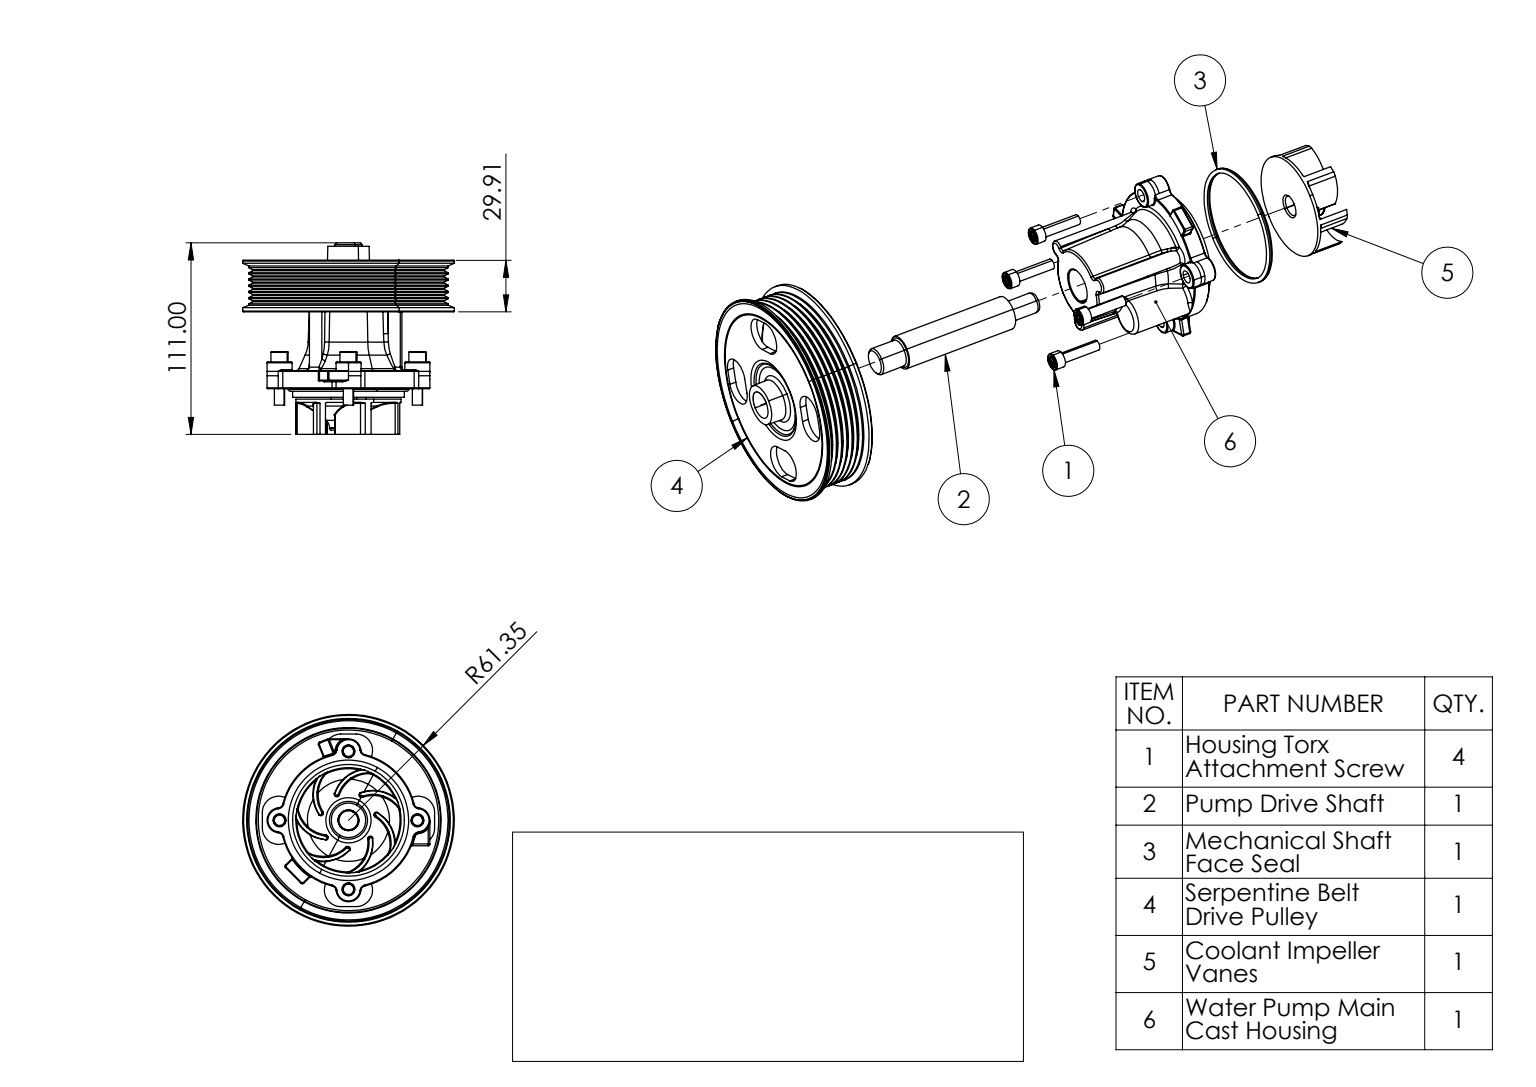
ISO-10303-21;
HEADER;
FILE_DESCRIPTION (('STEP AP214'),
    '1' );
FILE_NAME ('MAS-679',
    '2026-10-09T13:19:41',
    ( '' ),
    ( '' ),
    'SwSTEP 2.0',
    'SolidWorks 2026',
    '' );
FILE_SCHEMA (( 'AUTOMOTIVE_DESIGN' ));
ENDSEC;

DATA;
#1 = CARTESIAN_POINT ( 'NONE',  ( 13.86303783279999990, -99.69348480060000384, -10.38524229410000110 ) ) ;
#2 = DIRECTION ( 'NONE',  ( -1.000000000000000000, 0.000000000000000000, -1.110223024630000146E-15 ) ) ;
#3 = CARTESIAN_POINT ( 'NONE',  ( -4.209215656141860329, -99.16821844303207456, -18.57953415105935946 ) ) ;
#4 = CARTESIAN_POINT ( 'NONE',  ( 36.82697894980000086, -80.49999984420000487, -13.57704391360000074 ) ) ;
#5 = CARTESIAN_POINT ( 'NONE',  ( 11.49840686428493441, -72.20801872445015590, -27.07840416834825348 ) ) ;
#6 = CARTESIAN_POINT ( 'NONE',  ( -18.42950098929999925, -19.15770089200000115, 12.27996177870000061 ) ) ;
#7 = ORIENTED_EDGE ( 'NONE', *, *, #8559, .F. ) ;
#8 = CARTESIAN_POINT ( 'NONE',  ( 11.78548194719999920, -15.31994771319999948, 21.57317999869999881 ) ) ;
#9 = DIRECTION ( 'NONE',  ( 0.4377874319499604483, 0.000000000000000000, 0.8990785084889187928 ) ) ;
#10 = CARTESIAN_POINT ( 'NONE',  ( 6.195449712719999447, -93.01125874769999768, -25.86806793289999717 ) ) ;
#11 = DIRECTION ( 'NONE',  ( 0.000000000000000000, -1.000000000000000000, 0.000000000000000000 ) ) ;
#12 = CARTESIAN_POINT ( 'NONE',  ( -0.4517124965758896882, -92.59735406128710622, -30.49666433008702171 ) ) ;
#13 = APPLICATION_PROTOCOL_DEFINITION ( 'draft international standard', 'automotive_design', 1998, #17800 ) ;
#14 = CARTESIAN_POINT ( 'NONE',  ( 0.000000000000000000, -31.69999999999999929, 0.000000000000000000 ) ) ;
#15 = AXIS2_PLACEMENT_3D ( 'NONE', #13983, #16160, #22740 ) ;
#16 = CARTESIAN_POINT ( 'NONE',  ( 0.000000000000000000, -101.2530993010000060, 0.000000000000000000 ) ) ;
#17 = AXIS2_PLACEMENT_3D ( 'NONE', #8871, #7009, #22746 ) ;
#18 = CIRCLE ( 'NONE', #19870, 0.3500000000000003664 ) ;
#20 = ORIENTED_EDGE ( 'NONE', *, *, #20137, .T. ) ;
#19 = ADVANCED_FACE ( 'NONE', ( #21694 ), #5826, .T. ) ;
#21 = ADVANCED_FACE ( 'NONE', ( #16761 ), #3074, .F. ) ;
#22 = VERTEX_POINT ( 'NONE', #6246 ) ;
#23 = CARTESIAN_POINT ( 'NONE',  ( -13.70187146130000144, -57.41946977620000325, 20.98050236089999743 ) ) ;
#24 = CARTESIAN_POINT ( 'NONE',  ( -21.94602169939999925, -74.00000000000000000, -32.01791432939999993 ) ) ;
#25 = ORIENTED_EDGE ( 'NONE', *, *, #2852, .T. ) ;
#26 = CARTESIAN_POINT ( 'NONE',  ( -13.83118819819999956, -93.00000000000000000, 21.42307711379999802 ) ) ;
#27 = CARTESIAN_POINT ( 'NONE',  ( -6.649694310500000149, -97.57347470069998963, -20.16533349119999841 ) ) ;
#28 = CARTESIAN_POINT ( 'NONE',  ( 7.286238495500000134, -101.2500498790000023, 13.33737010350000141 ) ) ;
#29 = DIRECTION ( 'NONE',  ( 0.000000000000000000, -1.000000000000000000, 0.000000000000000000 ) ) ;
#30 = CARTESIAN_POINT ( 'NONE',  ( -7.249922261819999214, -74.00000000000000000, 40.03357376379999977 ) ) ;
#31 = DIRECTION ( 'NONE',  ( 0.4794255386042040601, 0.000000000000000000, 0.8775825618903720926 ) ) ;
#32 = CARTESIAN_POINT ( 'NONE',  ( 47.25000000000000000, -79.07667144713899177, -0.2614142261083034491 ) ) ;
#33 = ORIENTED_EDGE ( 'NONE', *, *, #25582, .F. ) ;
#34 = CARTESIAN_POINT ( 'NONE',  ( 6.962673371610000217, -93.00000450890000536, -28.64060071930000007 ) ) ;
#35 = CARTESIAN_POINT ( 'NONE',  ( 41.00000000000000000, -82.25000000000000000, -10.20110288159999890 ) ) ;
#36 = DIRECTION ( 'NONE',  ( 0.000000000000000000, 1.000000000000000000, 0.000000000000000000 ) ) ;
#37 = CARTESIAN_POINT ( 'NONE',  ( -13.16349300034329239, -92.74292563041959170, 27.51314017236756015 ) ) ;
#38 = ORIENTED_EDGE ( 'NONE', *, *, #11460, .T. ) ;
#39 = AXIS2_PLACEMENT_3D ( 'NONE', #26145, #6457, #10384 ) ;
#40 = CARTESIAN_POINT ( 'NONE',  ( -38.65569705749999940, -74.00000000000000000, 7.472970580910000216 ) ) ;
#41 = CARTESIAN_POINT ( 'NONE',  ( -14.41816450560000007, -92.76166464580001048, 26.16031912729999931 ) ) ;
#42 = DIRECTION ( 'NONE',  ( 0.4794255386042040601, 0.000000000000000000, 0.8775825618903719816 ) ) ;
#43 = ORIENTED_EDGE ( 'NONE', *, *, #10677, .T. ) ;
#44 = CONICAL_SURFACE ( 'NONE', #19544, 55.67692378859999280, 1.047197551199999799 ) ;
#45 = DIRECTION ( 'NONE',  ( 0.000000000000000000, -1.000000000000000000, 0.000000000000000000 ) ) ;
#46 = CONICAL_SURFACE ( 'NONE', #14894, 2.000000000000000888, 1.308996938999999804 ) ;
#47 = EDGE_CURVE ( 'NONE', #418, #1224, #23072, .T. ) ;
#48 = CARTESIAN_POINT ( 'NONE',  ( 0.8512941674849999751, -100.5027207520000019, -16.22949194299999931 ) ) ;
#49 = CARTESIAN_POINT ( 'NONE',  ( 7.691676892869999449, -59.03425911290000272, -22.18797527670000136 ) ) ;
#50 = CARTESIAN_POINT ( 'NONE',  ( -12.44168150949999863, -68.42644193349998716, -23.76792160109999585 ) ) ;
#51 = CARTESIAN_POINT ( 'NONE',  ( 23.24173891719999929, -63.62917541130000387, -7.733004683649999045 ) ) ;
#52 = CARTESIAN_POINT ( 'NONE',  ( 26.61465604159999998, -68.28989644159999273, 0.1578853838729999959 ) ) ;
#53 = CARTESIAN_POINT ( 'NONE',  ( 40.75609756099999714, -80.50000000000000000, -7.713029007999999465 ) ) ;
#54 = VERTEX_POINT ( 'NONE', #28244 ) ;
#55 = ADVANCED_FACE ( 'NONE', ( #15109 ), #24277, .F. ) ;
#56 = CARTESIAN_POINT ( 'NONE',  ( 28.37844821513105131, -92.77481473400868595, 11.17671000879152565 ) ) ;
#57 = FACE_OUTER_BOUND ( 'NONE', #7313, .T. ) ;
#58 = CARTESIAN_POINT ( 'NONE',  ( -4.347883707720000324, -95.85308664729998895, 22.07540195419999662 ) ) ;
#59 = ORIENTED_EDGE ( 'NONE', *, *, #8938, .T. ) ;
#60 = AXIS2_PLACEMENT_3D ( 'NONE', #11546, #27165, #75 ) ;
#61 = CARTESIAN_POINT ( 'NONE',  ( 23.72908286170881098, -92.68577957607949713, -19.16202722645927281 ) ) ;
#62 = CARTESIAN_POINT ( 'NONE',  ( 18.43702196799999982, -93.96464232210000489, 16.73647664110000122 ) ) ;
#63 = CIRCLE ( 'NONE', #7047, 3.000000000000002665 ) ;
#64 = CIRCLE ( 'NONE', #16341, 0.3500000000000003664 ) ;
#65 = CARTESIAN_POINT ( 'NONE',  ( 19.49531202280000031, -22.51609091130000095, -8.976487791660000326 ) ) ;
#66 = CARTESIAN_POINT ( 'NONE',  ( 22.75333808661257606, -19.47282734142590499, 1.034408943893888599 ) ) ;
#67 = CARTESIAN_POINT ( 'NONE',  ( -7.081475122079999629, -101.0678230150000019, 14.15032671260000008 ) ) ;
#68 = ORIENTED_EDGE ( 'NONE', *, *, #28286, .T. ) ;
#69 = CARTESIAN_POINT ( 'NONE',  ( 26.87524702870645044, -72.43548166874914784, -11.03468220454692883 ) ) ;
#70 = CARTESIAN_POINT ( 'NONE',  ( -13.19299550116862640, -100.0559847774924549, -11.12607270767140477 ) ) ;
#71 = CARTESIAN_POINT ( 'NONE',  ( 8.702528184260000188, -36.35983078039999583, -21.11894135150000196 ) ) ;
#72 = CARTESIAN_POINT ( 'NONE',  ( -37.59243475499999931, -65.56519245710001087, -0.6307174998519999853 ) ) ;
#73 = PLANE ( 'NONE',  #14194 ) ;
#74 = CARTESIAN_POINT ( 'NONE',  ( 22.07903221200000132, -19.15751145089999952, 0.09883320182290000755 ) ) ;
#75 = DIRECTION ( 'NONE',  ( 1.000000000000000000, 0.000000000000000000, 0.000000000000000000 ) ) ;
#76 = DIRECTION ( 'NONE',  ( 0.4794255386042042266, 0.000000000000000000, 0.8775825618903720926 ) ) ;
#77 = VERTEX_POINT ( 'NONE', #6989 ) ;
#78 = CARTESIAN_POINT ( 'NONE',  ( 11.12836528380000090, -101.0356131030000029, -10.75380786670000077 ) ) ;
#79 = CARTESIAN_POINT ( 'NONE',  ( 16.21749840157504963, -94.69376227371040500, 17.23632262694635386 ) ) ;
#80 = CARTESIAN_POINT ( 'NONE',  ( 7.120909764619999412E-15, -73.00000000000000000, 40.00000000000000000 ) ) ;
#81 = EDGE_CURVE ( 'NONE', #22088, #1149, #28672, .T. ) ;
#82 = CARTESIAN_POINT ( 'NONE',  ( 26.66586753799999698, -92.50000000000000000, 13.56661073689999952 ) ) ;
#83 = FACE_OUTER_BOUND ( 'NONE', #27486, .T. ) ;
#84 = DIRECTION ( 'NONE',  ( 1.000000000000000000, 0.000000000000000000, 0.000000000000000000 ) ) ;
#85 = CARTESIAN_POINT ( 'NONE',  ( 21.68645939410062340, -94.27895761509498129, 13.53905968357343781 ) ) ;
#86 = TOROIDAL_SURFACE ( 'NONE', #19140, 38.75000000000000000, 0.5000000000000000000 ) ;
#87 = VERTEX_POINT ( 'NONE', #24762 ) ;
#88 = CIRCLE ( 'NONE', #11209, 30.50000000000000000 ) ;
#89 = CARTESIAN_POINT ( 'NONE',  ( 36.71918983540000880, -74.79610922010000706, -14.73254090590000054 ) ) ;
#90 = VECTOR ( 'NONE', #20251, 1000.000000000000000 ) ;
#91 = EDGE_CURVE ( 'NONE', #19757, #9289, #15248, .T. ) ;
#92 = EDGE_LOOP ( 'NONE', ( #10026, #14439, #14720, #4638 ) ) ;
#93 = CARTESIAN_POINT ( 'NONE',  ( -13.96596450430000047, -64.58097845250000546, 21.73803617189999926 ) ) ;
#94 = CARTESIAN_POINT ( 'NONE',  ( 7.237400523855146872, -74.28469014324819852, 40.42867112560485054 ) ) ;
#95 = CARTESIAN_POINT ( 'NONE',  ( -26.59811871830000030, -93.01125874769999768, -0.2839302173490000358 ) ) ;
#96 = CARTESIAN_POINT ( 'NONE',  ( 27.02683049547185234, -19.50000000000000000, 2.817888817433860993 ) ) ;
#97 = CARTESIAN_POINT ( 'NONE',  ( -13.14566783280000095, -99.53431386179998697, -11.42099844400000030 ) ) ;
#98 = FACE_OUTER_BOUND ( 'NONE', #13994, .T. ) ;
#99 = EDGE_LOOP ( 'NONE', ( #14663, #18599, #4684, #25899 ) ) ;
#100 = CIRCLE ( 'NONE', #13575, 52.20000000000000284 ) ;
#101 = B_SPLINE_CURVE_WITH_KNOTS ( 'NONE', 5,
 ( #4962, #12492, #15099, #10442, #8409, #5814 ),
 .UNSPECIFIED., .F., .F.,
 ( 6, 6 ),
 ( 0.000000000000000000, 1.000000000000000000 ),
 .UNSPECIFIED. ) ;
#102 = CARTESIAN_POINT ( 'NONE',  ( 7.432628554159999013, -73.95638562449998687, -39.04162410920000070 ) ) ;
#103 = VERTEX_POINT ( 'NONE', #2623 ) ;
#104 = AXIS2_PLACEMENT_3D ( 'NONE', #11589, #3684, #25016 ) ;
#105 = DIRECTION ( 'NONE',  ( -0.7071067811865457964, 0.000000000000000000, -0.7071067811865492381 ) ) ;
#106 = ORIENTED_EDGE ( 'NONE', *, *, #502, .T. ) ;
#107 = CARTESIAN_POINT ( 'NONE',  ( -16.95867319479999935, -74.50000000000000000, 44.10460184009999551 ) ) ;
#108 = B_SPLINE_CURVE_WITH_KNOTS ( 'NONE', 3,
 ( #24628, #17928, #4072, #26234, #6261, #26822 ),
 .UNSPECIFIED., .F., .F.,
 ( 4, 2, 4 ),
 ( 0.000000000000000000, 0.5000000000000000000, 1.000000000000000000 ),
 .UNSPECIFIED. ) ;
#109 = CARTESIAN_POINT ( 'NONE',  ( -40.50000000000000000, -63.30468293320000583, -2.309401076760000393 ) ) ;
#110 = CARTESIAN_POINT ( 'NONE',  ( -10.71874886979999886, -18.50000000000000000, -18.09957584549999865 ) ) ;
#111 = PLANE ( 'NONE',  #8405 ) ;
#112 = CARTESIAN_POINT ( 'NONE',  ( 24.26002557130000170, -94.09272382170000526, -9.010767759849999337 ) ) ;
#113 = CARTESIAN_POINT ( 'NONE',  ( -13.91698628299999996, -74.00000000000000000, 36.28539016370000070 ) ) ;
#114 = FACE_OUTER_BOUND ( 'NONE', #18535, .T. ) ;
#115 = CARTESIAN_POINT ( 'NONE',  ( -16.09522089960879399, -99.28262727489575923, 7.457865879375452423 ) ) ;
#116 = B_SPLINE_SURFACE_WITH_KNOTS ( 'NONE', 5, 5, ( 
 ( #14625, #23526, #3562, #12417, #21334, #1390 ),
 ( #10232, #9826, #23801, #19147, #20920, #18734 ),
 ( #5874, #28035, #8074, #16964, #25852, #14753 ),
 ( #26709, #28718, #17525, #19703, #28300, #6299 ),
 ( #19988, #58, #13133, #10789, #8906, #15459 ),
 ( #11070, #6601, #22187, #4412, #6443, #17235 ) ),
 .UNSPECIFIED., .F., .F., .F.,
 ( 6, 6 ),
 ( 6, 6 ),
 ( 15.82769160610000014, 30.79604198849999719 ),
 ( 0.000000000000000000, 0.5000000000000000000 ),
 .UNSPECIFIED. ) ;
#117 = ORIENTED_EDGE ( 'NONE', *, *, #9091, .F. ) ;
#118 = CARTESIAN_POINT ( 'NONE',  ( -15.38823321699999980, -101.6484610359999863, 4.383952149800000697 ) ) ;
#119 = CYLINDRICAL_SURFACE ( 'NONE', #23798, 4.999999999999999112 ) ;
#120 = DIRECTION ( 'NONE',  ( 0.000000000000000000, -1.000000000000000000, 0.000000000000000000 ) ) ;
#121 = PRODUCT_DEFINITION ( 'UNKNOWN', '', #18568, #21393 ) ;
#122 = CARTESIAN_POINT ( 'NONE',  ( 20.98382983661468160, -19.47636826822539646, 9.463978915456744190 ) ) ;
#123 = CARTESIAN_POINT ( 'NONE',  ( 23.35514555854173224, -63.53090568636451962, -7.475128354575953260 ) ) ;
#124 = ORIENTED_EDGE ( 'NONE', *, *, #22234, .T. ) ;
#125 = ADVANCED_FACE ( 'NONE', ( #15853 ), #9081, .F. ) ;
#126 = CARTESIAN_POINT ( 'NONE',  ( 26.73456646982424445, -92.62800705135703083, -14.68054035958608772 ) ) ;
#127 = CARTESIAN_POINT ( 'NONE',  ( -32.18237743670000128, -74.02983596709999858, -21.99383679990000218 ) ) ;
#128 = ORIENTED_EDGE ( 'NONE', *, *, #22826, .F. ) ;
#129 = EDGE_CURVE ( 'NONE', #4293, #10101, #28625, .T. ) ;
#130 = EDGE_CURVE ( 'NONE', #14037, #19059, #13032, .T. ) ;
#131 = CARTESIAN_POINT ( 'NONE',  ( -16.95867319479999935, -79.50000000000000000, 44.10460184009999551 ) ) ;
#132 = CARTESIAN_POINT ( 'NONE',  ( 19.86285231560000142, -35.99517856170000130, -9.398749189900000189 ) ) ;
#133 = CARTESIAN_POINT ( 'NONE',  ( -35.88566914520000495, -79.50000000000000000, -26.69328098980000163 ) ) ;
#134 = VERTEX_POINT ( 'NONE', #18050 ) ;
#135 = ORIENTED_EDGE ( 'NONE', *, *, #7062, .T. ) ;
#136 = CARTESIAN_POINT ( 'NONE',  ( -40.00000000000000000, -69.00000000000000000, 0.000000000000000000 ) ) ;
#137 = CARTESIAN_POINT ( 'NONE',  ( 25.95077523760000204, -92.66001738319999959, 10.56845450099999972 ) ) ;
#138 = CARTESIAN_POINT ( 'NONE',  ( 30.45033996220000105, -72.00000000000000000, 1.805359716810000181 ) ) ;
#139 = VERTEX_POINT ( 'NONE', #26948 ) ;
#140 = CARTESIAN_POINT ( 'NONE',  ( -39.22207447329392238, -63.24690319806988725, -2.469861454400793299 ) ) ;
#141 = CARTESIAN_POINT ( 'NONE',  ( -22.28727701460000077, -80.19684096389998729, -32.37890396869999421 ) ) ;
#142 = TOROIDAL_SURFACE ( 'NONE', #23843, 43.34897771020000334, 20.00000000000000000 ) ;
#143 = AXIS2_PLACEMENT_3D ( 'NONE', #11532, #26560, #20442 ) ;
#144 = LINE ( 'NONE', #2612, #25776 ) ;
#145 = CARTESIAN_POINT ( 'NONE',  ( -12.45428620100000039, -94.22485739629999557, -21.30780079690000406 ) ) ;
#146 = AXIS2_PLACEMENT_3D ( 'NONE', #12009, #28037, #9963 ) ;
#147 = ORIENTED_EDGE ( 'NONE', *, *, #2522, .F. ) ;
#148 = DIRECTION ( 'NONE',  ( 0.000000000000000000, 1.000000000000000000, 0.000000000000000000 ) ) ;
#149 = CARTESIAN_POINT ( 'NONE',  ( -17.00715350810000004, -99.92967567080000890, 3.484608414699999823 ) ) ;
#150 = DIRECTION ( 'NONE',  ( 0.000000000000000000, -1.000000000000000000, 0.000000000000000000 ) ) ;
#151 = CARTESIAN_POINT ( 'NONE',  ( -21.99783282880000002, -74.36373701399999447, -32.65606203760000170 ) ) ;
#152 = DIRECTION ( 'NONE',  ( 0.4794255386042040601, 0.000000000000000000, 0.8775825618903720926 ) ) ;
#153 = CARTESIAN_POINT ( 'NONE',  ( -27.04683438039999999, -80.00000000000000000, -36.23922253580000330 ) ) ;
#154 = CARTESIAN_POINT ( 'NONE',  ( 0.9512194931930000319, -99.70407914540000149, -17.16990763940000164 ) ) ;
#155 = CARTESIAN_POINT ( 'NONE',  ( -18.45398243510000214, -18.61794786970000359, 11.31880357350000033 ) ) ;
#156 = ORIENTED_EDGE ( 'NONE', *, *, #2664, .T. ) ;
#157 = EDGE_CURVE ( 'NONE', #20862, #20652, #26784, .T. ) ;
#158 = CARTESIAN_POINT ( 'NONE',  ( -7.593124578350000320, -94.98812656910000385, -22.45811535680000048 ) ) ;
#159 = CIRCLE ( 'NONE', #18770, 16.00000000000000000 ) ;
#160 = CARTESIAN_POINT ( 'NONE',  ( 9.189959902346380716, -37.98173178281364670, -22.48186365736571801 ) ) ;
#161 = CARTESIAN_POINT ( 'NONE',  ( -23.83924287751435500, -92.80442066021429071, -19.02474555443098936 ) ) ;
#162 = DIRECTION ( 'NONE',  ( 0.000000000000000000, 1.000000000000000000, 0.000000000000000000 ) ) ;
#163 = CARTESIAN_POINT ( 'NONE',  ( -38.62700573890000300, -65.19264941160000149, 2.813424548380000001 ) ) ;
#164 = CARTESIAN_POINT ( 'NONE',  ( -14.62576901236522886, -101.1449112445098564, 4.605366063130757581 ) ) ;
#165 = ADVANCED_FACE ( 'NONE', ( #26356 ), #6385, .F. ) ;
#166 = DIRECTION ( 'NONE',  ( 0.000000000000000000, 0.000000000000000000, 1.000000000000000000 ) ) ;
#167 = CIRCLE ( 'NONE', #27093, 2.000000000000001776 ) ;
#168 = B_SPLINE_CURVE_WITH_KNOTS ( 'NONE', 3,
 ( #1213, #18961, #8023, #3928, #12792, #23335 ),
 .UNSPECIFIED., .F., .F.,
 ( 4, 2, 4 ),
 ( 0.000000000000000000, 0.5000000000000000000, 1.000000000000000000 ),
 .UNSPECIFIED. ) ;
#169 = DIRECTION ( 'NONE',  ( 0.000000000000000000, 1.000000000000000000, 0.000000000000000000 ) ) ;
#170 = CIRCLE ( 'NONE', #22027, 0.8000000000000003775 ) ;
#171 = CARTESIAN_POINT ( 'NONE',  ( 0.000000000000000000, -37.50000000000000000, 0.000000000000000000 ) ) ;
#172 = ORIENTED_EDGE ( 'NONE', *, *, #20476, .T. ) ;
#173 = CARTESIAN_POINT ( 'NONE',  ( 5.151434834259999649E-15, -84.50000000000000000, 40.00000000000000000 ) ) ;
#174 = DIRECTION ( 'NONE',  ( 0.4794255386042042266, 0.000000000000000000, 0.8775825618903720926 ) ) ;
#175 = EDGE_LOOP ( 'NONE', ( #20884, #12154, #22401, #5530, #9489 ) ) ;
#176 = CARTESIAN_POINT ( 'NONE',  ( -12.68423258129999986, -57.45864775709999606, 20.28109956510000345 ) ) ;
#177 = DIRECTION ( 'NONE',  ( 0.000000000000000000, 1.000000000000000000, 0.000000000000000000 ) ) ;
#178 = VERTEX_POINT ( 'NONE', #329 ) ;
#179 = CARTESIAN_POINT ( 'NONE',  ( 16.44117324919999845, -94.63960161729998788, 17.12038106740000032 ) ) ;
#180 = CIRCLE ( 'NONE', #4826, 30.50000000000000000 ) ;
#181 = CARTESIAN_POINT ( 'NONE',  ( 7.155402402981435372, -93.74885977083570765, -25.65720728536609840 ) ) ;
#182 = CARTESIAN_POINT ( 'NONE',  ( -24.61280144410000048, -93.91547326130000783, -2.656926711870000180 ) ) ;
#183 = CARTESIAN_POINT ( 'NONE',  ( 0.000000000000000000, 4.440892098500000496E-16, 0.000000000000000000 ) ) ;
#184 = CARTESIAN_POINT ( 'NONE',  ( -11.05730518689999897, -18.50000000000000000, -18.25363368680000065 ) ) ;
#185 = CARTESIAN_POINT ( 'NONE',  ( 11.60289000694941208, -98.08323605844854853, -16.85433682801441435 ) ) ;
#186 = ORIENTED_EDGE ( 'NONE', *, *, #11011, .T. ) ;
#187 = FACE_OUTER_BOUND ( 'NONE', #28080, .T. ) ;
#188 = DIRECTION ( 'NONE',  ( 0.4794255386042000078, 0.000000000000000000, 0.8775825618903743131 ) ) ;
#189 = CARTESIAN_POINT ( 'NONE',  ( -12.62382144519470906, -92.54938211474033949, 27.76503023812927395 ) ) ;
#190 = ORIENTED_EDGE ( 'NONE', *, *, #2721, .F. ) ;
#191 = EDGE_CURVE ( 'NONE', #3233, #22412, #10451, .T. ) ;
#192 = DIRECTION ( 'NONE',  ( 1.000000000000000000, 0.000000000000000000, 0.000000000000000000 ) ) ;
#193 = CARTESIAN_POINT ( 'NONE',  ( 0.000000000000000000, -23.00000000000000000, 0.000000000000000000 ) ) ;
#194 = CARTESIAN_POINT ( 'NONE',  ( 4.794255386040000566, -108.5000000000000000, 8.775825618900000791 ) ) ;
#195 = ORIENTED_EDGE ( 'NONE', *, *, #12887, .F. ) ;
#196 = EDGE_CURVE ( 'NONE', #27670, #21621, #4916, .T. ) ;
#197 = CARTESIAN_POINT ( 'NONE',  ( 27.03525773600000193, -69.21553441180000732, 0.3672064477150000505 ) ) ;
#198 = CARTESIAN_POINT ( 'NONE',  ( 1.100347978140000071, -100.4792519539999915, -16.15648718290000119 ) ) ;
#199 = CARTESIAN_POINT ( 'NONE',  ( 26.01146028782885011, -74.32246178234187539, -29.34981677889942375 ) ) ;
#200 = CARTESIAN_POINT ( 'NONE',  ( 21.14593590499999820, -36.00000000000000000, -10.72085360310000013 ) ) ;
#201 = EDGE_CURVE ( 'NONE', #9396, #9232, #7255, .T. ) ;
#202 = CARTESIAN_POINT ( 'NONE',  ( -11.49099129190000035, -57.47122623430000488, -20.56185124510000151 ) ) ;
#203 = EDGE_CURVE ( 'NONE', #6901, #22316, #21214, .T. ) ;
#204 = AXIS2_PLACEMENT_3D ( 'NONE', #18687, #25805, #7624 ) ;
#205 = B_SPLINE_CURVE_WITH_KNOTS ( 'NONE', 3,
 ( #6928, #20469, #27325, #4883 ),
 .UNSPECIFIED., .F., .F.,
 ( 4, 4 ),
 ( 0.000000000000000000, 1.000000000000000000 ),
 .UNSPECIFIED. ) ;
#206 = FACE_OUTER_BOUND ( 'NONE', #10971, .T. ) ;
#207 = AXIS2_PLACEMENT_3D ( 'NONE', #10252, #6026, #27775 ) ;
#208 = CYLINDRICAL_SURFACE ( 'NONE', #19119, 0.5000000000000004441 ) ;
#209 = ORIENTED_EDGE ( 'NONE', *, *, #22626, .F. ) ;
#210 = DIRECTION ( 'NONE',  ( 0.000000000000000000, 1.000000000000000000, 0.000000000000000000 ) ) ;
#211 = CARTESIAN_POINT ( 'NONE',  ( 14.90405967080000060, -97.14975741390000508, 15.22359678429999974 ) ) ;
#212 = VERTEX_POINT ( 'NONE', #28690 ) ;
#213 = AXIS2_PLACEMENT_3D ( 'NONE', #15083, #23991, #4026 ) ;
#214 = CARTESIAN_POINT ( 'NONE',  ( 36.70830968599999977, -79.00000000000000000, -14.75000000000000000 ) ) ;
#215 = CARTESIAN_POINT ( 'NONE',  ( 18.38937822269999955, -93.75379239730000336, 16.85123465680000265 ) ) ;
#216 = CARTESIAN_POINT ( 'NONE',  ( 0.000000000000000000, -108.5000000000000000, 0.000000000000000000 ) ) ;
#217 = EDGE_CURVE ( 'NONE', #3543, #26971, #14750, .T. ) ;
#218 = FACE_OUTER_BOUND ( 'NONE', #16317, .T. ) ;
#219 = ORIENTED_EDGE ( 'NONE', *, *, #4229, .F. ) ;
#220 = CARTESIAN_POINT ( 'NONE',  ( -3.592524684419479364, -80.18584070972035249, 46.36824188645663014 ) ) ;
#221 = CARTESIAN_POINT ( 'NONE',  ( -12.45669907782013119, -101.5026031439933831, -10.21990696985948333 ) ) ;
#222 = CARTESIAN_POINT ( 'NONE',  ( 9.433208476599999059, -36.00000000000000000, -19.93952380609999864 ) ) ;
#223 = DIRECTION ( 'NONE',  ( 0.000000000000000000, 1.000000000000000000, 0.000000000000000000 ) ) ;
#224 = CARTESIAN_POINT ( 'NONE',  ( 7.375300558930000250, -99.32951138629999832, 16.07022401509999909 ) ) ;
#225 = AXIS2_PLACEMENT_3D ( 'NONE', #24981, #531, #7212 ) ;
#226 = DIRECTION ( 'NONE',  ( 0.000000000000000000, -1.000000000000000000, 0.000000000000000000 ) ) ;
#227 = CARTESIAN_POINT ( 'NONE',  ( 7.460698725479999927E-15, -73.50000000000000000, 40.00000000000000000 ) ) ;
#228 = AXIS2_PLACEMENT_3D ( 'NONE', #18983, #14038, #961 ) ;
#229 = CARTESIAN_POINT ( 'NONE',  ( 13.12744653600000078, -94.59276292389999696, -19.84842857619999990 ) ) ;
#230 = ORIENTED_EDGE ( 'NONE', *, *, #12077, .T. ) ;
#231 = CYLINDRICAL_SURFACE ( 'NONE', #19067, 8.099999999999997868 ) ;
#232 = CARTESIAN_POINT ( 'NONE',  ( -47.25000000000000000, -77.00000000000000000, 3.352534721190000231E-15 ) ) ;
#233 = CARTESIAN_POINT ( 'NONE',  ( 10.26951296328627450, -97.66504487118385214, 16.98417627201420643 ) ) ;
#234 = EDGE_CURVE ( 'NONE', #8501, #14143, #28325, .T. ) ;
#235 = CARTESIAN_POINT ( 'NONE',  ( 16.83483077069999823, -101.1889999979999999, 4.239603657359999112 ) ) ;
#236 = B_SPLINE_CURVE_WITH_KNOTS ( 'NONE', 5,
 ( #24946, #20125, #22766, #18392, #22315, #639, #13265, #8890, #20574 ),
 .UNSPECIFIED., .F., .F.,
 ( 6, 3, 6 ),
 ( 54.79316277730000451, 55.82679151939999684, 65.31895145690000959 ),
 .UNSPECIFIED. ) ;
#237 = CARTESIAN_POINT ( 'NONE',  ( 21.68248887209999864, -36.72282065030000098, -8.793944725010000241 ) ) ;
#238 = CARTESIAN_POINT ( 'NONE',  ( -13.11191196370000078, -67.01088404460000447, -22.48946444609999773 ) ) ;
#239 = AXIS2_PLACEMENT_3D ( 'NONE', #11995, #25424, #7660 ) ;
#240 = CARTESIAN_POINT ( 'NONE',  ( 14.95019707169999990, -101.2530993000000024, 2.710463435110000319 ) ) ;
#241 = CARTESIAN_POINT ( 'NONE',  ( 47.25000000000000000, -82.25000000000000000, 7.327133149349999745E-15 ) ) ;
#242 = ORIENTED_EDGE ( 'NONE', *, *, #1523, .T. ) ;
#243 = EDGE_CURVE ( 'NONE', #2786, #26473, #23537, .T. ) ;
#244 = DIRECTION ( 'NONE',  ( 1.000000000000000000, 0.000000000000000000, 0.000000000000000000 ) ) ;
#245 = CIRCLE ( 'NONE', #4394, 58.54999999999999716 ) ;
#246 = ORIENTED_EDGE ( 'NONE', *, *, #20790, .F. ) ;
#247 = CARTESIAN_POINT ( 'NONE',  ( -14.67079199249999988, -67.87586507669998070, 22.52608771310000080 ) ) ;
#248 = CARTESIAN_POINT ( 'NONE',  ( -14.08829788499999935, -63.05022673990000470, 21.64331597370000182 ) ) ;
#249 = CARTESIAN_POINT ( 'NONE',  ( 7.244026535080238638, -74.18384006186305157, 40.29424782664090543 ) ) ;
#250 = CIRCLE ( 'NONE', #27231, 57.75000000000000000 ) ;
#251 = B_SPLINE_CURVE_WITH_KNOTS ( 'NONE', 3,
 ( #2695, #18425, #27024, #971, #16075, #16523, #22510, #7208, #16373, #25420, #27617 ),
 .UNSPECIFIED., .F., .F.,
 ( 4, 2, 1, 2, 2, 4 ),
 ( 0.000000000000000000, 0.2499999999999618638, 0.3749999999999487632, 0.4374999999999482636, 0.4999999999999477085, 1.000000000000000000 ),
 .UNSPECIFIED. ) ;
#252 = CARTESIAN_POINT ( 'NONE',  ( 20.27618985420000186, -36.00000000000000000, -9.807089787700000727 ) ) ;
#253 = CARTESIAN_POINT ( 'NONE',  ( 19.26180799268026078, -18.95847994163547767, 10.44830257471190471 ) ) ;
#254 = CARTESIAN_POINT ( 'NONE',  ( -7.325370793560000315, -19.50000000000000000, -24.94672208400000102 ) ) ;
#255 = ADVANCED_FACE ( 'NONE', ( #17790 ), #18406, .F. ) ;
#256 = CARTESIAN_POINT ( 'NONE',  ( 20.51180957029163565, -19.46799463732224922, -8.054242869036199792 ) ) ;
#257 = CARTESIAN_POINT ( 'NONE',  ( 15.94061401059999916, -100.1275643909999928, 4.799433088389999824 ) ) ;
#258 = VERTEX_POINT ( 'NONE', #22459 ) ;
#259 = DIRECTION ( 'NONE',  ( 1.000000000000000000, 0.000000000000000000, 0.000000000000000000 ) ) ;
#260 = FILL_AREA_STYLE_COLOUR ( '', #13962 ) ;
#261 = CARTESIAN_POINT ( 'NONE',  ( -19.90122868539999956, -97.01677120260001175, -7.153572992790000029 ) ) ;
#262 = ORIENTED_EDGE ( 'NONE', *, *, #10555, .F. ) ;
#263 = CARTESIAN_POINT ( 'NONE',  ( -30.47294111744043832, -92.56492639277982448, 1.288063236097679587 ) ) ;
#264 = LINE ( 'NONE', #16101, #15060 ) ;
#265 = CARTESIAN_POINT ( 'NONE',  ( 0.000000000000000000, -26.90310889129999694, 0.000000000000000000 ) ) ;
#266 = CIRCLE ( 'NONE', #3945, 6.749999999999999112 ) ;
#267 = CARTESIAN_POINT ( 'NONE',  ( 20.31209251039999941, -39.36414254479999641, 10.36558011049999983 ) ) ;
#268 = LINE ( 'NONE', #1996, #17176 ) ;
#269 = CARTESIAN_POINT ( 'NONE',  ( -7.237400523910141104, -74.28469014252485181, -40.42867112467618540 ) ) ;
#270 = CARTESIAN_POINT ( 'NONE',  ( 19.55635611740000002, -19.15716910929999628, 10.13489318640000114 ) ) ;
#271 = CARTESIAN_POINT ( 'NONE',  ( -32.83566817454328657, -79.62152845406559720, -22.22906645665674219 ) ) ;
#272 = CARTESIAN_POINT ( 'NONE',  ( -17.52930755215682268, -96.09960287657678180, 13.04485788190981488 ) ) ;
#273 = ORIENTED_EDGE ( 'NONE', *, *, #13276, .F. ) ;
#274 = DIRECTION ( 'NONE',  ( 0.000000000000000000, -1.000000000000000000, 0.000000000000000000 ) ) ;
#275 = CARTESIAN_POINT ( 'NONE',  ( -3.794472973536972216, -98.68740021267650775, 19.30576947772378560 ) ) ;
#276 = CARTESIAN_POINT ( 'NONE',  ( -12.75146816829999885, -100.4650220110000021, -10.99189795709999906 ) ) ;
#277 = CARTESIAN_POINT ( 'NONE',  ( 21.85414229151949073, -19.48999941750866327, 9.596093625701307417 ) ) ;
#278 = CARTESIAN_POINT ( 'NONE',  ( 22.95684285356151122, -62.19234181365079195, -7.315910207710417446 ) ) ;
#279 = ORIENTED_EDGE ( 'NONE', *, *, #17232, .T. ) ;
#280 = CARTESIAN_POINT ( 'NONE',  ( -37.29988270759999835, -74.00000000000000000, -26.69328098980000163 ) ) ;
#281 = ORIENTED_EDGE ( 'NONE', *, *, #28769, .F. ) ;
#282 = CARTESIAN_POINT ( 'NONE',  ( -1.332267629549999902E-15, -101.6484611540000031, 3.552713678799999608E-15 ) ) ;
#283 = CARTESIAN_POINT ( 'NONE',  ( 0.3059185938709999553, -101.1889999979999999, 14.72672055670000013 ) ) ;
#284 = CARTESIAN_POINT ( 'NONE',  ( 10.50737348100000013, -92.95010077049998642, 27.57035790109999596 ) ) ;
#285 = ORIENTED_EDGE ( 'NONE', *, *, #19460, .T. ) ;
#286 = B_SPLINE_CURVE_WITH_KNOTS ( 'NONE', 3,
 ( #13483, #9260, #22391, #17872, #13330, #22237 ),
 .UNSPECIFIED., .F., .F.,
 ( 4, 2, 4 ),
 ( 0.000000000000000000, 0.5000000000000000000, 1.000000000000000000 ),
 .UNSPECIFIED. ) ;
#287 = EDGE_CURVE ( 'NONE', #8306, #13803, #18426, .T. ) ;
#288 = EDGE_LOOP ( 'NONE', ( #10036, #21342, #22222, #19692, #5253 ) ) ;
#289 = CARTESIAN_POINT ( 'NONE',  ( -27.35150891653901084, -93.48480241393187384, -0.1005241429990150898 ) ) ;
#290 = CARTESIAN_POINT ( 'NONE',  ( 19.72730657420000000, -94.57749572790000059, 14.01459989379999982 ) ) ;
#291 = DIRECTION ( 'NONE',  ( 0.000000000000000000, -1.000000000000000000, 0.000000000000000000 ) ) ;
#292 = ORIENTED_EDGE ( 'NONE', *, *, #16592, .T. ) ;
#293 = DIRECTION ( 'NONE',  ( 0.9704142011833033488, 0.000000000000000000, -0.2414462220490755373 ) ) ;
#294 = CARTESIAN_POINT ( 'NONE',  ( -25.34933364415341472, -93.66270333196791853, -5.750320990542998167 ) ) ;
#295 = EDGE_CURVE ( 'NONE', #9549, #16619, #7522, .T. ) ;
#296 = DIRECTION ( 'NONE',  ( -0.2162432783070587228, 0.000000000000000000, -0.9763395129702658881 ) ) ;
#297 = EDGE_CURVE ( 'NONE', #22756, #7089, #25863, .T. ) ;
#298 = CARTESIAN_POINT ( 'NONE',  ( -12.52668430659999999, -94.45168166330000759, -21.51447599709999992 ) ) ;
#299 = CARTESIAN_POINT ( 'NONE',  ( -24.12300379919877713, -94.89420224095245260, -4.133214399626305102 ) ) ;
#300 = VERTEX_POINT ( 'NONE', #17646 ) ;
#301 = EDGE_CURVE ( 'NONE', #178, #23662, #773, .T. ) ;
#302 = CARTESIAN_POINT ( 'NONE',  ( -15.53338745080000116, -84.25000000000000000, -28.43367500519999780 ) ) ;
#303 = CARTESIAN_POINT ( 'NONE',  ( -16.99615325119999909, -99.69348474340000621, 3.341833029000000010 ) ) ;
#304 = CARTESIAN_POINT ( 'NONE',  ( 0.000000000000000000, -18.50000000000000000, 0.000000000000000000 ) ) ;
#305 = CARTESIAN_POINT ( 'NONE',  ( -21.75993564049999662, -74.26505820949999759, -32.61013845149999923 ) ) ;
#306 = CARTESIAN_POINT ( 'NONE',  ( -9.444188748147608337, -96.12507615671063377, -21.04386775914182905 ) ) ;
#307 = DIRECTION ( 'NONE',  ( 0.000000000000000000, 1.000000000000000000, 0.000000000000000000 ) ) ;
#308 = CARTESIAN_POINT ( 'NONE',  ( 0.5505338958400000093, -101.0875971110000080, -15.39929819530000010 ) ) ;
#309 = EDGE_LOOP ( 'NONE', ( #11613, #26788, #16517, #882 ) ) ;
#310 = CARTESIAN_POINT ( 'NONE',  ( -11.92805169729999903, -93.25168459629999518, -23.54816055649999740 ) ) ;
#311 = CARTESIAN_POINT ( 'NONE',  ( 23.49021206360000136, -61.37513324760000444, 10.53893526849999951 ) ) ;
#312 = DIRECTION ( 'NONE',  ( 0.9952295494196654602, 0.000000000000000000, -0.09756097560976667582 ) ) ;
#313 = CARTESIAN_POINT ( 'NONE',  ( -23.96181287727355880, -92.68577957613881324, -18.87019301755865186 ) ) ;
#314 = DIRECTION ( 'NONE',  ( 0.000000000000000000, -1.000000000000000000, 0.000000000000000000 ) ) ;
#315 = CARTESIAN_POINT ( 'NONE',  ( 47.13373881900000129, -79.60558632359999365, -1.850014393339999952 ) ) ;
#316 = AXIS2_PLACEMENT_3D ( 'NONE', #22770, #793, #16190 ) ;
#317 =( NAMED_UNIT ( * ) SI_UNIT ( $, .STERADIAN. ) SOLID_ANGLE_UNIT ( ) );
#318 = CARTESIAN_POINT ( 'NONE',  ( 0.000000000000000000, -11.00000000000000000, 0.000000000000000000 ) ) ;
#319 = ORIENTED_EDGE ( 'NONE', *, *, #5451, .T. ) ;
#320 = CARTESIAN_POINT ( 'NONE',  ( 17.35878545119999927, -99.60591458940000109, 0.7490350149880000696 ) ) ;
#321 = VERTEX_POINT ( 'NONE', #13849 ) ;
#322 = CARTESIAN_POINT ( 'NONE',  ( 22.48431106502128785, -26.11410610478370131, 9.982359961558207928 ) ) ;
#323 = CARTESIAN_POINT ( 'NONE',  ( 32.39999999999999858, -89.50000000000000000, 3.967724586379999025E-15 ) ) ;
#324 = ORIENTED_EDGE ( 'NONE', *, *, #4162, .T. ) ;
#325 = CARTESIAN_POINT ( 'NONE',  ( 0.000000000000000000, -102.8486084350000027, 0.000000000000000000 ) ) ;
#326 = DIRECTION ( 'NONE',  ( 1.000000000000000000, 0.000000000000000000, 0.000000000000000000 ) ) ;
#327 = EDGE_CURVE ( 'NONE', #28629, #9768, #11659, .T. ) ;
#328 = CARTESIAN_POINT ( 'NONE',  ( 4.957296131405555251, -93.25521310932876418, -27.72106811766053980 ) ) ;
#329 = CARTESIAN_POINT ( 'NONE',  ( 32.25000000000000000, -74.00000000000000000, 1.484822157706350179E-15 ) ) ;
#330 = DIRECTION ( 'NONE',  ( -0.9993816408608721114, 0.000000000000000000, 0.03516156865429608674 ) ) ;
#331 = EDGE_CURVE ( 'NONE', #2214, #4550, #8167, .T. ) ;
#332 = CARTESIAN_POINT ( 'NONE',  ( -10.44633092189999957, -19.46971296670000129, -20.02005348129999973 ) ) ;
#333 = ORIENTED_EDGE ( 'NONE', *, *, #19304, .T. ) ;
#334 = ADVANCED_FACE ( 'NONE', ( #7744 ), #22137, .T. ) ;
#335 = CARTESIAN_POINT ( 'NONE',  ( 7.189062418559999834, -92.50000460620000808, -28.89817089330000144 ) ) ;
#336 = CARTESIAN_POINT ( 'NONE',  ( -20.38472824830307317, -61.37133910092857292, 12.44426916512128223 ) ) ;
#337 = CARTESIAN_POINT ( 'NONE',  ( -13.21000303337382675, -92.77521214512354675, 27.49085673672507468 ) ) ;
#338 = ORIENTED_EDGE ( 'NONE', *, *, #4914, .F. ) ;
#339 = CARTESIAN_POINT ( 'NONE',  ( -38.15937129994918564, -63.35495516230771074, -1.162516276375642921 ) ) ;
#340 = CARTESIAN_POINT ( 'NONE',  ( -15.46453744689999965, -92.60980597189998775, 23.68301408729999835 ) ) ;
#341 = CARTESIAN_POINT ( 'NONE',  ( -22.62548402540000225, -71.48510949040000639, 17.99032368389999803 ) ) ;
#342 = ORIENTED_EDGE ( 'NONE', *, *, #9374, .T. ) ;
#343 = CARTESIAN_POINT ( 'NONE',  ( -17.63662366879999865, -94.54719310779999830, 16.06392309460000334 ) ) ;
#344 = CARTESIAN_POINT ( 'NONE',  ( 0.9125455711469999676, -100.1785804069999983, -16.62377051789999882 ) ) ;
#345 = CARTESIAN_POINT ( 'NONE',  ( 25.28766026403006961, -74.25610482756999886, -29.93611247388432162 ) ) ;
#346 = CARTESIAN_POINT ( 'NONE',  ( -19.90266458460165566, -57.44036973094087273, 14.20824301555132152 ) ) ;
#347 = CARTESIAN_POINT ( 'NONE',  ( 22.71963930829999967, -57.44066855169999997, -9.099147364980002095 ) ) ;
#348 = CARTESIAN_POINT ( 'NONE',  ( 6.888451995309999631, -99.53431386179998697, 15.99365561480000153 ) ) ;
#349 = ORIENTED_EDGE ( 'NONE', *, *, #6891, .T. ) ;
#350 = CARTESIAN_POINT ( 'NONE',  ( -17.51528407220000361, -94.37182379849998881, 16.53944417690000179 ) ) ;
#351 = CARTESIAN_POINT ( 'NONE',  ( 15.38595020189201179, -101.1586404113103015, 2.789465265516761772 ) ) ;
#352 = EDGE_CURVE ( 'NONE', #18033, #14401, #4448, .T. ) ;
#353 = CARTESIAN_POINT ( 'NONE',  ( 19.89028060919999774, -94.80026829410000744, 14.17835456439999930 ) ) ;
#354 = ORIENTED_EDGE ( 'NONE', *, *, #12243, .F. ) ;
#355 = CARTESIAN_POINT ( 'NONE',  ( 23.48150327141549099, -92.56772982771099123, -19.46465348493570957 ) ) ;
#356 = DIRECTION ( 'NONE',  ( 0.000000000000000000, 1.000000000000000000, 0.000000000000000000 ) ) ;
#357 = EDGE_CURVE ( 'NONE', #20895, #2845, #5405, .T. ) ;
#358 = B_SPLINE_SURFACE_WITH_KNOTS ( 'NONE', 5, 5, ( 
 ( #10209, #18565, #20758, #23504, #23087, #27741, #25691, #27609, #3542 ),
 ( #25277, #12127, #816, #21309, #7649, #19123, #16212, #964, #25125 ),
 ( #5159, #25412, #3402, #14040, #9658, #22946, #14328, #16367, #23222 ),
 ( #11846, #27457, #5305, #3131, #20898, #16516, #5443, #3270, #21043 ),
 ( #1100, #7777, #16650, #25544, #14467, #23361, #23634, #1928, #28278 ),
 ( #19396, #15144, #19819, #4092, #28424, #23917, #3954, #12678, #10767 ) ),
 .UNSPECIFIED., .F., .F., .F.,
 ( 6, 6 ),
 ( 6, 3, 6 ),
 ( 10.27983419480000116, 28.98451109560000205 ),
 ( 0.000000000000000000, 0.2500000000000000000, 0.5000000000000000000 ),
 .UNSPECIFIED. ) ;
#359 = LINE ( 'NONE', #9205, #7030 ) ;
#360 = ORIENTED_EDGE ( 'NONE', *, *, #15898, .T. ) ;
#361 = DIRECTION ( 'NONE',  ( 0.000000000000000000, -1.000000000000000000, 0.000000000000000000 ) ) ;
#362 = CARTESIAN_POINT ( 'NONE',  ( -12.45203970512436165, -101.4728631013286559, -10.26186846076686443 ) ) ;
#363 = CARTESIAN_POINT ( 'NONE',  ( 8.154561305720001485, -36.99980119890000196, -21.51307946880000088 ) ) ;
#364 = EDGE_CURVE ( 'NONE', #27046, #11872, #7856, .T. ) ;
#365 = CARTESIAN_POINT ( 'NONE',  ( 8.054097215812880961, -19.46843057288947421, -20.48836643782571443 ) ) ;
#366 = ORIENTED_EDGE ( 'NONE', *, *, #9045, .T. ) ;
#367 = AXIS2_PLACEMENT_3D ( 'NONE', #6686, #4637, #15550 ) ;
#368 = ADVANCED_FACE ( 'NONE', ( #27069 ), #19745, .T. ) ;
#369 = CIRCLE ( 'NONE', #15692, 60.85000000000000142 ) ;
#370 = DIRECTION ( 'NONE',  ( 0.000000000000000000, 1.000000000000000000, 0.000000000000000000 ) ) ;
#371 = CARTESIAN_POINT ( 'NONE',  ( -36.70028666173043774, -63.05366661935808992, 0.03681143521525633011 ) ) ;
#372 = DIRECTION ( 'NONE',  ( 0.000000000000000000, 1.000000000000000000, 0.000000000000000000 ) ) ;
#373 = CYLINDRICAL_SURFACE ( 'NONE', #27643, 15.99999999999999822 ) ;
#374 = CARTESIAN_POINT ( 'NONE',  ( -14.95854026159999961, -100.9763033870000015, 4.709388778109999230 ) ) ;
#375 = CARTESIAN_POINT ( 'NONE',  ( -17.31644382271060323, -99.07183861590023355, -8.238310338614811101 ) ) ;
#376 = CARTESIAN_POINT ( 'NONE',  ( -38.31826369283189848, -63.05366661936042050, -2.839229858537526852 ) ) ;
#377 = CONICAL_SURFACE ( 'NONE', #5926, 2.000000000000000888, 1.308996938999999804 ) ;
#378 = CARTESIAN_POINT ( 'NONE',  ( 26.29305724443631220, -63.71690337527751069, 1.488180441977877466 ) ) ;
#379 = CARTESIAN_POINT ( 'NONE',  ( 0.000000000000000000, -101.6484611540000031, 0.000000000000000000 ) ) ;
#380 = CARTESIAN_POINT ( 'NONE',  ( 24.72812962333588160, -93.39299082536693675, -12.36525841036616313 ) ) ;
#381 = CARTESIAN_POINT ( 'NONE',  ( -10.61287167059999881, -19.46510050329999686, 19.30934957549999709 ) ) ;
#382 = ORIENTED_EDGE ( 'NONE', *, *, #3847, .F. ) ;
#383 = CARTESIAN_POINT ( 'NONE',  ( 36.31166979920000415, -74.62997809459999132, -14.90098611910000059 ) ) ;
#384 = CARTESIAN_POINT ( 'NONE',  ( 3.883346862689999845, -2.000000000000000000, 7.108418751309999450 ) ) ;
#385 = AXIS2_PLACEMENT_3D ( 'NONE', #10663, #12718, #21630 ) ;
#386 = CARTESIAN_POINT ( 'NONE',  ( 23.63616061750000341, -94.63960162979999780, -2.179844042860000108 ) ) ;
#387 = CARTESIAN_POINT ( 'NONE',  ( -12.68423313600000135, -57.45864720369999645, 20.28110700490000085 ) ) ;
#388 = CARTESIAN_POINT ( 'NONE',  ( -1.314504061159999897E-13, -19.50000000000000000, -1.119104808819999722E-13 ) ) ;
#389 = CARTESIAN_POINT ( 'NONE',  ( 29.11677867130000052, -92.50000000000000000, 6.880015861159999524 ) ) ;
#390 = CARTESIAN_POINT ( 'NONE',  ( 18.71434861636577907, -18.49999996077436037, 10.15134080778569370 ) ) ;
#391 = ADVANCED_FACE ( 'NONE', ( #7256 ), #13212, .F. ) ;
#392 = B_SPLINE_CURVE_WITH_KNOTS ( 'NONE', 5,
 ( #381, #18132, #9225, #11262, #10956, #27029 ),
 .UNSPECIFIED., .F., .F.,
 ( 6, 6 ),
 ( 0.000000000000000000, 1.000000000000000000 ),
 .UNSPECIFIED. ) ;
#393 = CARTESIAN_POINT ( 'NONE',  ( 16.66712582699999956, -100.0994409990000094, 4.341523580040000496 ) ) ;
#394 = ORIENTED_EDGE ( 'NONE', *, *, #12962, .T. ) ;
#395 = CARTESIAN_POINT ( 'NONE',  ( -7.253647055860000137, -74.31845592130000000, -40.32201634399999790 ) ) ;
#396 = CARTESIAN_POINT ( 'NONE',  ( 30.63887047069549752, -74.17816095543288668, -24.34389095944435155 ) ) ;
#397 = EDGE_CURVE ( 'NONE', #15581, #14037, #15975, .T. ) ;
#398 = AXIS2_PLACEMENT_3D ( 'NONE', #25664, #5557, #14574 ) ;
#399 = CARTESIAN_POINT ( 'NONE',  ( -20.09682587570000223, -97.23151480800000002, -7.274462301079999804 ) ) ;
#400 = VERTEX_POINT ( 'NONE', #13649 ) ;
#401 = CARTESIAN_POINT ( 'NONE',  ( -30.44002477821454633, -92.69183043801065480, 1.913949942781201674 ) ) ;
#402 = DIRECTION ( 'NONE',  ( 0.6184463001828860440, 0.000000000000000000, 0.7858270635388550085 ) ) ;
#403 = DIRECTION ( 'NONE',  ( 0.4794255386042042266, 0.000000000000000000, 0.8775825618903720926 ) ) ;
#404 = DIRECTION ( 'NONE',  ( 0.000000000000000000, 0.000000000000000000, -1.000000000000000000 ) ) ;
#405 = CARTESIAN_POINT ( 'NONE',  ( 7.670973119660000172, -34.59820496239999699, -21.21808926809999818 ) ) ;
#406 = CARTESIAN_POINT ( 'NONE',  ( 22.78264864029999970, -94.59276292120000562, -6.873201003520000185 ) ) ;
#407 = TOROIDAL_SURFACE ( 'NONE', #6924, 18.14285714289999873, 0.5000000000000000000 ) ;
#408 = DIRECTION ( 'NONE',  ( 0.000000000000000000, 1.000000000000000000, 0.000000000000000000 ) ) ;
#409 = CARTESIAN_POINT ( 'NONE',  ( -1.598721155459999804E-14, -84.50000000000000000, 7.105427357599999217E-15 ) ) ;
#410 = CARTESIAN_POINT ( 'NONE',  ( 13.82833792859999811, -99.73367660430000115, -10.41122475269999903 ) ) ;
#411 = ORIENTED_EDGE ( 'NONE', *, *, #8688, .T. ) ;
#412 = CIRCLE ( 'NONE', #28280, 57.75000000000000000 ) ;
#413 = CARTESIAN_POINT ( 'NONE',  ( -12.08584015490000141, -69.49854784190000601, -25.11440668759999895 ) ) ;
#414 = CARTESIAN_POINT ( 'NONE',  ( -9.356041104380000917, -74.50000000000000000, -37.60355029590000697 ) ) ;
#415 = CARTESIAN_POINT ( 'NONE',  ( -13.27698888679999989, -99.83167681540000160, -11.13684395419999973 ) ) ;
#416 = CARTESIAN_POINT ( 'NONE',  ( -12.76745321220000129, -101.1364147039999892, -8.514038431850000421 ) ) ;
#417 = CARTESIAN_POINT ( 'NONE',  ( 16.58537890990000108, -94.98812477769999418, 16.93952572510000110 ) ) ;
#418 = VERTEX_POINT ( 'NONE', #2300 ) ;
#419 = EDGE_CURVE ( 'NONE', #9997, #22379, #25806, .T. ) ;
#420 = CARTESIAN_POINT ( 'NONE',  ( 0.000000000000000000, -90.50000000000000000, 0.000000000000000000 ) ) ;
#421 =( GEOMETRIC_REPRESENTATION_CONTEXT ( 3 ) GLOBAL_UNCERTAINTY_ASSIGNED_CONTEXT ( ( #7445 ) ) GLOBAL_UNIT_ASSIGNED_CONTEXT ( ( #6851, #22443, #317 ) ) REPRESENTATION_CONTEXT ( 'NONE', 'WORKASPACE' ) );
#422 = ORIENTED_EDGE ( 'NONE', *, *, #27436, .F. ) ;
#423 = B_SPLINE_CURVE_WITH_KNOTS ( 'NONE', 5,
 ( #28794, #10856, #8982, #22117, #26629, #17888, #2016, #26198, #19767 ),
 .UNSPECIFIED., .F., .F.,
 ( 6, 3, 6 ),
 ( 0.000000000000000000, 0.2815520576815128129, 1.000000000000000000 ),
 .UNSPECIFIED. ) ;
#424 = CARTESIAN_POINT ( 'NONE',  ( -4.500000000000000000, -11.00000000000000000, 31.00000000000000000 ) ) ;
#425 = B_SPLINE_CURVE_WITH_KNOTS ( 'NONE', 3,
 ( #6749, #17383, #15612, #10933, #24370, #2227, #8482, #26130 ),
 .UNSPECIFIED., .F., .F.,
 ( 4, 2, 2, 4 ),
 ( 0.000000000000000000, 0.5000000000000000000, 0.7500000000000000000, 1.000000000000000000 ),
 .UNSPECIFIED. ) ;
#426 = CARTESIAN_POINT ( 'NONE',  ( -10.50000000000000000, -89.00000000000000000, 6.411537967209999764E-15 ) ) ;
#427 = CARTESIAN_POINT ( 'NONE',  ( 10.51978096080000213, -92.52763213160000078, 27.11043680749999751 ) ) ;
#428 = ORIENTED_EDGE ( 'NONE', *, *, #14886, .F. ) ;
#429 = EDGE_CURVE ( 'NONE', #15620, #8975, #245, .T. ) ;
#430 = CIRCLE ( 'NONE', #7407, 0.4999999999999993339 ) ;
#431 = ORIENTED_EDGE ( 'NONE', *, *, #22851, .T. ) ;
#432 = DIRECTION ( 'NONE',  ( -1.000000000000000000, 0.000000000000000000, -4.565061778886334044E-16 ) ) ;
#433 = DIRECTION ( 'NONE',  ( 0.4151946956541399669, 0.5000000000001689759, 0.7600087925152558821 ) ) ;
#434 = CARTESIAN_POINT ( 'NONE',  ( 47.03393487260000683, -74.30497055530000239, -1.819362492409999810 ) ) ;
#435 = ORIENTED_EDGE ( 'NONE', *, *, #15676, .F. ) ;
#436 = DIRECTION ( 'NONE',  ( -1.224606353819999829E-16, 0.000000000000000000, 1.000000000000000000 ) ) ;
#437 = CARTESIAN_POINT ( 'NONE',  ( -11.33957729739370635, -60.31986010322346203, 20.76858926670032446 ) ) ;
#438 = DIRECTION ( 'NONE',  ( 1.000000000000000000, 0.000000000000000000, 0.000000000000000000 ) ) ;
#439 = CARTESIAN_POINT ( 'NONE',  ( -14.10155798110000092, -93.81709628049999594, -21.57370430179999943 ) ) ;
#440 = CARTESIAN_POINT ( 'NONE',  ( -24.00582547640926379, -94.71481465629901209, -4.132763972591003032 ) ) ;
#441 = ORIENTED_EDGE ( 'NONE', *, *, #13396, .T. ) ;
#442 = CARTESIAN_POINT ( 'NONE',  ( 36.44627168800000305, -74.06782051840001202, -14.22901210950000106 ) ) ;
#443 = CARTESIAN_POINT ( 'NONE',  ( -17.09009608839999927, -99.55609322370000314, 3.193624944930000265 ) ) ;
#444 = CARTESIAN_POINT ( 'NONE',  ( -39.96417052329999819, -74.08839659379999887, 7.268571389559999929 ) ) ;
#445 = CARTESIAN_POINT ( 'NONE',  ( -21.96029098729999873, -74.01681409379999366, -32.14278154310000701 ) ) ;
#446 = ORIENTED_EDGE ( 'NONE', *, *, #18563, .T. ) ;
#448 = TOROIDAL_SURFACE ( 'NONE', #14380, 3.500000000000000000, 0.5000000000000000000 ) ;
#447 = B_SPLINE_CURVE_WITH_KNOTS ( 'NONE', 3,
 ( #7135, #24608, #16144, #11221, #2517, #21773, #21492, #4538, #15745, #9188 ),
 .UNSPECIFIED., .F., .F.,
 ( 4, 2, 2, 2, 4 ),
 ( 0.000000000000000000, 0.2500000000000000000, 0.5000000000000000000, 0.7500000000000000000, 1.000000000000000000 ),
 .UNSPECIFIED. ) ;
#449 = DIRECTION ( 'NONE',  ( 0.000000000000000000, 1.000000000000000000, 0.000000000000000000 ) ) ;
#450 = DIRECTION ( 'NONE',  ( 0.000000000000000000, -1.000000000000000000, 0.000000000000000000 ) ) ;
#451 = CARTESIAN_POINT ( 'NONE',  ( -18.42673315119999700, -19.46723765599999822, 12.71460005940000038 ) ) ;
#452 = VERTEX_POINT ( 'NONE', #2600 ) ;
#453 = CIRCLE ( 'NONE', #16705, 25.14975229270000057 ) ;
#454 = CONICAL_SURFACE ( 'NONE', #1820, 55.67692378859999280, 1.047197551199999799 ) ;
#455 = DIRECTION ( 'NONE',  ( 0.9952295494196655712, 0.000000000000000000, -0.09756097560976655092 ) ) ;
#456 = EDGE_CURVE ( 'NONE', #25924, #731, #15538, .T. ) ;
#457 = AXIS2_PLACEMENT_3D ( 'NONE', #1882, #15240, #28107 ) ;
#458 = CARTESIAN_POINT ( 'NONE',  ( 23.02872706139999792, -64.78279487710000240, 10.89319034239999873 ) ) ;
#459 = CARTESIAN_POINT ( 'NONE',  ( 27.68682485439999752, -17.30000000000000071, 50.68039294919999804 ) ) ;
#460 = CARTESIAN_POINT ( 'NONE',  ( 15.94843830448696487, -101.0147714271772088, 4.203990814596493486 ) ) ;
#461 = CYLINDRICAL_SURFACE ( 'NONE', #14611, 7.250000000000004441 ) ;
#462 = EDGE_LOOP ( 'NONE', ( #7534, #13266, #11753, #16100 ) ) ;
#463 = DIRECTION ( 'NONE',  ( 0.000000000000000000, 1.000000000000000000, 0.000000000000000000 ) ) ;
#464 = CARTESIAN_POINT ( 'NONE',  ( -14.29547445250000060, -74.00000000000000000, 45.69901703040000029 ) ) ;
#465 = B_SPLINE_CURVE_WITH_KNOTS ( 'NONE', 5,
 ( #5943, #23459, #23728, #10162, #18944, #17165, #14693, #26054, #14961, #21544, #25785, #21403 ),
 .UNSPECIFIED., .F., .F.,
 ( 6, 3, 3, 6 ),
 ( 0.000000000000000000, 0.4964111757582199136, 0.7833083924326244007, 1.000000000000000000 ),
 .UNSPECIFIED. ) ;
#466 = CARTESIAN_POINT ( 'NONE',  ( -11.32870268019999926, -60.33034294469999992, -22.21640803110000206 ) ) ;
#467 = ADVANCED_FACE ( 'NONE', ( #20064 ), #15828, .T. ) ;
#468 = CARTESIAN_POINT ( 'NONE',  ( 25.82404717150000195, -69.73911356650000926, -8.782782835009999900 ) ) ;
#469 = DIRECTION ( 'NONE',  ( 1.000000000000000000, 0.000000000000000000, 0.000000000000000000 ) ) ;
#470 = ORIENTED_EDGE ( 'NONE', *, *, #14294, .F. ) ;
#471 = CARTESIAN_POINT ( 'NONE',  ( 7.815970093360001426E-15, -84.50000000000000000, -40.00000000000000000 ) ) ;
#473 = ORIENTED_EDGE ( 'NONE', *, *, #11539, .F. ) ;
#472 = TOROIDAL_SURFACE ( 'NONE', #16728, 1.500000000000000000, 0.5000000000000000000 ) ;
#474 = DIRECTION ( 'NONE',  ( 0.000000000000000000, 1.000000000000000000, 0.000000000000000000 ) ) ;
#475 = CARTESIAN_POINT ( 'NONE',  ( 9.119802927630001221, -98.28914429610000525, 16.69368728350000097 ) ) ;
#476 = EDGE_LOOP ( 'NONE', ( #14422, #15237, #5808, #25954 ) ) ;
#477 = CYLINDRICAL_SURFACE ( 'NONE', #16417, 5.999999999999999112 ) ;
#478 = CIRCLE ( 'NONE', #7895, 3.000000000000000000 ) ;
#479 = CIRCLE ( 'NONE', #4152, 28.68388914670000034 ) ;
#480 = PLANE ( 'NONE',  #18583 ) ;
#481 = DIRECTION ( 'NONE',  ( 0.000000000000000000, 1.000000000000000000, 0.000000000000000000 ) ) ;
#482 = CARTESIAN_POINT ( 'NONE',  ( -10.10487300439999991, -18.62107971969999909, -21.27518202489999766 ) ) ;
#483 = CARTESIAN_POINT ( 'NONE',  ( 21.51792335492191199, -37.40300027226001589, -7.702379948524843201 ) ) ;
#484 = ORIENTED_EDGE ( 'NONE', *, *, #2417, .F. ) ;
#485 = CARTESIAN_POINT ( 'NONE',  ( 11.45574570990000041, -93.13207089280000162, -23.61394595179999811 ) ) ;
#486 = CARTESIAN_POINT ( 'NONE',  ( -20.39638010391581702, -61.43221488831640897, 12.45288284519579314 ) ) ;
#487 = CARTESIAN_POINT ( 'NONE',  ( -13.33479272893357859, -92.93978723899297734, 27.43052168310984840 ) ) ;
#488 = ORIENTED_EDGE ( 'NONE', *, *, #1371, .F. ) ;
#489 = LINE ( 'NONE', #22764, #1160 ) ;
#490 = DIRECTION ( 'NONE',  ( 0.4794255386042036715, 0.000000000000000000, 0.8775825618903724257 ) ) ;
#491 = CARTESIAN_POINT ( 'NONE',  ( 14.34373124439999891, -102.5000000000000000, 26.25602392650000283 ) ) ;
#492 = ORIENTED_EDGE ( 'NONE', *, *, #28617, .F. ) ;
#493 = CARTESIAN_POINT ( 'NONE',  ( -18.48642635659999911, -96.07607726710000406, 13.72266607319999920 ) ) ;
#494 = CARTESIAN_POINT ( 'NONE',  ( 0.6457915530089999301, -99.58396362730000817, -17.35065848859999704 ) ) ;
#495 = CARTESIAN_POINT ( 'NONE',  ( -20.45998242170000125, -52.56313962710000709, 14.78974999389999923 ) ) ;
#496 = CARTESIAN_POINT ( 'NONE',  ( -19.95527577780000072, -57.47855601759999900, 12.14622656770000120 ) ) ;
#497 = PRODUCT_RELATED_PRODUCT_CATEGORY ( 'part', '', ( #13159 ) ) ;
#498 = CARTESIAN_POINT ( 'NONE',  ( 22.40625751809999855, -60.56287431679999855, -8.064917839230000496 ) ) ;
#499 = EDGE_CURVE ( 'NONE', #18811, #12707, #22077, .T. ) ;
#500 = CARTESIAN_POINT ( 'NONE',  ( 27.49606017789999868, -67.46051290640001241, 1.934794646639999893 ) ) ;
#501 = CARTESIAN_POINT ( 'NONE',  ( -10.27945668490000131, -18.50000000000000000, 18.70272521329999904 ) ) ;
#502 = EDGE_CURVE ( 'NONE', #19526, #5924, #14185, .T. ) ;
#503 = EDGE_CURVE ( 'NONE', #1478, #12804, #17430, .T. ) ;
#504 = EDGE_LOOP ( 'NONE', ( #699, #16423, #5514, #12046 ) ) ;
#505 = CARTESIAN_POINT ( 'NONE',  ( 10.20110288159999890, -74.50000000000000000, -41.00000000000000000 ) ) ;
#506 = CARTESIAN_POINT ( 'NONE',  ( -43.20000000000000284, -65.14977478849999670, 0.1732050807559999961 ) ) ;
#507 = B_SPLINE_CURVE_WITH_KNOTS ( 'NONE', 3,
 ( #4002, #15340, #26308, #12728 ),
 .UNSPECIFIED., .F., .F.,
 ( 4, 4 ),
 ( 0.000000000000000000, 1.000000000000000000 ),
 .UNSPECIFIED. ) ;
#508 = CARTESIAN_POINT ( 'NONE',  ( 10.14179094049999819, -99.62155479429999616, 14.52072615979999881 ) ) ;
#509 = EDGE_LOOP ( 'NONE', ( #14292, #25818, #23874, #1797 ) ) ;
#510 = CARTESIAN_POINT ( 'NONE',  ( 7.323170304809999642, -73.87254094300001839, 39.07240670449999698 ) ) ;
#511 = CARTESIAN_POINT ( 'NONE',  ( 26.37318048140000215, -93.00000450890000536, 13.16123783449999962 ) ) ;
#512 = DIRECTION ( 'NONE',  ( 0.000000000000000000, 1.000000000000000000, 0.000000000000000000 ) ) ;
#513 = FACE_OUTER_BOUND ( 'NONE', #18198, .T. ) ;
#514 = CARTESIAN_POINT ( 'NONE',  ( -6.885095864830000245, -101.1417990620000040, 14.17428525849999943 ) ) ;
#515 = CARTESIAN_POINT ( 'NONE',  ( 26.80884837331130655, -72.62863614316471228, -10.52387429041271538 ) ) ;
#516 = CARTESIAN_POINT ( 'NONE',  ( -12.61948338259999858, -101.6484611540000031, -9.836088610590000059 ) ) ;
#517 = CARTESIAN_POINT ( 'NONE',  ( 8.994939661169999212, -36.15004583290000539, -20.77616074780000233 ) ) ;
#518 = CARTESIAN_POINT ( 'NONE',  ( 8.620126422187169624, -19.47938362974832316, -19.97534244429069616 ) ) ;
#519 = VERTEX_POINT ( 'NONE', #424 ) ;
#520 = CIRCLE ( 'NONE', #16773, 5.000000000000000888 ) ;
#521 = CARTESIAN_POINT ( 'NONE',  ( 7.321257786130000333, -99.28585527969998736, 16.15667156069999777 ) ) ;
#522 = CARTESIAN_POINT ( 'NONE',  ( 36.28164458690000060, -74.50000000000000000, -14.97346873880000118 ) ) ;
#523 = CARTESIAN_POINT ( 'NONE',  ( -3.773308002759999891, -96.65227117080000596, -20.92579437230000039 ) ) ;
#524 = CARTESIAN_POINT ( 'NONE',  ( -2.568686407175419184, -19.48618186047746548, -23.50321383691693100 ) ) ;
#525 = CYLINDRICAL_SURFACE ( 'NONE', #18143, 7.249999999999999112 ) ;
#526 = CARTESIAN_POINT ( 'NONE',  ( 5.873292863139999653, -11.55246854740000018, 10.75099047199999980 ) ) ;
#527 = DIRECTION ( 'NONE',  ( 1.000000000000000000, 0.000000000000000000, 0.000000000000000000 ) ) ;
#528 = CARTESIAN_POINT ( 'NONE',  ( -39.10791602276640333, -73.54003775238672347, 7.198125313980217932 ) ) ;
#529 = DIRECTION ( 'NONE',  ( -0.2414462220490760924, 0.000000000000000000, -0.9704142011833030157 ) ) ;
#530 = FACE_OUTER_BOUND ( 'NONE', #1949, .T. ) ;
#531 = DIRECTION ( 'NONE',  ( 0.000000000000000000, 1.000000000000000000, 0.000000000000000000 ) ) ;
#532 = ORIENTED_EDGE ( 'NONE', *, *, #4377, .T. ) ;
#533 = ADVANCED_FACE ( 'NONE', ( #11147 ), #17891, .T. ) ;
#534 = CARTESIAN_POINT ( 'NONE',  ( 36.25731322790000632, -74.69416361989999587, -15.03231676859999943 ) ) ;
#535 = CARTESIAN_POINT ( 'NONE',  ( -22.29222582179728107, -79.74578553650356127, -32.80938733156981613 ) ) ;
#536 = CONICAL_SURFACE ( 'NONE', #26096, 7.000000000000005329, 0.7853981633970000820 ) ;
#537 = AXIS2_PLACEMENT_3D ( 'NONE', #16966, #27223, #1016 ) ;
#538 = EDGE_CURVE ( 'NONE', #11457, #18344, #12745, .T. ) ;
#539 = CIRCLE ( 'NONE', #15843, 30.50000000000000000 ) ;
#540 = CARTESIAN_POINT ( 'NONE',  ( -11.41594931139999858, -19.46510050329999686, -18.84569254350000023 ) ) ;
#541 = CARTESIAN_POINT ( 'NONE',  ( 19.99082350619999815, -35.29518274429999991, -8.963945870050000764 ) ) ;
#542 = CARTESIAN_POINT ( 'NONE',  ( -19.01557598121447157, -92.50000000001456613, 22.91712378798360916 ) ) ;
#543 = CARTESIAN_POINT ( 'NONE',  ( 28.83687378200000140, -92.50000647099999185, 7.262115126140000321 ) ) ;
#544 = DIRECTION ( 'NONE',  ( 0.000000000000000000, -1.000000000000000000, 0.000000000000000000 ) ) ;
#545 = CARTESIAN_POINT ( 'NONE',  ( -19.98788946392987853, -95.81531090358907932, 9.701109111489476078 ) ) ;
#546 = CARTESIAN_POINT ( 'NONE',  ( 27.68682485439999752, -14.30000000000000071, 50.68039294919999804 ) ) ;
#547 = ORIENTED_EDGE ( 'NONE', *, *, #12350, .T. ) ;
#548 = CARTESIAN_POINT ( 'NONE',  ( 21.56931449510000220, -36.56979901409999911, -6.850353628320000610 ) ) ;
#549 = CARTESIAN_POINT ( 'NONE',  ( -24.15517241699999929, -94.98812769030000425, -4.102690932189999806 ) ) ;
#550 = ORIENTED_EDGE ( 'NONE', *, *, #21053, .T. ) ;
#551 = CARTESIAN_POINT ( 'NONE',  ( 8.639505966715979923, -92.69183043846588532, 29.25093587448420962 ) ) ;
#552 = CARTESIAN_POINT ( 'NONE',  ( 0.3872056760440000245, -99.92967571559999840, -17.35614698070000017 ) ) ;
#553 = LINE ( 'NONE', #19920, #16709 ) ;
#554 = DIRECTION ( 'NONE',  ( 1.000000000000000000, 0.000000000000000000, 0.000000000000000000 ) ) ;
#555 = CARTESIAN_POINT ( 'NONE',  ( -40.00000000000000000, -65.00000000000000000, 3.175426480540000096 ) ) ;
#556 = AXIS2_PLACEMENT_3D ( 'NONE', #15444, #1512, #21732 ) ;
#557 = DIRECTION ( 'NONE',  ( 0.9982579106777251798, 0.000000000000000000, -0.05900121837168281064 ) ) ;
#558 = CIRCLE ( 'NONE', #25661, 18.64285714289999873 ) ;
#559 = VECTOR ( 'NONE', #7059, 1000.000000000000000 ) ;
#560 = CARTESIAN_POINT ( 'NONE',  ( -13.82310862920000005, -74.00000000000000000, 36.20061004779999791 ) ) ;
#561 = CARTESIAN_POINT ( 'NONE',  ( -21.72229115340000050, -67.06690763590000870, 14.40139912269999911 ) ) ;
#562 = CARTESIAN_POINT ( 'NONE',  ( 14.21256893470000193, -98.58303758080000989, -12.13706782569999909 ) ) ;
#563 = EDGE_LOOP ( 'NONE', ( #25536, #17511, #4054, #11653 ) ) ;
#565 = EDGE_CURVE ( 'NONE', #21465, #19989, #2562, .T. ) ;
#564 = CARTESIAN_POINT ( 'NONE',  ( -12.47289874710000035, -69.87861895790000233, -24.46965691790000363 ) ) ;
#566 = DIRECTION ( 'NONE',  ( 0.000000000000000000, 1.000000000000000000, 0.000000000000000000 ) ) ;
#567 = CARTESIAN_POINT ( 'NONE',  ( 7.891778559019607009, -101.5538022607323683, 14.00007649551812072 ) ) ;
#568 = DIRECTION ( 'NONE',  ( 0.000000000000000000, -1.000000000000000000, 0.000000000000000000 ) ) ;
#569 = CARTESIAN_POINT ( 'NONE',  ( 7.135467692469593892, -73.63089972761061119, -38.71641001238787538 ) ) ;
#570 = ORIENTED_EDGE ( 'NONE', *, *, #2545, .F. ) ;
#571 = ADVANCED_FACE ( 'NONE', ( #26925 ), #15677, .T. ) ;
#572 = CARTESIAN_POINT ( 'NONE',  ( 26.38387423984804769, -92.80045754842753070, -15.30171679607595259 ) ) ;
#573 = ORIENTED_EDGE ( 'NONE', *, *, #1821, .F. ) ;
#574 = EDGE_CURVE ( 'NONE', #4330, #15463, #9981, .T. ) ;
#575 = DIRECTION ( 'NONE',  ( 0.4794255386042000078, 0.000000000000000000, 0.8775825618903743131 ) ) ;
#576 = CARTESIAN_POINT ( 'NONE',  ( -4.045235864600000397, -98.43722212099999069, 19.19069134749999961 ) ) ;
#577 = VECTOR ( 'NONE', #18094, 1000.000000000000000 ) ;
#578 = CARTESIAN_POINT ( 'NONE',  ( 8.074115162410000934, -92.66424957140000629, 26.74225754210000261 ) ) ;
#579 = VECTOR ( 'NONE', #5626, 999.9999999999998863 ) ;
#580 = ORIENTED_EDGE ( 'NONE', *, *, #6138, .F. ) ;
#581 = CARTESIAN_POINT ( 'NONE',  ( 0.000000000000000000, -37.08699221940000257, 0.000000000000000000 ) ) ;
#582 = CARTESIAN_POINT ( 'NONE',  ( -16.86265888959999870, -79.50000000000000000, 45.21850545039999503 ) ) ;
#583 = CARTESIAN_POINT ( 'NONE',  ( 10.08829703670000022, -36.00000000000000000, -20.49602678049999938 ) ) ;
#584 = VERTEX_POINT ( 'NONE', #13793 ) ;
#585 = CARTESIAN_POINT ( 'NONE',  ( 7.246063797170706700, -73.82871504787716788, -39.75929607700521018 ) ) ;
#586 = CARTESIAN_POINT ( 'NONE',  ( -11.50280172684225732, -61.70151683873936577, 21.01880821135103972 ) ) ;
#587 = ORIENTED_EDGE ( 'NONE', *, *, #16283, .F. ) ;
#588 = CARTESIAN_POINT ( 'NONE',  ( 22.44118743278407280, -65.00127796776330058, 11.39886732859506502 ) ) ;
#589 = EDGE_CURVE ( 'NONE', #21458, #13839, #9040, .T. ) ;
#590 = CARTESIAN_POINT ( 'NONE',  ( 7.367077158260816994, -101.1416252679887577, 13.68480675837215799 ) ) ;
#591 = CARTESIAN_POINT ( 'NONE',  ( -2.675358685650000012, -67.79480919600000277, -26.71434926430000090 ) ) ;
#592 = PLANE ( 'NONE',  #25559 ) ;
#593 = CARTESIAN_POINT ( 'NONE',  ( -15.48552837409999938, -71.82739780379999672, 23.60563397449999812 ) ) ;
#594 = ORIENTED_EDGE ( 'NONE', *, *, #7560, .T. ) ;
#595 = DIRECTION ( 'NONE',  ( 1.000000000000000000, 0.000000000000000000, 0.000000000000000000 ) ) ;
#596 = CARTESIAN_POINT ( 'NONE',  ( -16.91403943069999727, -99.72583475830001021, 3.025870399720000048 ) ) ;
#597 = CARTESIAN_POINT ( 'NONE',  ( 25.46032906830000186, -64.78279197330000727, 0.8694561931790000253 ) ) ;
#598 = CARTESIAN_POINT ( 'NONE',  ( -21.94602169939999925, -74.00000000000000000, -32.01791432939999993 ) ) ;
#599 = ORIENTED_EDGE ( 'NONE', *, *, #25882, .T. ) ;
#600 = CARTESIAN_POINT ( 'NONE',  ( -19.61617179850000170, -45.99935878759999497, 11.93235644279999974 ) ) ;
#601 = VECTOR ( 'NONE', #24406, 1000.000000000000000 ) ;
#602 = CARTESIAN_POINT ( 'NONE',  ( 0.7331063123750001242, -99.53431386179998697, -17.39857302659999760 ) ) ;
#603 = CARTESIAN_POINT ( 'NONE',  ( -18.66344010299999923, -18.85523519099999845, 11.44727505870000073 ) ) ;
#604 = ORIENTED_EDGE ( 'NONE', *, *, #24072, .T. ) ;
#605 = ADVANCED_FACE ( 'NONE', ( #18903 ), #27359, .T. ) ;
#607 = EDGE_CURVE ( 'NONE', #27919, #28507, #7827, .T. ) ;
#606 = CARTESIAN_POINT ( 'NONE',  ( -9.465083148179999739, -93.62676565499999981, -23.38439984080000045 ) ) ;
#608 = DIRECTION ( 'NONE',  ( 0.3388759126238506392, 0.000000000000000000, -0.9408310772095872521 ) ) ;
#609 = CARTESIAN_POINT ( 'NONE',  ( 8.964388214039999525, -35.14340553630000130, -19.96644199109999818 ) ) ;
#610 = CARTESIAN_POINT ( 'NONE',  ( 16.28778070538160350, -100.5550990449209223, 4.345266980774773913 ) ) ;
#611 = DIRECTION ( 'NONE',  ( 0.000000000000000000, 1.000000000000000000, 0.000000000000000000 ) ) ;
#612 = ORIENTED_EDGE ( 'NONE', *, *, #9543, .F. ) ;
#613 = CARTESIAN_POINT ( 'NONE',  ( 47.25000000000000000, -79.00000000000000000, -7.713829575100000215E-13 ) ) ;
#614 = CONTEXT_DEPENDENT_SHAPE_REPRESENTATION ( #13885, #24097 ) ;
#615 = CARTESIAN_POINT ( 'NONE',  ( -11.81677247600000058, -62.06858034060000762, -21.05646513629999816 ) ) ;
#616 = CARTESIAN_POINT ( 'NONE',  ( 25.13747520559999771, -67.81660459209999203, -9.975487151870000346 ) ) ;
#617 = CARTESIAN_POINT ( 'NONE',  ( 9.475766568499999210, -35.50000000000000000, -19.97576656850000276 ) ) ;
#618 = VERTEX_POINT ( 'NONE', #23274 ) ;
#619 = DIRECTION ( 'NONE',  ( 0.000000000000000000, 1.000000000000000000, 0.000000000000000000 ) ) ;
#620 = ORIENTED_EDGE ( 'NONE', *, *, #6006, .F. ) ;
#621 = CARTESIAN_POINT ( 'NONE',  ( 0.000000000000000000, -102.5000000000000000, 0.000000000000000000 ) ) ;
#622 = CARTESIAN_POINT ( 'NONE',  ( 9.335817441747641610, -98.58684426249028832, 16.46450815360437048 ) ) ;
#623 = VERTEX_POINT ( 'NONE', #3318 ) ;
#624 = AXIS2_PLACEMENT_3D ( 'NONE', #1463, #10304, #17029 ) ;
#625 = CARTESIAN_POINT ( 'NONE',  ( -2.579145438419999881, -53.53226321310000202, -25.13754169039999908 ) ) ;
#626 = EDGE_CURVE ( 'NONE', #27517, #13659, #27786, .T. ) ;
#627 = CARTESIAN_POINT ( 'NONE',  ( -22.27191869549999836, -94.59276292389999696, -8.381623179300000004 ) ) ;
#628 = CARTESIAN_POINT ( 'NONE',  ( -10.49491320851042708, -19.48298603870330581, -20.96686108838342832 ) ) ;
#629 = CARTESIAN_POINT ( 'NONE',  ( -18.14789115860000024, -98.53904439360000822, 4.701750000830000609 ) ) ;
#630 = CARTESIAN_POINT ( 'NONE',  ( -0.5455113252076949637, -98.53908159007990264, -18.73906669024530913 ) ) ;
#631 = CARTESIAN_POINT ( 'NONE',  ( 47.24130919904909121, -79.14360025649037311, -0.4895094584727857079 ) ) ;
#632 = EDGE_LOOP ( 'NONE', ( #19632, #17486, #11324, #22339 ) ) ;
#633 = CARTESIAN_POINT ( 'NONE',  ( 13.03263341399999931, -94.63960343439998724, -19.83860458410000049 ) ) ;
#634 = CARTESIAN_POINT ( 'NONE',  ( -20.38860325545200070, -61.39165777032547311, 12.44713039966608292 ) ) ;
#635 = DIRECTION ( 'NONE',  ( 0.000000000000000000, 1.000000000000000000, 0.000000000000000000 ) ) ;
#636 = ORIENTED_EDGE ( 'NONE', *, *, #17902, .T. ) ;
#637 = DIRECTION ( 'NONE',  ( -1.000000000000000000, 0.000000000000000000, 0.000000000000000000 ) ) ;
#638 = CYLINDRICAL_SURFACE ( 'NONE', #9269, 4.999999999999999112 ) ;
#639 = CARTESIAN_POINT ( 'NONE',  ( 7.235472567440000446, -61.68715554919999988, -22.75972229710000150 ) ) ;
#640 = VERTEX_POINT ( 'NONE', #18620 ) ;
#641 = CARTESIAN_POINT ( 'NONE',  ( -18.40263696530000104, -95.90090461900000207, 13.63749173159999906 ) ) ;
#642 = CARTESIAN_POINT ( 'NONE',  ( 0.7331063045040000503, -99.53431386179998697, -17.39857310140000024 ) ) ;
#643 = DIRECTION ( 'NONE',  ( 0.000000000000000000, 1.000000000000000000, 0.000000000000000000 ) ) ;
#644 = CARTESIAN_POINT ( 'NONE',  ( 22.30843460160000191, -36.00000000000000000, -11.28235740200000059 ) ) ;
#645 = CARTESIAN_POINT ( 'NONE',  ( 23.70193923009999892, -61.68490361759999985, -9.613352042829999888 ) ) ;
#646 = VECTOR ( 'NONE', #958, 1000.000000000000000 ) ;
#647 = CARTESIAN_POINT ( 'NONE',  ( 25.12978992150000224, -65.01950800350000748, 0.1513709550449999774 ) ) ;
#648 = DIRECTION ( 'NONE',  ( 1.000000000000000000, 0.000000000000000000, 0.000000000000000000 ) ) ;
#649 = ORIENTED_EDGE ( 'NONE', *, *, #27398, .T. ) ;
#650 = CARTESIAN_POINT ( 'NONE',  ( -19.68803156824991163, -18.87168151093004198, 14.53288012867929702 ) ) ;
#651 = VECTOR ( 'NONE', #20044, 1000.000000000000114 ) ;
#652 = CARTESIAN_POINT ( 'NONE',  ( 8.185345124539999517, -101.3150701389999995, 14.03998254610000096 ) ) ;
#653 = ORIENTED_EDGE ( 'NONE', *, *, #17240, .T. ) ;
#654 = CARTESIAN_POINT ( 'NONE',  ( 7.135467526410000261, -73.50000000000000000, 38.71641004229999794 ) ) ;
#655 = CARTESIAN_POINT ( 'NONE',  ( 7.383549334360000493, -18.50000000000000000, -19.69582310909999734 ) ) ;
#656 = CARTESIAN_POINT ( 'NONE',  ( 23.35112319427650007, -19.48210987405916583, 1.375628917947436136 ) ) ;
#657 = CARTESIAN_POINT ( 'NONE',  ( -7.569816714379999922, -100.7776802639999971, 13.87827956499999971 ) ) ;
#658 = CARTESIAN_POINT ( 'NONE',  ( -12.66558680574216922, -93.40492137171338527, -23.55307789253798845 ) ) ;
#659 = CARTESIAN_POINT ( 'NONE',  ( 9.018047497980001381, -36.17942459150000190, -20.85226661109999924 ) ) ;
#660 = AXIS2_PLACEMENT_3D ( 'NONE', #6377, #25920, #4047 ) ;
#661 = CARTESIAN_POINT ( 'NONE',  ( 7.318052426040000391, -101.1822553929999913, 13.41977313900000013 ) ) ;
#662 = ORIENTED_EDGE ( 'NONE', *, *, #22175, .F. ) ;
#663 = EDGE_CURVE ( 'NONE', #10505, #5317, #25363, .T. ) ;
#664 = CARTESIAN_POINT ( 'NONE',  ( -43.22799762839635918, -65.13413837705087417, 0.1570406424686417168 ) ) ;
#665 = CARTESIAN_POINT ( 'NONE',  ( -36.74605004467864688, -63.06523941402065958, -0.1332336900803410829 ) ) ;
#666 = CARTESIAN_POINT ( 'NONE',  ( 21.48302338326642413, -36.56890885472610364, -7.253824468342653375 ) ) ;
#667 = ORIENTED_EDGE ( 'NONE', *, *, #3117, .T. ) ;
#668 = DIRECTION ( 'NONE',  ( -0.7071067811865470176, 0.000000000000000000, 0.7071067811865480168 ) ) ;
#669 = EDGE_CURVE ( 'NONE', #15395, #12657, #1152, .T. ) ;
#670 = CARTESIAN_POINT ( 'NONE',  ( 11.85549584000000145, -101.3350617309999961, -10.77753387699999976 ) ) ;
#671 = CARTESIAN_POINT ( 'NONE',  ( -0.8441209747499999194, -45.99930305819999887, -22.94698520209999870 ) ) ;
#672 = CARTESIAN_POINT ( 'NONE',  ( 15.48878798707903925, -95.04305759974297985, 17.29288121155813585 ) ) ;
#673 = EDGE_CURVE ( 'NONE', #12096, #23467, #9990, .T. ) ;
#674 = DIRECTION ( 'NONE',  ( 0.000000000000000000, 1.000000000000000000, 0.000000000000000000 ) ) ;
#675 = AXIS2_PLACEMENT_3D ( 'NONE', #1404, #7809, #1680 ) ;
#676 = CARTESIAN_POINT ( 'NONE',  ( 41.00000000000000000, -74.50000000000000000, 10.20110288159999890 ) ) ;
#677 = CARTESIAN_POINT ( 'NONE',  ( 22.20693316850000087, -40.71455396009999816, -8.968806686309999776 ) ) ;
#678 = CARTESIAN_POINT ( 'NONE',  ( 19.97576656849999921, -72.00000000000000000, -19.97576656849999921 ) ) ;
#679 = CARTESIAN_POINT ( 'NONE',  ( -14.88706571849999882, -101.2269841009999993, 3.209819282999999857 ) ) ;
#680 = ORIENTED_EDGE ( 'NONE', *, *, #13024, .F. ) ;
#681 = CARTESIAN_POINT ( 'NONE',  ( 36.59408416780000550, -74.85684975549999365, -14.74361069959999959 ) ) ;
#682 = CARTESIAN_POINT ( 'NONE',  ( -32.66809844459999823, -74.41869006989999491, -22.00101410510000122 ) ) ;
#683 = CARTESIAN_POINT ( 'NONE',  ( -18.13877362739999910, -92.50000000000000000, -23.79298866759999598 ) ) ;
#684 = AXIS2_PLACEMENT_3D ( 'NONE', #27269, #20999, #20718 ) ;
#685 = CARTESIAN_POINT ( 'NONE',  ( 21.27776255609999723, -96.58372173029999885, 1.059637706860000028 ) ) ;
#686 = CARTESIAN_POINT ( 'NONE',  ( 9.004237477329999351, -35.65077419509999146, -19.54737253879999770 ) ) ;
#687 = CARTESIAN_POINT ( 'NONE',  ( 23.18812391385057126, -58.58546841852697895, 10.40058855015711892 ) ) ;
#688 = CARTESIAN_POINT ( 'NONE',  ( 20.11250903250000022, -36.00000000000000000, -9.561259576869998611 ) ) ;
#689 = CARTESIAN_POINT ( 'NONE',  ( 21.16767063019999995, -36.23936169889999803, -8.913590358700000493 ) ) ;
#690 = CARTESIAN_POINT ( 'NONE',  ( 0.4125572470530000091, -92.84292833370000153, -30.36594662649999776 ) ) ;
#691 = CIRCLE ( 'NONE', #4371, 24.76278252470000041 ) ;
#692 = CARTESIAN_POINT ( 'NONE',  ( 16.40194905730000130, -100.1981337080000003, 4.404945126920000398 ) ) ;
#693 = ORIENTED_EDGE ( 'NONE', *, *, #2892, .T. ) ;
#694 = CIRCLE ( 'NONE', #26077, 1.249999999999999112 ) ;
#695 = CARTESIAN_POINT ( 'NONE',  ( 8.185346967789998374, -101.3150701389999995, 14.03998109830000018 ) ) ;
#696 = CARTESIAN_POINT ( 'NONE',  ( -22.25469472199999998, -96.07623048470000526, -5.897558151980000218 ) ) ;
#697 = ORIENTED_EDGE ( 'NONE', *, *, #27258, .F. ) ;
#698 = CARTESIAN_POINT ( 'NONE',  ( -30.48402335599918800, -92.52498922770503498, 0.9899291096564720727 ) ) ;
#699 = ORIENTED_EDGE ( 'NONE', *, *, #16855, .F. ) ;
#700 = EDGE_CURVE ( 'NONE', #27146, #28156, #13733, .T. ) ;
#701 = DIRECTION ( 'NONE',  ( 0.000000000000000000, -1.000000000000000000, 0.000000000000000000 ) ) ;
#702 = DIRECTION ( 'NONE',  ( 0.000000000000000000, 0.000000000000000000, -1.000000000000000000 ) ) ;
#703 = DIRECTION ( 'NONE',  ( 0.000000000000000000, 1.000000000000000000, 0.000000000000000000 ) ) ;
#704 = TOROIDAL_SURFACE ( 'NONE', #18826, 25.11294200180000047, 0.5000000000000000000 ) ;
#705 = CARTESIAN_POINT ( 'NONE',  ( -7.250038883930940870, -73.95086734744796786, -39.95935625309049755 ) ) ;
#706 = ADVANCED_FACE ( 'NONE', ( #3044 ), #14624, .F. ) ;
#707 = CARTESIAN_POINT ( 'NONE',  ( -14.57729759870000130, -74.12911414260001663, 36.26887511289999821 ) ) ;
#708 = CARTESIAN_POINT ( 'NONE',  ( -21.87632299289999693, -67.55173099820000004, 16.08189821899999927 ) ) ;
#709 = CARTESIAN_POINT ( 'NONE',  ( 14.00782577689999897, -96.65227117100000953, -15.99711037630000021 ) ) ;
#710 = ORIENTED_EDGE ( 'NONE', *, *, #14232, .F. ) ;
#711 = CARTESIAN_POINT ( 'NONE',  ( -12.46915732870000149, -70.42119542689999889, -24.73933575500000259 ) ) ;
#712 = CARTESIAN_POINT ( 'NONE',  ( 8.142471319829999388, -22.47117226119999955, -20.59194991089999860 ) ) ;
#713 = DIRECTION ( 'NONE',  ( 0.9295286103719528903, 0.000000000000000000, 0.3687499999999813705 ) ) ;
#714 = CARTESIAN_POINT ( 'NONE',  ( 19.96073932771978221, -19.46608320370787482, 9.833604944531050052 ) ) ;
#715 = CARTESIAN_POINT ( 'NONE',  ( 11.77298154309999845, -101.2530993010000060, -9.604785791470000333 ) ) ;
#716 = ORIENTED_EDGE ( 'NONE', *, *, #14608, .F. ) ;
#717 = CIRCLE ( 'NONE', #12731, 2.000000035459998493 ) ;
#718 = ORIENTED_EDGE ( 'NONE', *, *, #26083, .T. ) ;
#719 = CARTESIAN_POINT ( 'NONE',  ( -2.487950882160000265, -57.83919435140000331, -24.63540447140000111 ) ) ;
#720 = LINE ( 'NONE', #20953, #7524 ) ;
#721 = LINE ( 'NONE', #9422, #6410 ) ;
#722 = CARTESIAN_POINT ( 'NONE',  ( 2.631283596650000334, -94.29487537309999823, 25.29847487550000196 ) ) ;
#723 = VERTEX_POINT ( 'NONE', #5055 ) ;
#724 = CARTESIAN_POINT ( 'NONE',  ( -11.18835776723661724, -94.77533639018899692, -20.78536094536529077 ) ) ;
#725 = CIRCLE ( 'NONE', #16980, 18.64285714289999518 ) ;
#726 = VERTEX_POINT ( 'NONE', #19037 ) ;
#727 = CARTESIAN_POINT ( 'NONE',  ( -26.32546053305905076, -93.86130746203110675, -1.655768764585977548 ) ) ;
#728 = CARTESIAN_POINT ( 'NONE',  ( 21.09474350280000010, -36.06031159909999673, -9.858094216790000530 ) ) ;
#729 = ADVANCED_FACE ( 'NONE', ( #27924 ), #23339, .F. ) ;
#730 = CARTESIAN_POINT ( 'NONE',  ( 47.14031554959999681, -74.51859318479999672, -1.361887490440000015 ) ) ;
#731 = VERTEX_POINT ( 'NONE', #1559 ) ;
#732 = CARTESIAN_POINT ( 'NONE',  ( 7.250349464191871540, -73.96150430845511892, -39.97648509748324130 ) ) ;
#733 = CARTESIAN_POINT ( 'NONE',  ( -11.45517213598250095, -61.33682282352064874, 20.94728758455344675 ) ) ;
#734 = EDGE_CURVE ( 'NONE', #9200, #23505, #24513, .T. ) ;
#735 = CARTESIAN_POINT ( 'NONE',  ( 24.22382764319999993, -64.24504439390000243, 10.76339940740000145 ) ) ;
#736 = CIRCLE ( 'NONE', #10888, 0.3500000000000003664 ) ;
#737 = CARTESIAN_POINT ( 'NONE',  ( -2.901733356760000326, -65.28594186040000125, -26.69036142120000221 ) ) ;
#738 = ADVANCED_FACE ( 'NONE', ( #6191 ), #18923, .F. ) ;
#739 = AXIS2_PLACEMENT_3D ( 'NONE', #22838, #3037, #27350 ) ;
#740 = CYLINDRICAL_SURFACE ( 'NONE', #28427, 5.000000000000000000 ) ;
#741 = ORIENTED_EDGE ( 'NONE', *, *, #6844, .T. ) ;
#742 = EDGE_CURVE ( 'NONE', #12644, #2204, #16508, .T. ) ;
#743 = CARTESIAN_POINT ( 'NONE',  ( 36.61501056740000593, -74.18926003920000767, -14.42630212289999925 ) ) ;
#744 = CARTESIAN_POINT ( 'NONE',  ( -15.62495981729999883, -101.3646851630000043, 3.472370199919999845 ) ) ;
#745 = CARTESIAN_POINT ( 'NONE',  ( 25.05740514639999716, -58.84796781909999908, 1.374148744239999997 ) ) ;
#746 = CARTESIAN_POINT ( 'NONE',  ( -20.94815322850000072, -63.05060005210000185, 15.10280677179999920 ) ) ;
#747 = EDGE_LOOP ( 'NONE', ( #26424, #26914 ) ) ;
#748 = CARTESIAN_POINT ( 'NONE',  ( -40.00000000000000000, -63.00000000000000000, 0.000000000000000000 ) ) ;
#749 = CARTESIAN_POINT ( 'NONE',  ( -13.83118819819999956, -93.00000000000000000, 21.42307711379999802 ) ) ;
#750 = CARTESIAN_POINT ( 'NONE',  ( 36.73784911806745868, -74.38638021456385729, -14.53963971729679017 ) ) ;
#751 = ORIENTED_EDGE ( 'NONE', *, *, #16283, .T. ) ;
#752 = DIRECTION ( 'NONE',  ( 1.000000000000000000, 0.000000000000000000, 0.000000000000000000 ) ) ;
#753 = CARTESIAN_POINT ( 'NONE',  ( 20.73451516309999931, -60.34941021230000047, 11.32693620240000065 ) ) ;
#754 = CARTESIAN_POINT ( 'NONE',  ( -2.664535259099999805E-15, -84.00000000000000000, -40.00000000000000000 ) ) ;
#755 = CARTESIAN_POINT ( 'NONE',  ( 15.63673621517384227, -101.5526869446983511, 3.723052656565844831 ) ) ;
#756 = CARTESIAN_POINT ( 'NONE',  ( -4.459621975350000156, -72.00000000000000000, -28.73485931899999812 ) ) ;
#757 = ORIENTED_EDGE ( 'NONE', *, *, #538, .T. ) ;
#758 = CARTESIAN_POINT ( 'NONE',  ( 46.85840109400000131, -80.01819416290000220, -2.680681327329999863 ) ) ;
#759 = CARTESIAN_POINT ( 'NONE',  ( -11.12510688389999913, -19.15751128430000350, 19.07158749389999741 ) ) ;
#760 = CARTESIAN_POINT ( 'NONE',  ( -12.19871700799999914, -59.03921360480000402, -19.98710743599999873 ) ) ;
#761 = CARTESIAN_POINT ( 'NONE',  ( 37.10328156088058194, -79.93994609586795264, -14.09141366765611636 ) ) ;
#762 = CARTESIAN_POINT ( 'NONE',  ( 24.78973582949999965, -64.24504403269999386, -10.08507979989999903 ) ) ;
#763 = CARTESIAN_POINT ( 'NONE',  ( 2.113568700161239988, -94.60931859130616317, 24.93618714997996122 ) ) ;
#764 = ORIENTED_EDGE ( 'NONE', *, *, #15472, .F. ) ;
#765 = CARTESIAN_POINT ( 'NONE',  ( 25.57735248450000043, -16.00000000000000000, 46.81902967690000139 ) ) ;
#766 = DIRECTION ( 'NONE',  ( -1.000000000000000000, 0.000000000000000000, -1.224606353820000075E-16 ) ) ;
#767 = VERTEX_POINT ( 'NONE', #4884 ) ;
#768 = CARTESIAN_POINT ( 'NONE',  ( 22.78965548680000097, -53.78538132969999452, 10.19408277159999976 ) ) ;
#769 = CARTESIAN_POINT ( 'NONE',  ( -5.360408304419999936, -101.0356131030000029, 14.51726283890000069 ) ) ;
#770 = ORIENTED_EDGE ( 'NONE', *, *, #5118, .F. ) ;
#771 = CARTESIAN_POINT ( 'NONE',  ( 45.89652019488737977, -80.18584073604786511, -4.323399995959095854 ) ) ;
#772 = ADVANCED_FACE ( 'NONE', ( #13764 ), #9092, .T. ) ;
#773 = CIRCLE ( 'NONE', #24460, 7.750000000000000000 ) ;
#774 = ORIENTED_EDGE ( 'NONE', *, *, #17934, .T. ) ;
#775 = FACE_OUTER_BOUND ( 'NONE', #22718, .T. ) ;
#776 = CARTESIAN_POINT ( 'NONE',  ( 40.00000000000000000, -80.50000000000000000, 0.000000000000000000 ) ) ;
#777 = CARTESIAN_POINT ( 'NONE',  ( 13.75178900340000077, -72.82938648530000592, 25.17248092229999656 ) ) ;
#778 = CARTESIAN_POINT ( 'NONE',  ( -10.38787484979999931, -19.16887642500000055, -20.73616781340000159 ) ) ;
#779 = CARTESIAN_POINT ( 'NONE',  ( 46.40218322401350548, -80.00000000000000000, -4.271240362889383135 ) ) ;
#780 = ORIENTED_EDGE ( 'NONE', *, *, #25866, .T. ) ;
#781 = CARTESIAN_POINT ( 'NONE',  ( -32.25831118210000170, -80.18584106479998752, -22.46797580029999963 ) ) ;
#782 = CARTESIAN_POINT ( 'NONE',  ( -20.68567502208468767, -62.76183479546326538, 12.67672343809073254 ) ) ;
#783 = CARTESIAN_POINT ( 'NONE',  ( 46.25000000000000000, -74.00000000000000000, -4.582575694960000057 ) ) ;
#784 = CARTESIAN_POINT ( 'NONE',  ( 15.50655985760000100, -100.4792519539999915, 4.667916574389999518 ) ) ;
#785 = ORIENTED_EDGE ( 'NONE', *, *, #21487, .T. ) ;
#786 = CIRCLE ( 'NONE', #28633, 0.3500000000000003664 ) ;
#787 = DIRECTION ( 'NONE',  ( 1.000000000000000000, 0.000000000000000000, 0.000000000000000000 ) ) ;
#788 = CARTESIAN_POINT ( 'NONE',  ( -12.40956463280000044, -101.1716782170000073, -9.672470230850001016 ) ) ;
#789 = CARTESIAN_POINT ( 'NONE',  ( -16.04004518150000180, -79.50000000000000000, 40.43303297039999933 ) ) ;
#790 = VERTEX_POINT ( 'NONE', #2415 ) ;
#791 = CARTESIAN_POINT ( 'NONE',  ( -16.41347552970000123, -99.62149529559999905, 6.656434160910000841 ) ) ;
#792 = CARTESIAN_POINT ( 'NONE',  ( -19.54048411309999977, -52.63055504180000099, 12.61913916920000034 ) ) ;
#793 = DIRECTION ( 'NONE',  ( 0.000000000000000000, 1.000000000000000000, 0.000000000000000000 ) ) ;
#794 = CARTESIAN_POINT ( 'NONE',  ( -19.68647263592396257, -57.47571017175199160, 12.70082573817182592 ) ) ;
#795 = DIRECTION ( 'NONE',  ( 1.000000000000000000, 0.000000000000000000, 0.000000000000000000 ) ) ;
#796 = ADVANCED_FACE ( 'NONE', ( #21061 ), #26133, .F. ) ;
#797 = CARTESIAN_POINT ( 'NONE',  ( 26.57205606840000200, -68.20221627489999605, 0.6012252253150000003 ) ) ;
#798 = ORIENTED_EDGE ( 'NONE', *, *, #9993, .T. ) ;
#799 = CARTESIAN_POINT ( 'NONE',  ( 20.49657866619999780, -57.47855601759999900, 11.20866246179999948 ) ) ;
#800 = DIRECTION ( 'NONE',  ( 1.000000000000000000, 0.000000000000000000, -1.165696672470000011E-15 ) ) ;
#801 = CARTESIAN_POINT ( 'NONE',  ( 12.48171397640000180, -98.43722862079999913, 15.12788944299999905 ) ) ;
#802 = ORIENTED_EDGE ( 'NONE', *, *, #21545, .T. ) ;
#803 = VECTOR ( 'NONE', #16768, 999.9999999999998863 ) ;
#804 = CYLINDRICAL_SURFACE ( 'NONE', #2762, 4.750000000000001776 ) ;
#805 = CARTESIAN_POINT ( 'NONE',  ( -11.67423268237357448, -95.07100787631300420, -21.41835470664000596 ) ) ;
#806 = EDGE_CURVE ( 'NONE', #21652, #15706, #7691, .T. ) ;
#807 = CARTESIAN_POINT ( 'NONE',  ( -17.09958374329999842, -92.50686295190000408, -23.80106955060000118 ) ) ;
#808 = CARTESIAN_POINT ( 'NONE',  ( -7.939103275319999042, -100.2511768809999921, 14.67510867289999865 ) ) ;
#809 = FACE_OUTER_BOUND ( 'NONE', #5937, .T. ) ;
#810 = DIRECTION ( 'NONE',  ( 1.000000000000000000, 0.000000000000000000, 0.000000000000000000 ) ) ;
#811 = CYLINDRICAL_SURFACE ( 'NONE', #10352, 0.7499999999999991118 ) ;
#812 = CYLINDRICAL_SURFACE ( 'NONE', #25089, 3.749999999999996447 ) ;
#813 = VERTEX_POINT ( 'NONE', #16669 ) ;
#814 = CARTESIAN_POINT ( 'NONE',  ( -40.29424782663165416, -74.18384006185542034, 7.244026535080610785 ) ) ;
#815 = FACE_OUTER_BOUND ( 'NONE', #4729, .T. ) ;
#816 = CARTESIAN_POINT ( 'NONE',  ( 12.08846704350000145, -99.82967635420000363, -13.24263972569999837 ) ) ;
#817 = ORIENTED_EDGE ( 'NONE', *, *, #25510, .T. ) ;
#818 = CARTESIAN_POINT ( 'NONE',  ( -2.235159051901111749, -19.47504441211092896, -22.82101578340120795 ) ) ;
#819 = CYLINDRICAL_SURFACE ( 'NONE', #10657, 0.4999999999999967804 ) ;
#820 = CARTESIAN_POINT ( 'NONE',  ( -2.495716009669999735, -52.58489974409999945, -24.49317771890000017 ) ) ;
#821 = CARTESIAN_POINT ( 'NONE',  ( -18.09364012780129372, -92.54687141712491893, 24.55341606856252312 ) ) ;
#822 = FACE_OUTER_BOUND ( 'NONE', #17874, .T. ) ;
#823 = CARTESIAN_POINT ( 'NONE',  ( 21.79230230059999940, -37.95144147500000287, -8.472395268590000583 ) ) ;
#824 = DIRECTION ( 'NONE',  ( 0.000000000000000000, -1.000000000000000000, 0.000000000000000000 ) ) ;
#825 = CARTESIAN_POINT ( 'NONE',  ( -17.12548553040000243, -99.53431416519998720, 3.156821174210000081 ) ) ;
#826 = EDGE_LOOP ( 'NONE', ( #24817, #21134, #2537, #3950, #25575 ) ) ;
#827 = CARTESIAN_POINT ( 'NONE',  ( -32.69645381549999286, -74.45114023669999881, -21.71458329279999688 ) ) ;
#828 = CYLINDRICAL_SURFACE ( 'NONE', #23410, 16.00000000000000000 ) ;
#829 = CARTESIAN_POINT ( 'NONE',  ( 7.493565752170000316, -101.1298585160000130, 13.45843171979999831 ) ) ;
#830 = ADVANCED_FACE ( 'NONE', ( #5326 ), #25668, .F. ) ;
#831 = CARTESIAN_POINT ( 'NONE',  ( -13.39422214930000088, -65.52751332760001901, 21.76797051860000209 ) ) ;
#832 = CARTESIAN_POINT ( 'NONE',  ( 20.42417383799999797, -34.94312134569999984, -8.791129100729998314 ) ) ;
#833 = CARTESIAN_POINT ( 'NONE',  ( -43.20000000000000284, -64.11445222650000630, 0.1732050807559999961 ) ) ;
#834 = EDGE_CURVE ( 'NONE', #24358, #3863, #28590, .T. ) ;
#835 = CARTESIAN_POINT ( 'NONE',  ( -1.158253037810001107, -52.63055504179944677, -23.23212522879996556 ) ) ;
#836 = CARTESIAN_POINT ( 'NONE',  ( 18.48933855830000184, -18.50000000000000000, 10.02928721039999971 ) ) ;
#837 = CARTESIAN_POINT ( 'NONE',  ( 13.81100091409999919, -101.1889999979999999, -10.51865105429999936 ) ) ;
#838 = DIRECTION ( 'NONE',  ( 1.000000000000000000, 0.000000000000000000, 0.000000000000000000 ) ) ;
#839 = ORIENTED_EDGE ( 'NONE', *, *, #4007, .T. ) ;
#840 = CARTESIAN_POINT ( 'NONE',  ( -5.459548099580000091, -101.1364147039999892, 14.34189828759999941 ) ) ;
#841 = CARTESIAN_POINT ( 'NONE',  ( -20.16249632440000283, -93.14733754460000625, 18.54048584069999706 ) ) ;
#842 = VERTEX_POINT ( 'NONE', #27887 ) ;
#843 = CARTESIAN_POINT ( 'NONE',  ( -30.43382723913022403, -92.71525149887465034, 2.010643618899957019 ) ) ;
#844 = CARTESIAN_POINT ( 'NONE',  ( 0.5993989555620130583, -100.8061861239892067, -16.64687443652875132 ) ) ;
#845 = CARTESIAN_POINT ( 'NONE',  ( -7.243718123969999922, -73.71457659610000235, 39.57993253109999898 ) ) ;
#846 = CYLINDRICAL_SURFACE ( 'NONE', #3859, 0.9999999999999991118 ) ;
#847 = CIRCLE ( 'NONE', #11969, 3.500000000000003109 ) ;
#848 = CARTESIAN_POINT ( 'NONE',  ( 23.34631240599999913, -94.16701134370001114, -7.441733273619999700 ) ) ;
#849 = CARTESIAN_POINT ( 'NONE',  ( -21.66710847110000060, -65.28157844300000079, 15.85023555240000093 ) ) ;
#850 = CARTESIAN_POINT ( 'NONE',  ( 23.87011249777025412, -92.83160374581406415, -18.98598802258993246 ) ) ;
#851 = B_SPLINE_SURFACE_WITH_KNOTS ( 'NONE', 5, 5, ( 
 ( #9154, #9307, #24622, #7287, #11483, #27396 ),
 ( #27108, #18362, #11342, #26963, #9456, #7147 ),
 ( #20248, #7000, #20389, #758, #9603, #18502 ),
 ( #7444, #315, #4654, #13978, #13830, #13530 ),
 ( #24773, #18061, #4810, #18210, #24919, #11631 ),
 ( #16304, #4949, #22735, #2776, #20541, #613 ) ),
 .UNSPECIFIED., .F., .F., .F.,
 ( 6, 6 ),
 ( 6, 6 ),
 ( 5.157533855050000504, 12.02487295920000143 ),
 ( 0.000000000000000000, 0.5000000000000000000 ),
 .UNSPECIFIED. ) ;
#852 = ORIENTED_EDGE ( 'NONE', *, *, #4107, .F. ) ;
#853 = CARTESIAN_POINT ( 'NONE',  ( -12.27142156090000036, -72.55115057349999574, -25.88050564190000102 ) ) ;
#854 = CARTESIAN_POINT ( 'NONE',  ( 7.670974394469999957, -34.59820524359999894, -21.21808786259999735 ) ) ;
#855 = DIRECTION ( 'NONE',  ( 0.5000000000001882938, 0.000000000000000000, 0.8660254037843300168 ) ) ;
#856 = CARTESIAN_POINT ( 'NONE',  ( 8.125631349740000786, -111.0000000000000000, 24.17072847820000092 ) ) ;
#857 = CARTESIAN_POINT ( 'NONE',  ( 15.34608781240000042, -101.0356131030000029, 1.995616791270000023 ) ) ;
#858 = ORIENTED_EDGE ( 'NONE', *, *, #20790, .T. ) ;
#859 = CIRCLE ( 'NONE', #18511, 57.75000000000000000 ) ;
#860 = EDGE_LOOP ( 'NONE', ( #15145, #21340, #10745, #11214 ) ) ;
#861 = EDGE_CURVE ( 'NONE', #22467, #9596, #19286, .T. ) ;
#862 = EDGE_CURVE ( 'NONE', #12242, #19473, #26277, .T. ) ;
#863 = CARTESIAN_POINT ( 'NONE',  ( 4.500000000000000000, -13.00000000000000000, -50.00000000000000000 ) ) ;
#864 = AXIS2_PLACEMENT_3D ( 'NONE', #14681, #1447, #3755 ) ;
#865 = EDGE_CURVE ( 'NONE', #22913, #452, #1848, .T. ) ;
#866 = CARTESIAN_POINT ( 'NONE',  ( -4.870171913750000137, -99.56347590840000805, 16.86609011349999676 ) ) ;
#867 = CARTESIAN_POINT ( 'NONE',  ( 1.495931207609999980, -94.52292840100000149, 23.88472403519999787 ) ) ;
#868 = ADVANCED_FACE ( 'NONE', ( #21197 ), #23938, .T. ) ;
#869 = ORIENTED_EDGE ( 'NONE', *, *, #25177, .F. ) ;
#870 = CARTESIAN_POINT ( 'NONE',  ( -20.32218854209832060, -45.95049969750532171, 14.70359657038399170 ) ) ;
#871 = ORIENTED_EDGE ( 'NONE', *, *, #18136, .T. ) ;
#872 = DIRECTION ( 'NONE',  ( 0.000000000000000000, 0.000000000000000000, -1.000000000000000000 ) ) ;
#873 = CARTESIAN_POINT ( 'NONE',  ( 21.87060598609999928, -37.33944922150000423, -8.721288104830000165 ) ) ;
#874 = CARTESIAN_POINT ( 'NONE',  ( -2.903039748510000351, -94.98812477769999418, 23.52859306979999943 ) ) ;
#875 = ORIENTED_EDGE ( 'NONE', *, *, #26119, .T. ) ;
#876 = CARTESIAN_POINT ( 'NONE',  ( 7.245634850458852583, -74.15297958040834203, -40.25190969039465472 ) ) ;
#877 = DIRECTION ( 'NONE',  ( 0.000000000000000000, -1.000000000000000000, 0.000000000000000000 ) ) ;
#878 = ORIENTED_EDGE ( 'NONE', *, *, #8574, .T. ) ;
#879 = CARTESIAN_POINT ( 'NONE',  ( -14.59919365920000089, -79.49999999010000806, 36.80099835649999562 ) ) ;
#880 = CARTESIAN_POINT ( 'NONE',  ( -1.061008937839999833, -66.63438074019998680, -25.83911337500000016 ) ) ;
#881 = FACE_OUTER_BOUND ( 'NONE', #22917, .T. ) ;
#882 = ORIENTED_EDGE ( 'NONE', *, *, #11910, .F. ) ;
#883 = CARTESIAN_POINT ( 'NONE',  ( 36.54773082250000016, -74.06528849890000288, -14.18451747229999960 ) ) ;
#884 = CARTESIAN_POINT ( 'NONE',  ( -15.68327981119999670, -101.1552388829999956, 3.291924952050000019 ) ) ;
#885 = CARTESIAN_POINT ( 'NONE',  ( 23.41606623399999876, -59.03785532109999679, -0.2656050083209999801 ) ) ;
#886 = CARTESIAN_POINT ( 'NONE',  ( -20.94814304569999663, -64.78279493969998271, 14.49686735409999905 ) ) ;
#887 = ORIENTED_EDGE ( 'NONE', *, *, #2613, .F. ) ;
#888 = LINE ( 'NONE', #4938, #18082 ) ;
#889 = CARTESIAN_POINT ( 'NONE',  ( -2.199195337949999995, -18.50000000000000000, -21.72398268019999890 ) ) ;
#890 = CARTESIAN_POINT ( 'NONE',  ( 36.58027808493192623, -74.13071341588579344, -14.24617784392711428 ) ) ;
#891 = ORIENTED_EDGE ( 'NONE', *, *, #7329, .T. ) ;
#892 = CARTESIAN_POINT ( 'NONE',  ( -12.57512920220000119, -18.50000000000000000, 18.22246578589999899 ) ) ;
#893 = CARTESIAN_POINT ( 'NONE',  ( -4.314829847440000421, -16.50000000000000000, -7.898243057010000179 ) ) ;
#894 = CARTESIAN_POINT ( 'NONE',  ( 8.963580768319998171, -35.44265701029999605, -20.01429411819999871 ) ) ;
#895 = CARTESIAN_POINT ( 'NONE',  ( 16.39931659300885514, -100.4166221066841587, 4.355705164862286871 ) ) ;
#896 = EDGE_CURVE ( 'NONE', #22615, #26338, #2075, .T. ) ;
#897 = CARTESIAN_POINT ( 'NONE',  ( -13.44405788329999929, -68.28990366489999531, 22.97003105929999833 ) ) ;
#898 = VERTEX_POINT ( 'NONE', #25850 ) ;
#899 = EDGE_CURVE ( 'NONE', #18945, #25813, #27579, .T. ) ;
#900 = CIRCLE ( 'NONE', #15733, 53.35000000000000142 ) ;
#901 = AXIS2_PLACEMENT_3D ( 'NONE', #9797, #12393, #21304 ) ;
#902 = CONTEXT_DEPENDENT_SHAPE_REPRESENTATION ( #21333, #1547 ) ;
#903 = CARTESIAN_POINT ( 'NONE',  ( -11.09626372079999967, -18.85488200820000060, 18.94417954700000450 ) ) ;
#904 = CARTESIAN_POINT ( 'NONE',  ( -11.93805380160000063, -59.03785532109999679, -20.14610571120000060 ) ) ;
#905 = FACE_OUTER_BOUND ( 'NONE', #21357, .T. ) ;
#906 = CARTESIAN_POINT ( 'NONE',  ( 3.767790178086171782, -94.00299386466799945, 25.81181420351906297 ) ) ;
#907 = EDGE_CURVE ( 'NONE', #16270, #7945, #3697, .T. ) ;
#908 = ORIENTED_EDGE ( 'NONE', *, *, #7129, .F. ) ;
#909 = CARTESIAN_POINT ( 'NONE',  ( 22.85993602570000149, -94.54719592029999831, -6.820848577220000486 ) ) ;
#910 = ORIENTED_EDGE ( 'NONE', *, *, #10616, .T. ) ;
#911 =( GEOMETRIC_REPRESENTATION_CONTEXT ( 3 ) GLOBAL_UNCERTAINTY_ASSIGNED_CONTEXT ( ( #21125 ) ) GLOBAL_UNIT_ASSIGNED_CONTEXT ( ( #27847, #5964, #28255 ) ) REPRESENTATION_CONTEXT ( 'NONE', 'WORKASPACE' ) );
#912 = CARTESIAN_POINT ( 'NONE',  ( -11.61449144829999902, -19.46147648009999997, 19.01640067170000137 ) ) ;
#913 = CARTESIAN_POINT ( 'NONE',  ( -5.598527377420000839, -101.2141467319999890, 14.18131542549999935 ) ) ;
#914 = VERTEX_POINT ( 'NONE', #15022 ) ;
#915 = FACE_OUTER_BOUND ( 'NONE', #3176, .T. ) ;
#916 = CARTESIAN_POINT ( 'NONE',  ( 39.12175830329999826, -73.75838856969998858, 7.250123850439999629 ) ) ;
#917 = CARTESIAN_POINT ( 'NONE',  ( -10.51912179628067179, -19.48459656375596083, -21.06649659360595805 ) ) ;
#918 = CARTESIAN_POINT ( 'NONE',  ( 23.52740994132569341, -94.89420224091314537, -6.742681588792337699 ) ) ;
#919 = CARTESIAN_POINT ( 'NONE',  ( 26.64667610715658341, -68.06111924181846007, 1.045321110801250342 ) ) ;
#920 = CARTESIAN_POINT ( 'NONE',  ( 9.822722921346285219, -62.32592447406135960, -24.20923697715459255 ) ) ;
#921 = ORIENTED_EDGE ( 'NONE', *, *, #8543, .F. ) ;
#922 = TOROIDAL_SURFACE ( 'NONE', #1351, 3.500000000000000000, 0.5000000000000000000 ) ;
#923 = CARTESIAN_POINT ( 'NONE',  ( -32.73892504640000567, -79.66744423050000989, -22.13232332860000184 ) ) ;
#924 = CARTESIAN_POINT ( 'NONE',  ( 19.88643906569999942, -97.93128678309999202, 2.148978528179999792 ) ) ;
#925 = CARTESIAN_POINT ( 'NONE',  ( -20.57672323510000112, -92.65509245750000389, 18.55002133529999853 ) ) ;
#926 = CARTESIAN_POINT ( 'NONE',  ( 14.80905440220000102, -101.2358105800000061, 3.500992360309999718 ) ) ;
#927 = VERTEX_POINT ( 'NONE', #21470 ) ;
#928 = CARTESIAN_POINT ( 'NONE',  ( -2.207587960610000177, -80.12576929450000307, 46.98911235669999797 ) ) ;
#929 = CARTESIAN_POINT ( 'NONE',  ( 7.687068830730000357, -29.55373640999999907, -21.02495470140000222 ) ) ;
#930 = LINE ( 'NONE', #25388, #17766 ) ;
#931 = EDGE_LOOP ( 'NONE', ( #13783, #10024, #26286, #1881 ) ) ;
#932 = CARTESIAN_POINT ( 'NONE',  ( -17.06681816329999890, -98.24294206849999966, 8.836829391780000265 ) ) ;
#933 = B_SPLINE_CURVE_WITH_KNOTS ( 'NONE', 5,
 ( #6402, #24190, #13248, #15129, #17199, #26088, #4076, #19520, #22155 ),
 .UNSPECIFIED., .F., .F.,
 ( 6, 3, 6 ),
 ( 0.000000000000000000, 1.237573681340000009, 1.566718891480000098 ),
 .UNSPECIFIED. ) ;
#934 = CARTESIAN_POINT ( 'NONE',  ( -18.92959878400000306, -32.71502530480000104, 13.33075250369999942 ) ) ;
#935 = SPHERICAL_SURFACE ( 'NONE', #9109, 2.000000494509999616 ) ;
#936 = CARTESIAN_POINT ( 'NONE',  ( -38.20072243471708617, -65.72601415636297872, 1.277196024491957571 ) ) ;
#937 = CARTESIAN_POINT ( 'NONE',  ( 22.38224740400000101, -58.97930424469999622, -8.613459702469999257 ) ) ;
#938 = EDGE_CURVE ( 'NONE', #813, #6598, #26153, .T. ) ;
#939 = CARTESIAN_POINT ( 'NONE',  ( 26.59217027070000228, -67.24447298400001216, 1.343207599729999924 ) ) ;
#940 = AXIS2_PLACEMENT_3D ( 'NONE', #13156, #4429, #22204 ) ;
#941 = EDGE_CURVE ( 'NONE', #25484, #19516, #6323, .T. ) ;
#942 = VECTOR ( 'NONE', #24106, 999.9999999999998863 ) ;
#943 = ADVANCED_FACE ( 'NONE', ( #22484 ), #23059, .T. ) ;
#944 = AXIS2_PLACEMENT_3D ( 'NONE', #27835, #25652, #10173 ) ;
#945 = ORIENTED_EDGE ( 'NONE', *, *, #24505, .F. ) ;
#946 = DIRECTION ( 'NONE',  ( 0.000000000000000000, -1.000000000000000000, 0.000000000000000000 ) ) ;
#947 = DIRECTION ( 'NONE',  ( -0.000000000000000000, 1.000000000000000000, 0.000000000000000000 ) ) ;
#948 = CARTESIAN_POINT ( 'NONE',  ( -7.325370793560000315, -19.50000000000000000, -24.94672208400000102 ) ) ;
#949 = CARTESIAN_POINT ( 'NONE',  ( 21.79230281499999933, -37.95144146749999692, -8.472394310150001218 ) ) ;
#950 = CARTESIAN_POINT ( 'NONE',  ( 7.584268328590000330, -101.6484612600000048, 14.08825304710000026 ) ) ;
#951 = ORIENTED_EDGE ( 'NONE', *, *, #1960, .T. ) ;
#952 = DIRECTION ( 'NONE',  ( 0.000000000000000000, 0.000000000000000000, -1.000000000000000000 ) ) ;
#953 = CARTESIAN_POINT ( 'NONE',  ( 47.16788169050000334, -74.59616887820000386, -1.399136062990000040 ) ) ;
#954 = CARTESIAN_POINT ( 'NONE',  ( 0.000000000000000000, -10.00000000000000000, 60.66666666670000296 ) ) ;
#955 = CARTESIAN_POINT ( 'NONE',  ( -7.808702190560000034, -100.5027207520000019, 14.25290428609999971 ) ) ;
#956 = CARTESIAN_POINT ( 'NONE',  ( 40.65853658540000026, -84.50000000000000000, -6.717799458580000049 ) ) ;
#957 = CARTESIAN_POINT ( 'NONE',  ( -36.23922253580000330, -74.50000000000000000, -27.04683438039999999 ) ) ;
#958 = DIRECTION ( 'NONE',  ( -0.7600087925152557711, 0.5000000000001688649, -0.4151946956541399114 ) ) ;
#959 = LINE ( 'NONE', #23355, #1352 ) ;
#960 = EDGE_LOOP ( 'NONE', ( #25413, #1869, #2126, #4112 ) ) ;
#961 = DIRECTION ( 'NONE',  ( 0.3687499999999825917, 0.000000000000000000, -0.9295286103719523352 ) ) ;
#962 = EDGE_CURVE ( 'NONE', #25324, #23580, #23376, .T. ) ;
#963 = DIRECTION ( 'NONE',  ( 0.3422283636740854340, 0.7003189540771749266, 0.6264448177271558782 ) ) ;
#964 = CARTESIAN_POINT ( 'NONE',  ( 11.50033716490000124, -99.57131247680000286, -13.08529392099999988 ) ) ;
#965 = ORIENTED_EDGE ( 'NONE', *, *, #6007, .F. ) ;
#966 = CARTESIAN_POINT ( 'NONE',  ( -14.24982662769999919, -74.06193868690000670, 36.58417219249999874 ) ) ;
#967 = CYLINDRICAL_SURFACE ( 'NONE', #8348, 16.00000000000000711 ) ;
#968 = CARTESIAN_POINT ( 'NONE',  ( -2.594576081490000075, -26.05152176759999705, -23.77804158390000211 ) ) ;
#969 = CARTESIAN_POINT ( 'NONE',  ( 41.00000000000000000, -84.50000000000000000, -10.20110288159999890 ) ) ;
#970 = CIRCLE ( 'NONE', #26038, 7.750000000000000000 ) ;
#971 = CARTESIAN_POINT ( 'NONE',  ( -38.00203752171322691, -65.72812580224879753, 0.9281902028072916977 ) ) ;
#972 = CARTESIAN_POINT ( 'NONE',  ( 40.70731707320000226, -82.25000000000000000, 7.215414233289999757 ) ) ;
#973 = CARTESIAN_POINT ( 'NONE',  ( 22.03392159830000097, -53.29669431010000125, -7.317502146920000783 ) ) ;
#974 = CARTESIAN_POINT ( 'NONE',  ( -16.13894939720000110, -100.3684138120000000, 2.534589637169999854 ) ) ;
#975 = ORIENTED_EDGE ( 'NONE', *, *, #2781, .F. ) ;
#976 = EDGE_CURVE ( 'NONE', #2923, #24336, #19701, .T. ) ;
#977 = B_SPLINE_CURVE_WITH_KNOTS ( 'NONE', 5,
 ( #1268, #16978, #25726, #6621, #28740, #10949, #22067, #6463, #6321, #3993, #21918, #12853 ),
 .UNSPECIFIED., .F., .F.,
 ( 6, 3, 3, 6 ),
 ( 0.000000000000000000, 0.4964111757593155927, 0.7833083924321462277, 1.000000000000000000 ),
 .UNSPECIFIED. ) ;
#978 = CARTESIAN_POINT ( 'NONE',  ( 6.983903848129999758, -101.1716782170000073, 14.09890285740000060 ) ) ;
#979 = CYLINDRICAL_SURFACE ( 'NONE', #11270, 32.39999999999999147 ) ;
#980 = CARTESIAN_POINT ( 'NONE',  ( -11.71812394180000005, -95.05064612279998926, -21.42448367849999968 ) ) ;
#981 = DIRECTION ( 'NONE',  ( 1.000000000000000000, 0.000000000000000000, 0.000000000000000000 ) ) ;
#982 = CARTESIAN_POINT ( 'NONE',  ( 36.82697894980000086, -80.49999984420000487, -13.57704391360000074 ) ) ;
#983 = CARTESIAN_POINT ( 'NONE',  ( 26.73328265790000202, -93.00000450890000536, -12.41349335419999989 ) ) ;
#984 = AXIS2_PLACEMENT_3D ( 'NONE', #22104, #28780, #24280 ) ;
#985 = CARTESIAN_POINT ( 'NONE',  ( -16.49390888960000368, -77.00000000000000000, 44.28897684009999836 ) ) ;
#986 = AXIS2_PLACEMENT_3D ( 'NONE', #22602, #25076, #15579 ) ;
#987 = ORIENTED_EDGE ( 'NONE', *, *, #21643, .T. ) ;
#988 = CARTESIAN_POINT ( 'NONE',  ( -17.05934341600000081, -99.58396357329999660, 3.231284207160000310 ) ) ;
#989 = ORIENTED_EDGE ( 'NONE', *, *, #21743, .T. ) ;
#990 = CARTESIAN_POINT ( 'NONE',  ( -41.75000000000000000, -65.14977478849999670, -2.684678751739999925 ) ) ;
#991 = ORIENTED_EDGE ( 'NONE', *, *, #7736, .F. ) ;
#992 = CARTESIAN_POINT ( 'NONE',  ( 0.5973072979270338534, -100.4166221066882656, -16.95738706857987310 ) ) ;
#993 = EDGE_CURVE ( 'NONE', #10427, #13587, #7237, .T. ) ;
#994 = CARTESIAN_POINT ( 'NONE',  ( -7.228306055930000085, -73.78142915380000488, 38.95667586449999931 ) ) ;
#995 = CARTESIAN_POINT ( 'NONE',  ( -12.53380938399999955, -99.91102932029998840, -11.37771751150000021 ) ) ;
#996 = CARTESIAN_POINT ( 'NONE',  ( 20.30102379280000235, -72.00000000000000000, -30.97095677779999789 ) ) ;
#997 = CARTESIAN_POINT ( 'NONE',  ( -6.754619094799999779, -97.17811284689999241, -19.41490638410000003 ) ) ;
#998 = CARTESIAN_POINT ( 'NONE',  ( 13.90581089109999979, -96.83679385050000121, -16.07632342850000029 ) ) ;
#999 = FACE_OUTER_BOUND ( 'NONE', #16209, .T. ) ;
#1000 = CARTESIAN_POINT ( 'NONE',  ( 8.118248377169999586, -31.57154383349999804, -20.94291994239999966 ) ) ;
#1001 = CARTESIAN_POINT ( 'NONE',  ( 0.000000000000000000, -18.50000000000000000, 0.000000000000000000 ) ) ;
#1002 = EDGE_CURVE ( 'NONE', #1715, #20804, #12259, .T. ) ;
#1003 = FILL_AREA_STYLE_COLOUR ( '', #22561 ) ;
#1004 = AXIS2_PLACEMENT_3D ( 'NONE', #7236, #15807, #16248 ) ;
#1005 = ORIENTED_EDGE ( 'NONE', *, *, #21842, .F. ) ;
#1006 = AXIS2_PLACEMENT_3D ( 'NONE', #8762, #26564, #6605 ) ;
#1007 = LINE ( 'NONE', #25323, #579 ) ;
#1008 = AXIS2_PLACEMENT_3D ( 'NONE', #14537, #28360, #12892 ) ;
#1009 = ORIENTED_EDGE ( 'NONE', *, *, #8094, .T. ) ;
#1010 = CARTESIAN_POINT ( 'NONE',  ( -2.487211299430000189, -58.24783479010000065, -24.65535445909999979 ) ) ;
#1011 = CARTESIAN_POINT ( 'NONE',  ( -2.163692630959999974, -97.01506441819999793, 20.66419130159999895 ) ) ;
#1012 = CYLINDRICAL_SURFACE ( 'NONE', #26910, 9.999999999999996447 ) ;
#1013 = VERTEX_POINT ( 'NONE', #20588 ) ;
#1014 = ORIENTED_EDGE ( 'NONE', *, *, #20847, .T. ) ;
#1015 = CARTESIAN_POINT ( 'NONE',  ( -28.90627101076691119, -93.08694455166653370, 3.225356627808906751 ) ) ;
#1016 = DIRECTION ( 'NONE',  ( -0.2414462220490755373, 0.000000000000000000, -0.9704142011833033488 ) ) ;
#1017 = CARTESIAN_POINT ( 'NONE',  ( 1.535001344007000501, -93.33134965528456917, 26.92859106544546677 ) ) ;
#1018 = VERTEX_POINT ( 'NONE', #11526 ) ;
#1019 = CIRCLE ( 'NONE', #13531, 23.79684788999999867 ) ;
#1020 = DIRECTION ( 'NONE',  ( 0.4794255386042041156, 0.000000000000000000, 0.8775825618903722036 ) ) ;
#1021 = DIRECTION ( 'NONE',  ( 0.000000000000000000, -1.000000000000000000, 0.000000000000000000 ) ) ;
#1022 = AXIS2_PLACEMENT_3D ( 'NONE', #25105, #14175, #648 ) ;
#1023 = AXIS2_PLACEMENT_3D ( 'NONE', #5325, #23241, #26231 ) ;
#1024 = CARTESIAN_POINT ( 'NONE',  ( -14.40567825890000009, -79.99130678609999734, 36.71221731090000873 ) ) ;
#1025 = B_SPLINE_CURVE_WITH_KNOTS ( 'NONE', 3,
 ( #4760, #6803, #13636, #19749, #20338, #2286 ),
 .UNSPECIFIED., .F., .F.,
 ( 4, 2, 4 ),
 ( 0.000000000000000000, 0.5000000000000000000, 1.000000000000000000 ),
 .UNSPECIFIED. ) ;
#1026 = CARTESIAN_POINT ( 'NONE',  ( 7.525098751867413505, -101.3051320485135989, 13.97834179997459891 ) ) ;
#1027 = CARTESIAN_POINT ( 'NONE',  ( -0.9701699858879999638, -66.11532834579999474, -25.60589938009999855 ) ) ;
#1028 = AXIS2_PLACEMENT_3D ( 'NONE', #28773, #22096, #8961 ) ;
#1029 = PRODUCT_DEFINITION ( 'UNKNOWN', '', #24580, #27815 ) ;
#1030 = CARTESIAN_POINT ( 'NONE',  ( -16.27748161719999942, -72.55114741090000052, 23.56761092880000064 ) ) ;
#1031 = ORIENTED_EDGE ( 'NONE', *, *, #24472, .F. ) ;
#1032 = EDGE_CURVE ( 'NONE', #16440, #21679, #3049, .T. ) ;
#1033 = CARTESIAN_POINT ( 'NONE',  ( 0.000000000000000000, -2.000000000000000000, 0.000000000000000000 ) ) ;
#1034 = CARTESIAN_POINT ( 'NONE',  ( -14.98642683749999982, -101.1746813909999929, 3.063272132379999846 ) ) ;
#1035 = CARTESIAN_POINT ( 'NONE',  ( 25.24156424050000069, -64.93834664010000779, 0.4035716298300000560 ) ) ;
#1036 = CARTESIAN_POINT ( 'NONE',  ( 36.26491344080000090, -73.99869055300000298, -14.02738897890000125 ) ) ;
#1037 = ORIENTED_EDGE ( 'NONE', *, *, #28166, .F. ) ;
#1038 = CARTESIAN_POINT ( 'NONE',  ( 7.347638122930000545E-15, -79.00000000000000000, -40.00000000000000000 ) ) ;
#1039 = ADVANCED_FACE ( 'NONE', ( #9787 ), #6268, .T. ) ;
#1040 = CARTESIAN_POINT ( 'NONE',  ( -7.288905194729153436, -73.99994620308055460, 39.62752846077490432 ) ) ;
#1041 = CARTESIAN_POINT ( 'NONE',  ( -7.919443313535407647, -100.1406256087997946, 15.25681078078310193 ) ) ;
#1042 = EDGE_LOOP ( 'NONE', ( #18545, #11786 ) ) ;
#1043 = EDGE_CURVE ( 'NONE', #4106, #10296, #15561, .T. ) ;
#1044 = FACE_OUTER_BOUND ( 'NONE', #23374, .T. ) ;
#1045 = CARTESIAN_POINT ( 'NONE',  ( 15.73209904307306495, -101.3586211804324364, 3.965908164571182670 ) ) ;
#1046 = CARTESIAN_POINT ( 'NONE',  ( 36.71918983540000880, -74.79610922010000706, -14.73254090590000054 ) ) ;
#1047 = ORIENTED_EDGE ( 'NONE', *, *, #26762, .F. ) ;
#1048 = TOROIDAL_SURFACE ( 'NONE', #18699, 57.54999999999999716, 1.000000000000000000 ) ;
#1049 = VECTOR ( 'NONE', #16313, 1000.000000000000000 ) ;
#1050 = AXIS2_PLACEMENT_3D ( 'NONE', #23123, #18318, #2882 ) ;
#1051 = CARTESIAN_POINT ( 'NONE',  ( 6.505013304209224856, -93.40023634520538565, 26.84593531204708938 ) ) ;
#1052 = EDGE_LOOP ( 'NONE', ( #19310, #18086, #18495, #5928 ) ) ;
#1053 = CARTESIAN_POINT ( 'NONE',  ( 47.25000000000000000, -75.00000000000000000, -1.242228542250000064E-12 ) ) ;
#1054 = VERTEX_POINT ( 'NONE', #22778 ) ;
#1055 = CARTESIAN_POINT ( 'NONE',  ( -10.70549402610000023, -27.06641747000000109, 19.56133743230000022 ) ) ;
#1056 = CARTESIAN_POINT ( 'NONE',  ( -6.285925807539999965, -101.5369810359999860, 14.71350185169999847 ) ) ;
#1057 = ORIENTED_EDGE ( 'NONE', *, *, #2655, .F. ) ;
#1058 = DIRECTION ( 'NONE',  ( 0.000000000000000000, 1.000000000000000000, 0.000000000000000000 ) ) ;
#1059 = AXIS2_PLACEMENT_3D ( 'NONE', #10540, #19604, #15069 ) ;
#1060 = CIRCLE ( 'NONE', #4744, 14.25000000000000000 ) ;
#1061 = CARTESIAN_POINT ( 'NONE',  ( 40.03809227200000009, -73.97913911259999509, 7.260235792989999659 ) ) ;
#1062 = CARTESIAN_POINT ( 'NONE',  ( -10.64840607053500854, -19.46749811384168893, -19.68096147938357277 ) ) ;
#1063 = CARTESIAN_POINT ( 'NONE',  ( 24.98800475346121175, -67.64340390318518814, -8.269946471920237130 ) ) ;
#1064 = CARTESIAN_POINT ( 'NONE',  ( 16.79767991550562201, -99.84800943041638277, 4.262183576306437516 ) ) ;
#1065 = VECTOR ( 'NONE', #27100, 1000.000000000000000 ) ;
#1066 = CARTESIAN_POINT ( 'NONE',  ( 46.77002716385706549, -79.85430130744032340, -3.262371211140790539 ) ) ;
#1067 = ORIENTED_EDGE ( 'NONE', *, *, #7433, .T. ) ;
#1068 = ADVANCED_FACE ( 'NONE', ( #9500, #27594, #25400, #14021, #7488, #27729 ), #16055, .F. ) ;
#1069 = CARTESIAN_POINT ( 'NONE',  ( -32.70203577369999692, -80.13412001289999864, -21.70611439569999845 ) ) ;
#1070 = CARTESIAN_POINT ( 'NONE',  ( -41.00000000000000000, -74.50000000000000000, 10.20110288159999890 ) ) ;
#1071 = CARTESIAN_POINT ( 'NONE',  ( 24.01308097620000126, -92.92146929989999649, -18.61461950569999857 ) ) ;
#1072 = ORIENTED_EDGE ( 'NONE', *, *, #1722, .F. ) ;
#1073 = CARTESIAN_POINT ( 'NONE',  ( -3.653527383279999707, -80.06168500389999565, 46.47637748780000067 ) ) ;
#1074 = CARTESIAN_POINT ( 'NONE',  ( -13.17060483900000101, -68.28989248250000799, -23.12790341000000183 ) ) ;
#1075 = ORIENTED_EDGE ( 'NONE', *, *, #3374, .F. ) ;
#1076 = ADVANCED_FACE ( 'NONE', ( #16501 ), #12110, .F. ) ;
#1077 = CARTESIAN_POINT ( 'NONE',  ( -6.717799458580000049, -84.00000000000000000, -40.65853658540000026 ) ) ;
#1078 = CARTESIAN_POINT ( 'NONE',  ( -19.73214627109999952, -19.39383846099999786, 14.41763749569999931 ) ) ;
#1079 = CARTESIAN_POINT ( 'NONE',  ( -8.209463884390000743, -99.53431386179998697, 15.35748973489999969 ) ) ;
#1080 = CARTESIAN_POINT ( 'NONE',  ( 29.01006767000000153, -74.25055803479999383, -26.50048742260000267 ) ) ;
#1081 = CARTESIAN_POINT ( 'NONE',  ( -14.92146038114265316, -71.38375628612867274, 23.72383756696897450 ) ) ;
#1082 = CARTESIAN_POINT ( 'NONE',  ( 26.61464584169999981, -68.28989939179999169, 0.1578490469770000015 ) ) ;
#1083 = AXIS2_PLACEMENT_3D ( 'NONE', #14215, #2856, #27761 ) ;
#1084 = B_SPLINE_CURVE_WITH_KNOTS ( 'NONE', 3,
 ( #28210, #4315, #23701, #17577, #6210, #21518 ),
 .UNSPECIFIED., .F., .F.,
 ( 4, 2, 4 ),
 ( 0.000000000000000000, 0.5000000000000000000, 1.000000000000000000 ),
 .UNSPECIFIED. ) ;
#1085 = ORIENTED_EDGE ( 'NONE', *, *, #16389, .T. ) ;
#1086 = LINE ( 'NONE', #18838, #1922 ) ;
#1087 = CARTESIAN_POINT ( 'NONE',  ( -38.81101221975856674, -73.50000015768027595, -7.152485405736775270 ) ) ;
#1088 = CARTESIAN_POINT ( 'NONE',  ( 20.73023592270000037, -36.12634066420000067, -8.988673776420000650 ) ) ;
#1089 = DIRECTION ( 'NONE',  ( -0.3447001089730665213, 0.000000000000000000, 0.9387128607161809857 ) ) ;
#1090 = ORIENTED_EDGE ( 'NONE', *, *, #9403, .T. ) ;
#1091 = CARTESIAN_POINT ( 'NONE',  ( 46.25000000000000000, -74.00000000000000000, -4.582575694960000057 ) ) ;
#1092 = CARTESIAN_POINT ( 'NONE',  ( -15.70782602609999756, -68.38632221809999123, 23.02257119289999920 ) ) ;
#1093 = FACE_OUTER_BOUND ( 'NONE', #11606, .T. ) ;
#1094 = CARTESIAN_POINT ( 'NONE',  ( 6.890073352990000011, -40.75155002679999683, -21.70991749099999879 ) ) ;
#1095 = CARTESIAN_POINT ( 'NONE',  ( 7.294752286439998734, -101.1411471520000021, 13.55045874839999875 ) ) ;
#1096 = EDGE_LOOP ( 'NONE', ( #26180, #28223, #1259, #7233 ) ) ;
#1097 = ADVANCED_FACE ( 'NONE', ( #2970 ), #25823, .T. ) ;
#1098 = CARTESIAN_POINT ( 'NONE',  ( -39.84605369636123129, -73.88016183364008782, 7.248366623731184788 ) ) ;
#1099 = CARTESIAN_POINT ( 'NONE',  ( 24.39453504989999999, -19.39368411259999903, 1.460252184429999822 ) ) ;
#1100 = CARTESIAN_POINT ( 'NONE',  ( 10.68340813570000059, -96.16784750930000314, -20.42747610590000207 ) ) ;
#1101 = EDGE_LOOP ( 'NONE', ( #18516, #25126, #4373, #25716 ) ) ;
#1102 = CARTESIAN_POINT ( 'NONE',  ( 19.92601281039999961, -18.61945110180000285, -8.242644266630000160 ) ) ;
#1103 = B_SPLINE_CURVE_WITH_KNOTS ( 'NONE', 3,
 ( #9770, #5554, #23742, #18682, #27581, #25387, #8018, #5415, #3375, #10178, #3240, #19095, #16908, #25801, #5827, #6247, #3923, #15110, #4358, #6542, #4056, #26358, #12787, #14974, #12922, #28246, #1743, #1892, #15250, #21839, #24171, #21695, #10730 ),
 .UNSPECIFIED., .F., .F.,
 ( 4, 2, 1, 1, 2, 2, 1, 1, 1, 2, 2, 2, 1, 1, 2, 2, 1, 1, 2, 2, 4 ),
 ( 0.000000000000000000, 0.06250000000012244372, 0.09375000000017180701, 0.1093750000001865452, 0.1171875000001930262, 0.1250000000001995071, 0.1875000000001214029, 0.2187500000000817679, 0.2343750000000625888, 0.2421875000000536238, 0.2500000000000446310, 0.3750000000000313083, 0.4375000000000246470, 0.4687500000000220379, 0.4843750000000230371, 0.5000000000000239808, 0.6250000000000188738, 0.6875000000000155431, 0.7187500000000137668, 0.7500000000000119904, 1.000000000000000000 ),
 .UNSPECIFIED. ) ;
#1104 = AXIS2_PLACEMENT_3D ( 'NONE', #1320, #19082, #16896 ) ;
#1105 = CARTESIAN_POINT ( 'NONE',  ( 11.96217641910000040, -101.6484611580000035, -10.62652795770000047 ) ) ;
#1106 = AXIS2_PLACEMENT_3D ( 'NONE', #6041, #26597, #12868 ) ;
#1107 = CARTESIAN_POINT ( 'NONE',  ( -2.573836319060000211, -39.29539198449999304, -24.78771587189999792 ) ) ;
#1108 = CARTESIAN_POINT ( 'NONE',  ( -16.54318588419999969, -93.00000000000000000, 25.62368046950000178 ) ) ;
#1109 = EDGE_CURVE ( 'NONE', #25360, #10596, #7633, .T. ) ;
#1110 = DIRECTION ( 'NONE',  ( 0.000000000000000000, -1.000000000000000000, 0.000000000000000000 ) ) ;
#1111 = CARTESIAN_POINT ( 'NONE',  ( 11.91621941349511360, -101.5902664364218992, -10.74252197561657773 ) ) ;
#1112 = CARTESIAN_POINT ( 'NONE',  ( 21.84994998139999822, -44.93330283399999558, -6.931585813899999948 ) ) ;
#1113 = CARTESIAN_POINT ( 'NONE',  ( 9.154723059868985047, -100.7167546688124986, 14.37589150456371279 ) ) ;
#1114 = CARTESIAN_POINT ( 'NONE',  ( 0.000000000000000000, -15.14308496720000008, 0.000000000000000000 ) ) ;
#1115 = VERTEX_POINT ( 'NONE', #11677 ) ;
#1116 = CARTESIAN_POINT ( 'NONE',  ( -32.73892506530000190, -74.45114023669999881, -22.13232332709999994 ) ) ;
#1117 = CARTESIAN_POINT ( 'NONE',  ( 13.79150630012393286, -97.05288880406236274, -15.91483940542160269 ) ) ;
#1118 = VECTOR ( 'NONE', #7360, 1000.000000000000000 ) ;
#1119 = CARTESIAN_POINT ( 'NONE',  ( -11.31832638660000079, -94.71194659750000255, -20.80844780490000190 ) ) ;
#1120 = CARTESIAN_POINT ( 'NONE',  ( 20.76917594449999882, -34.61672939740000032, -8.508194273930000051 ) ) ;
#1121 = CARTESIAN_POINT ( 'NONE',  ( 7.135467526410000261, -73.50000000000000000, 38.71641004229999794 ) ) ;
#1122 = CONICAL_SURFACE ( 'NONE', #9854, 11.99999999999999822, 0.02623728384790100648 ) ;
#1123 = DIRECTION ( 'NONE',  ( 0.000000000000000000, 1.000000000000000000, 0.000000000000000000 ) ) ;
#1124 = AXIS2_PLACEMENT_3D ( 'NONE', #20115, #24488, #15589 ) ;
#1125 = CARTESIAN_POINT ( 'NONE',  ( -18.09563929800284754, -93.31462968090272625, -21.26308191278070936 ) ) ;
#1126 = CARTESIAN_POINT ( 'NONE',  ( 20.15266352549999951, -28.56548694950000211, -8.805377537309999170 ) ) ;
#1127 = ORIENTED_EDGE ( 'NONE', *, *, #23270, .T. ) ;
#1128 = CARTESIAN_POINT ( 'NONE',  ( 8.069590842209999337, -101.0685850230000113, 13.92289867959999938 ) ) ;
#1129 = CARTESIAN_POINT ( 'NONE',  ( -17.03413894869999723, -99.61736770250000461, 3.268853260370000235 ) ) ;
#1130 = ORIENTED_EDGE ( 'NONE', *, *, #22043, .T. ) ;
#1131 = CYLINDRICAL_SURFACE ( 'NONE', #24779, 61.34999999999998721 ) ;
#1132 = ORIENTED_EDGE ( 'NONE', *, *, #23898, .T. ) ;
#1133 = EDGE_CURVE ( 'NONE', #17770, #10479, #13657, .T. ) ;
#1134 = ADVANCED_FACE ( 'NONE', ( #21028 ), #16056, .T. ) ;
#1135 = CARTESIAN_POINT ( 'NONE',  ( 0.5079992097761589775, -100.1240332945069724, -17.19565627508607264 ) ) ;
#1136 = DIRECTION ( 'NONE',  ( 0.000000000000000000, -1.000000000000000000, 0.000000000000000000 ) ) ;
#1137 = AXIS2_PLACEMENT_3D ( 'NONE', #6987, #7132, #23919 ) ;
#1138 = CARTESIAN_POINT ( 'NONE',  ( 13.25691510293539821, -92.77521214512113090, 27.46826507470851197 ) ) ;
#1139 = DIRECTION ( 'NONE',  ( 1.256627704189999682E-15, 0.000000000000000000, 1.000000000000000000 ) ) ;
#1140 = CARTESIAN_POINT ( 'NONE',  ( 25.08083557389999996, -74.00200704200000246, -30.10596417070000186 ) ) ;
#1141 = EDGE_CURVE ( 'NONE', #11892, #3141, #15331, .T. ) ;
#1142 = CARTESIAN_POINT ( 'NONE',  ( 0.000000000000000000, -2.000000000000000000, 0.000000000000000000 ) ) ;
#1143 = CARTESIAN_POINT ( 'NONE',  ( 13.12744029750000152, -94.59276292389999696, -19.84843707589999795 ) ) ;
#1144 = PLANE ( 'NONE',  #4134 ) ;
#1145 = DIRECTION ( 'NONE',  ( 1.000000000000000000, 0.000000000000000000, 0.000000000000000000 ) ) ;
#1146 = DIRECTION ( 'NONE',  ( 1.000000000000000000, 0.000000000000000000, 0.000000000000000000 ) ) ;
#1147 = ORIENTED_EDGE ( 'NONE', *, *, #17104, .T. ) ;
#1148 = CARTESIAN_POINT ( 'NONE',  ( -39.83713413880786902, -63.35496135694597086, -2.175426268797550744 ) ) ;
#1149 = VERTEX_POINT ( 'NONE', #23899 ) ;
#1150 = CONICAL_SURFACE ( 'NONE', #12714, 21.60095686220001454, 0.7949521073230001456 ) ;
#1151 = EDGE_CURVE ( 'NONE', #12597, #24336, #725, .T. ) ;
#1152 = LINE ( 'NONE', #7700, #5344 ) ;
#1153 = CARTESIAN_POINT ( 'NONE',  ( 9.270563563040001398, -37.35781407409999844, -22.45851363030000059 ) ) ;
#1154 = CARTESIAN_POINT ( 'NONE',  ( -28.83106611000000186, -92.65997669530000280, 3.154919777930000002 ) ) ;
#1155 = ORIENTED_EDGE ( 'NONE', *, *, #25039, .F. ) ;
#1156 = B_SPLINE_CURVE_WITH_KNOTS ( 'NONE', 5,
 ( #23277, #12450, #10265, #1421, #25605, #23417 ),
 .UNSPECIFIED., .F., .F.,
 ( 6, 6 ),
 ( 0.000000000000000000, 1.000000000000000000 ),
 .UNSPECIFIED. ) ;
#1157 = ORIENTED_EDGE ( 'NONE', *, *, #26762, .T. ) ;
#1158 = DIRECTION ( 'NONE',  ( -0.7600087925152557711, -0.5000000000001688649, -0.4151946956541399114 ) ) ;
#1159 = EDGE_LOOP ( 'NONE', ( #5660, #9858, #7477, #25278 ) ) ;
#1160 = VECTOR ( 'NONE', #22914, 1000.000000000000000 ) ;
#1161 = CARTESIAN_POINT ( 'NONE',  ( 0.000000000000000000, -82.50000000000000000, 0.000000000000000000 ) ) ;
#1162 = CARTESIAN_POINT ( 'NONE',  ( 9.009289338599998587, -35.83210504610000413, -20.15582154950000060 ) ) ;
#1163 = ORIENTED_EDGE ( 'NONE', *, *, #18541, .F. ) ;
#1164 = CARTESIAN_POINT ( 'NONE',  ( -21.99985828019999801, -74.00000000000000000, -31.89935321680000158 ) ) ;
#1165 = VERTEX_POINT ( 'NONE', #25529 ) ;
#1166 = CARTESIAN_POINT ( 'NONE',  ( -14.70126722260000030, -101.0847364069999941, 4.628494549459999163 ) ) ;
#1167 = CARTESIAN_POINT ( 'NONE',  ( -16.54766221710000096, -100.0428544680000016, 2.640864489020000150 ) ) ;
#1168 = CARTESIAN_POINT ( 'NONE',  ( 24.90432507590000455, -60.33034294479999460, 1.297259702619999899 ) ) ;
#1169 = CARTESIAN_POINT ( 'NONE',  ( -20.31915794119999674, -62.12743832499999996, 12.73748489189999944 ) ) ;
#1170 = ORIENTED_EDGE ( 'NONE', *, *, #26606, .F. ) ;
#1171 = AXIS2_PLACEMENT_3D ( 'NONE', #20331, #24861, #13775 ) ;
#1172 = CARTESIAN_POINT ( 'NONE',  ( 23.93312658989999875, -65.07443093669999712, -7.727579958389999781 ) ) ;
#1173 = CARTESIAN_POINT ( 'NONE',  ( -7.258712132442814990, -74.00006796125886410, 39.81159221151552430 ) ) ;
#1174 = CARTESIAN_POINT ( 'NONE',  ( 0.000000000000000000, -17.50000000000000000, 9.099999999999999645 ) ) ;
#1175 = VERTEX_POINT ( 'NONE', #1628 ) ;
#1176 = B_SPLINE_CURVE_WITH_KNOTS ( 'NONE', 3,
 ( #23554, #16856, #14788, #12593, #8521, #3457, #12323, #25746, #6787, #4303, #11276, #20033, #22529, #19876, #28761, #256, #17713 ),
 .UNSPECIFIED., .F., .F.,
 ( 4, 2, 2, 2, 1, 1, 1, 2, 2, 4 ),
 ( 0.000000000000000000, 0.2499999999998541722, 0.3749999999997812861, 0.4374999999997471467, 0.4687499999997326028, 0.4843749999997279954, 0.4921874999997256639, 0.4960937499997272182, 0.4999999999997287725, 1.000000000000000000 ),
 .UNSPECIFIED. ) ;
#1177 = CARTESIAN_POINT ( 'NONE',  ( -41.66730568001332102, -65.09474816372230066, -2.847883582410218661 ) ) ;
#1178 = CARTESIAN_POINT ( 'NONE',  ( -31.89935321680000158, -74.00000000000000000, -21.99985828019999801 ) ) ;
#1179 = CARTESIAN_POINT ( 'NONE',  ( 36.65640604229999866, -79.86805848820000620, -14.39612937579999929 ) ) ;
#1180 = DIRECTION ( 'NONE',  ( 1.000000000000000000, 0.000000000000000000, 0.000000000000000000 ) ) ;
#1181 = VERTEX_POINT ( 'NONE', #28133 ) ;
#1182 = AXIS2_PLACEMENT_3D ( 'NONE', #13757, #17697, #2120 ) ;
#1183 = ADVANCED_FACE ( 'NONE', ( #3658 ), #21474, .T. ) ;
#1184 = VECTOR ( 'NONE', #12556, 1000.000000000000000 ) ;
#1185 = CARTESIAN_POINT ( 'NONE',  ( -2.679427010961042299, -80.39259899117686814, 46.73670472467608761 ) ) ;
#1186 = EDGE_CURVE ( 'NONE', #5075, #17731, #27244, .T. ) ;
#1187 = VERTEX_POINT ( 'NONE', #12940 ) ;
#1188 = CARTESIAN_POINT ( 'NONE',  ( -17.91520637925930615, -98.72564645249281057, 4.448055852924632347 ) ) ;
#1189 = ORIENTED_EDGE ( 'NONE', *, *, #11802, .T. ) ;
#1190 = VECTOR ( 'NONE', #1655, 1000.000000000000000 ) ;
#1191 = CARTESIAN_POINT ( 'NONE',  ( 22.76317971519999972, -52.57401960349999825, 10.17780311019999928 ) ) ;
#1192 = CARTESIAN_POINT ( 'NONE',  ( -5.983771968930000185, -101.2459394079999981, 14.78967057790000084 ) ) ;
#1193 = EDGE_CURVE ( 'NONE', #6398, #23740, #108, .T. ) ;
#1194 = EDGE_LOOP ( 'NONE', ( #8651, #2603, #6295, #28164 ) ) ;
#1195 = CARTESIAN_POINT ( 'NONE',  ( -4.115583105835526112, -96.89152197809237066, -20.86381302798665160 ) ) ;
#1196 = EDGE_CURVE ( 'NONE', #14426, #19773, #20727, .T. ) ;
#1197 = CARTESIAN_POINT ( 'NONE',  ( 38.68350846249999364, -73.93831524339999817, 7.318371247189999984 ) ) ;
#1198 = CARTESIAN_POINT ( 'NONE',  ( -13.01174968712481217, -101.6407018583229416, -9.320898687691189011 ) ) ;
#1199 = CARTESIAN_POINT ( 'NONE',  ( -11.90443957499999961, -64.24504445130001784, -23.68393584109999850 ) ) ;
#1200 = CARTESIAN_POINT ( 'NONE',  ( 47.01215786981062195, -79.64739487177904209, -2.324349206678411939 ) ) ;
#1201 = ORIENTED_EDGE ( 'NONE', *, *, #3911, .F. ) ;
#1202 = DIRECTION ( 'NONE',  ( 0.000000000000000000, 1.000000000000000000, 0.000000000000000000 ) ) ;
#1203 = DIRECTION ( 'NONE',  ( 0.7071067811865470176, 0.000000000000000000, 0.7071067811865480168 ) ) ;
#1204 = CARTESIAN_POINT ( 'NONE',  ( -20.43643619460000238, -93.49011727610000833, 16.37406953600000037 ) ) ;
#1205 = CARTESIAN_POINT ( 'NONE',  ( 16.79922297439999923, -99.53431386179998697, 4.586272525910000120 ) ) ;
#1206 = EDGE_LOOP ( 'NONE', ( #19518, #1380, #945, #25945 ) ) ;
#1207 = VECTOR ( 'NONE', #24957, 1000.000000000000000 ) ;
#1208 = CARTESIAN_POINT ( 'NONE',  ( 14.05983645159999895, -99.53431386179998697, -10.27466725399999881 ) ) ;
#1209 = CARTESIAN_POINT ( 'NONE',  ( -41.45000000000000284, -63.07912966450000880, -2.857883832489999776 ) ) ;
#1210 = ORIENTED_EDGE ( 'NONE', *, *, #15889, .F. ) ;
#1211 = CARTESIAN_POINT ( 'NONE',  ( 7.102042752109999135, -101.6484611540000031, 14.33739825589999839 ) ) ;
#1212 = FACE_OUTER_BOUND ( 'NONE', #25199, .T. ) ;
#1213 = CARTESIAN_POINT ( 'NONE',  ( 6.019093083229999586, -92.50000000000000000, 29.30685818879999971 ) ) ;
#1214 = CARTESIAN_POINT ( 'NONE',  ( 30.21390923379999904, -74.22140788000000100, -25.07573566509999807 ) ) ;
#1215 = CARTESIAN_POINT ( 'NONE',  ( -14.49981904734982585, -70.55987052708249507, 23.54264869499610313 ) ) ;
#1216 = ADVANCED_FACE ( 'NONE', ( #13541 ), #4022, .F. ) ;
#1217 = ORIENTED_EDGE ( 'NONE', *, *, #10543, .T. ) ;
#1218 = CARTESIAN_POINT ( 'NONE',  ( 21.39481749499999808, -35.54838723460000693, -7.344946279170000203 ) ) ;
#1219 = ADVANCED_FACE ( 'NONE', ( #5396 ), #28141, .T. ) ;
#1220 = ORIENTED_EDGE ( 'NONE', *, *, #18993, .F. ) ;
#1221 = DIRECTION ( 'NONE',  ( 0.000000000000000000, -1.000000000000000000, 0.000000000000000000 ) ) ;
#1222 = EDGE_CURVE ( 'NONE', #14011, #25949, #25369, .T. ) ;
#1223 = DIRECTION ( 'NONE',  ( 1.000000000000000000, 0.000000000000000000, 0.000000000000000000 ) ) ;
#1224 = VERTEX_POINT ( 'NONE', #14279 ) ;
#1225 = B_SPLINE_CURVE_WITH_KNOTS ( 'NONE', 5,
 ( #21036, #1092, #5574, #21170, #5707, #20892 ),
 .UNSPECIFIED., .F., .F.,
 ( 6, 6 ),
 ( 0.000000000000000000, 1.000000000000000000 ),
 .UNSPECIFIED. ) ;
#1226 = DIRECTION ( 'NONE',  ( 0.09756097560976760563, 0.000000000000000000, 0.9952295494196654602 ) ) ;
#1227 = DIRECTION ( 'NONE',  ( -0.7071067811865470176, 0.000000000000000000, 0.7071067811865480168 ) ) ;
#1228 = CARTESIAN_POINT ( 'NONE',  ( 0.000000000000000000, -36.20000000000000284, 0.000000000000000000 ) ) ;
#1229 = DIRECTION ( 'NONE',  ( 0.000000000000000000, 1.000000000000000000, 0.000000000000000000 ) ) ;
#1230 = ORIENTED_EDGE ( 'NONE', *, *, #13863, .F. ) ;
#1231 = CARTESIAN_POINT ( 'NONE',  ( -43.29730172082344808, -65.09619745167302085, 0.03908829158085567329 ) ) ;
#1232 = CARTESIAN_POINT ( 'NONE',  ( -23.87286787420000067, -93.96464232239999603, -7.079520382630000164 ) ) ;
#1233 = DIRECTION ( 'NONE',  ( 1.000000000000000000, 0.000000000000000000, 0.000000000000000000 ) ) ;
#1234 = VERTEX_POINT ( 'NONE', #26969 ) ;
#1235 = CARTESIAN_POINT ( 'NONE',  ( -40.00000000000000000, -94.00000000000000000, 0.000000000000000000 ) ) ;
#1236 = CARTESIAN_POINT ( 'NONE',  ( -14.04941245390000049, -74.01263034700001242, 36.28249488850000404 ) ) ;
#1237 = CARTESIAN_POINT ( 'NONE',  ( -41.74999999999191402, -63.07120704560062308, -2.719973428251394321 ) ) ;
#1238 = DIRECTION ( 'NONE',  ( 0.000000000000000000, 1.000000000000000000, 0.000000000000000000 ) ) ;
#1239 = DIRECTION ( 'NONE',  ( 0.4794255386042000078, 0.000000000000000000, 0.8775825618903743131 ) ) ;
#1240 = DIRECTION ( 'NONE',  ( 0.000000000000000000, -1.000000000000000000, 0.000000000000000000 ) ) ;
#1241 = CARTESIAN_POINT ( 'NONE',  ( 21.75421831149999718, -44.93343662089999668, -7.233371418780000006 ) ) ;
#1242 = DIRECTION ( 'NONE',  ( 0.3639667172450259391, 0.000000000000000000, -0.9314119543670669188 ) ) ;
#1243 = CARTESIAN_POINT ( 'NONE',  ( -11.04661350269999964, -27.06679042429999882, -19.46499051269999825 ) ) ;
#1244 = ORIENTED_EDGE ( 'NONE', *, *, #11232, .T. ) ;
#1245 = DIRECTION ( 'NONE',  ( -1.000000000000000000, 0.000000000000000000, 0.000000000000000000 ) ) ;
#1246 = DIRECTION ( 'NONE',  ( 0.000000000000000000, 1.000000000000000000, 0.000000000000000000 ) ) ;
#1247 = ADVANCED_FACE ( 'NONE', ( #16022 ), #20850, .T. ) ;
#1248 = VECTOR ( 'NONE', #13164, 1000.000000000000114 ) ;
#1249 = EDGE_CURVE ( 'NONE', #21436, #3079, #22329, .T. ) ;
#1250 = CARTESIAN_POINT ( 'NONE',  ( -11.40589454009999848, -95.08268351149999376, -21.37599873950000173 ) ) ;
#1251 = CARTESIAN_POINT ( 'NONE',  ( 8.985156090609999424, -35.55399656489999671, -19.52064371570000034 ) ) ;
#1252 = DIRECTION ( 'NONE',  ( 0.4794255386042040601, 0.000000000000000000, 0.8775825618903720926 ) ) ;
#1253 = LINE ( 'NONE', #23245, #1839 ) ;
#1254 = ADVANCED_FACE ( 'NONE', ( #18664 ), #27557, .F. ) ;
#1255 = CARTESIAN_POINT ( 'NONE',  ( -18.58238019774981353, -93.25521310994808744, -21.15957345179030469 ) ) ;
#1256 = EDGE_CURVE ( 'NONE', #22342, #8389, #23961, .T. ) ;
#1257 = B_SPLINE_SURFACE_WITH_KNOTS ( 'NONE', 5, 5, ( 
 ( #7609, #16473, #20997, #25376, #27970, #8008 ),
 ( #18816, #9618, #23463, #10166, #12229, #27704 ),
 ( #1061, #7743, #9900, #16610, #27411, #19085 ),
 ( #21269, #7463, #3502, #12360, #20857, #25504 ),
 ( #16322, #25233, #916, #23048, #3091, #5539 ),
 ( #9759, #14427, #21140, #1197, #10032, #18946 ) ),
 .UNSPECIFIED., .F., .F., .F.,
 ( 6, 6 ),
 ( 6, 6 ),
 ( 9.300133431499999221E-14, 3.318582255960000005 ),
 ( 0.000000000000000000, 0.5000000000000000000 ),
 .UNSPECIFIED. ) ;
#1258 = CARTESIAN_POINT ( 'NONE',  ( -4.500000000000000000, -15.00000000000000000, 40.50000000000000000 ) ) ;
#1259 = ORIENTED_EDGE ( 'NONE', *, *, #23716, .F. ) ;
#1260 = CARTESIAN_POINT ( 'NONE',  ( 21.56931447779999900, -36.56979901409999911, -6.850353625240000355 ) ) ;
#1261 = FACE_OUTER_BOUND ( 'NONE', #13577, .T. ) ;
#1262 = ORIENTED_EDGE ( 'NONE', *, *, #8790, .F. ) ;
#1263 = CARTESIAN_POINT ( 'NONE',  ( -13.18221367349999973, -68.65989719860000662, -23.31533323539999714 ) ) ;
#1264 = CARTESIAN_POINT ( 'NONE',  ( 0.3228164666304381702, -101.4085864806541650, -16.18225634051029971 ) ) ;
#1265 = B_SPLINE_CURVE_WITH_KNOTS ( 'NONE', 3,
 ( #13229, #2179, #13678, #8853 ),
 .UNSPECIFIED., .F., .F.,
 ( 4, 4 ),
 ( 0.000000000000000000, 1.000000000000000000 ),
 .UNSPECIFIED. ) ;
#1266 = DIRECTION ( 'NONE',  ( 1.000000000000000000, 0.000000000000000000, -1.203338504109999799E-16 ) ) ;
#1267 = DIRECTION ( 'NONE',  ( 1.000000000000000000, 0.000000000000000000, 0.000000000000000000 ) ) ;
#1268 = CARTESIAN_POINT ( 'NONE',  ( -8.209463884390000743, -99.53431386179998697, 15.35748973489999969 ) ) ;
#1269 = DIRECTION ( 'NONE',  ( 1.000000000000000000, 0.000000000000000000, 0.000000000000000000 ) ) ;
#1270 = CARTESIAN_POINT ( 'NONE',  ( 16.42966103859999905, -94.59276292389999696, 17.21499949629999904 ) ) ;
#1271 = DIRECTION ( 'NONE',  ( 0.000000000000000000, -1.000000000000000000, 0.000000000000000000 ) ) ;
#1272 = DIRECTION ( 'NONE',  ( 1.000000000000000000, 0.000000000000000000, 0.000000000000000000 ) ) ;
#1273 = CARTESIAN_POINT ( 'NONE',  ( -41.74156629096919602, -63.06504043304209262, 2.752751128773220479 ) ) ;
#1274 = ORIENTED_EDGE ( 'NONE', *, *, #6243, .T. ) ;
#1275 = DIRECTION ( 'NONE',  ( 1.000000000000000000, 0.000000000000000000, 0.000000000000000000 ) ) ;
#1276 = EDGE_LOOP ( 'NONE', ( #8134, #14105, #8144, #14741 ) ) ;
#1277 = DIRECTION ( 'NONE',  ( 1.000000000000000000, 0.000000000000000000, -5.551115123130000643E-17 ) ) ;
#1278 = EDGE_CURVE ( 'NONE', #22412, #22777, #20587, .T. ) ;
#1279 = EDGE_LOOP ( 'NONE', ( #21889, #21162, #7938, #25017 ) ) ;
#1280 = CARTESIAN_POINT ( 'NONE',  ( -14.01337423630000067, -80.50000000000000000, 36.66316738249999929 ) ) ;
#1281 = CARTESIAN_POINT ( 'NONE',  ( -28.19807706989999829, -92.76550115769998683, 1.645633876470000034 ) ) ;
#1282 = CARTESIAN_POINT ( 'NONE',  ( -19.81272040990000249, -52.63293862069999562, 12.05498172269999912 ) ) ;
#1283 = ORIENTED_EDGE ( 'NONE', *, *, #9843, .F. ) ;
#1284 = DIRECTION ( 'NONE',  ( 0.4794255386042036160, 0.000000000000000000, 0.8775825618903723147 ) ) ;
#1285 = ORIENTED_EDGE ( 'NONE', *, *, #14765, .T. ) ;
#1286 = DIRECTION ( 'NONE',  ( -1.000000000000000000, 0.000000000000000000, 0.000000000000000000 ) ) ;
#1287 = DIRECTION ( 'NONE',  ( -0.4692400087391606633, 0.000000000000000000, 0.8830706733883038062 ) ) ;
#1288 = EDGE_LOOP ( 'NONE', ( #18758, #28729, #17531 ) ) ;
#1289 = CARTESIAN_POINT ( 'NONE',  ( -41.75000000000000000, -65.63577453799999262, 1.587713240270000048 ) ) ;
#1290 = CARTESIAN_POINT ( 'NONE',  ( -17.47679617029999832, -18.50000000000000000, 12.54464522169999796 ) ) ;
#1291 = ORIENTED_EDGE ( 'NONE', *, *, #22231, .F. ) ;
#1292 = CARTESIAN_POINT ( 'NONE',  ( -14.61698170120000029, -101.1363384779999990, 4.673707807969999628 ) ) ;
#1293 = AXIS2_PLACEMENT_3D ( 'NONE', #11079, #4557, #24376 ) ;
#1294 = CARTESIAN_POINT ( 'NONE',  ( -15.04689636610000036, -101.1175442680000032, 3.135183322060000499 ) ) ;
#1295 = CARTESIAN_POINT ( 'NONE',  ( -32.02433178753376808, -74.00000000000001421, -22.03106757217172884 ) ) ;
#1296 = CARTESIAN_POINT ( 'NONE',  ( -21.20809654359999641, -65.04696944340000186, 13.49691729160000087 ) ) ;
#1297 = EDGE_CURVE ( 'NONE', #15559, #11794, #14645, .T. ) ;
#1298 = ORIENTED_EDGE ( 'NONE', *, *, #3350, .F. ) ;
#1299 = CIRCLE ( 'NONE', #22695, 52.86371681420000357 ) ;
#1300 = CARTESIAN_POINT ( 'NONE',  ( -1.804107087350000027, -18.50000000000000000, -21.15426956649999823 ) ) ;
#1301 = CARTESIAN_POINT ( 'NONE',  ( -7.728319723075819603, -100.8738282916487208, 14.69600823143309576 ) ) ;
#1302 = ORIENTED_EDGE ( 'NONE', *, *, #17974, .F. ) ;
#1303 = CARTESIAN_POINT ( 'NONE',  ( -41.57851898686420355, -65.10052340105812618, -2.886766141929010931 ) ) ;
#1304 = TOROIDAL_SURFACE ( 'NONE', #15678, 43.34897771020000334, 20.00000000000000000 ) ;
#1305 = CYLINDRICAL_SURFACE ( 'NONE', #864, 0.4999999999999982236 ) ;
#1306 = CARTESIAN_POINT ( 'NONE',  ( 37.14416535689999677, -79.97680490119999774, -14.02189532789999937 ) ) ;
#1307 = ORIENTED_EDGE ( 'NONE', *, *, #295, .F. ) ;
#1308 = EDGE_CURVE ( 'NONE', #23834, #22763, #12324, .T. ) ;
#1309 = PRODUCT ( 'Pump Drive Shaft', 'Pump Drive Shaft', '', ( #7289 ) ) ;
#1310 = CARTESIAN_POINT ( 'NONE',  ( 6.719631698796779240, -100.6644468679725009, 15.36513027133983122 ) ) ;
#1311 = CARTESIAN_POINT ( 'NONE',  ( -9.356041104380000917, -84.50000000000000000, -37.60355029590000697 ) ) ;
#1312 = EDGE_LOOP ( 'NONE', ( #4453, #28583, #27849, #15878 ) ) ;
#1313 = CIRCLE ( 'NONE', #17574, 11.00000000000000000 ) ;
#1314 = CARTESIAN_POINT ( 'NONE',  ( 0.000000000000000000, -101.6484611540000031, 0.000000000000000000 ) ) ;
#1315 = CARTESIAN_POINT ( 'NONE',  ( 46.50724168351928967, -73.67599622268748760, -3.197465198608631987 ) ) ;
#1316 = ORIENTED_EDGE ( 'NONE', *, *, #18744, .F. ) ;
#1317 = CARTESIAN_POINT ( 'NONE',  ( 27.46713810829999858, -92.96321833979999383, 9.765138773850001286 ) ) ;
#1318 = CARTESIAN_POINT ( 'NONE',  ( -6.045971696259999639, -101.1411470200000053, 14.15183991680000020 ) ) ;
#1319 = ORIENTED_EDGE ( 'NONE', *, *, #10244, .F. ) ;
#1320 = CARTESIAN_POINT ( 'NONE',  ( 0.000000000000000000, -2.000000000000000000, 8.099999999999999645 ) ) ;
#1321 = DIRECTION ( 'NONE',  ( 0.000000000000000000, -1.000000000000000000, 0.000000000000000000 ) ) ;
#1322 = B_SPLINE_CURVE_WITH_KNOTS ( 'NONE', 3,
 ( #23215, #18848, #20749, #25270, #16205, #16643 ),
 .UNSPECIFIED., .F., .F.,
 ( 4, 2, 4 ),
 ( 0.000000000000000000, 0.5000000000000000000, 1.000000000000000000 ),
 .UNSPECIFIED. ) ;
#1323 = AXIS2_PLACEMENT_3D ( 'NONE', #7852, #12345, #17150 ) ;
#1324 = CARTESIAN_POINT ( 'NONE',  ( 0.000000000000000000, -84.75000000000000000, 0.000000000000000000 ) ) ;
#1325 = CARTESIAN_POINT ( 'NONE',  ( 9.027382853569999810, -36.23976085289999816, -21.24216557319999765 ) ) ;
#1326 = DIRECTION ( 'NONE',  ( 0.000000000000000000, 1.000000000000000000, 0.000000000000000000 ) ) ;
#1327 = CARTESIAN_POINT ( 'NONE',  ( 9.993770587066137523, -63.70931641282978575, -24.60213562706236345 ) ) ;
#1328 = ORIENTED_EDGE ( 'NONE', *, *, #25383, .F. ) ;
#1329 = CARTESIAN_POINT ( 'NONE',  ( -20.52527758500000132, -95.75647260690000451, -9.198302384599999826 ) ) ;
#1330 = CARTESIAN_POINT ( 'NONE',  ( 9.017788245969780903, -92.49999918155076273, -27.43400824161624385 ) ) ;
#1331 = EDGE_CURVE ( 'NONE', #15974, #19973, #5320, .T. ) ;
#1332 = CARTESIAN_POINT ( 'NONE',  ( 24.73701769899999903, -93.39359504719999450, -11.28691117220000173 ) ) ;
#1333 = CARTESIAN_POINT ( 'NONE',  ( -2.579354798150000239, -53.77454410920000072, -25.14349222919999960 ) ) ;
#1334 = CARTESIAN_POINT ( 'NONE',  ( -2.180054726419999866, -80.20928067410000040, 46.97828202600000225 ) ) ;
#1335 = CARTESIAN_POINT ( 'NONE',  ( 0.000000000000000000, -90.50000000000000000, 0.000000000000000000 ) ) ;
#1336 = EDGE_LOOP ( 'NONE', ( #27422, #1067, #8213, #19531 ) ) ;
#1337 = CIRCLE ( 'NONE', #5040, 55.67692378859999991 ) ;
#1338 = FACE_OUTER_BOUND ( 'NONE', #23635, .T. ) ;
#1339 = AXIS2_PLACEMENT_3D ( 'NONE', #8246, #19612, #25892 ) ;
#1340 = DIRECTION ( 'NONE',  ( 0.000000000000000000, 1.000000000000000000, 0.000000000000000000 ) ) ;
#1341 = CARTESIAN_POINT ( 'NONE',  ( 21.94462607333390380, -96.36359510713519683, -0.1463646804548337788 ) ) ;
#1342 = CARTESIAN_POINT ( 'NONE',  ( 23.96368475870000125, -101.1889999979999999, 8.717328305520000598 ) ) ;
#1343 = ADVANCED_FACE ( 'NONE', ( #6078 ), #19840, .T. ) ;
#1344 = DIRECTION ( 'NONE',  ( 1.000000000000000000, 0.000000000000000000, 0.000000000000000000 ) ) ;
#1345 = ORIENTED_EDGE ( 'NONE', *, *, #4475, .F. ) ;
#1346 = CARTESIAN_POINT ( 'NONE',  ( 20.95510899789999826, -35.33620304099999743, -8.408939718540000996 ) ) ;
#1347 = CARTESIAN_POINT ( 'NONE',  ( 20.41714882420000166, -35.80913068420000656, -8.862965437090000620 ) ) ;
#1348 = CARTESIAN_POINT ( 'NONE',  ( 28.07036528529999941, -39.32601556110000018, 51.38245899869999533 ) ) ;
#1349 = VERTEX_POINT ( 'NONE', #16743 ) ;
#1350 = CARTESIAN_POINT ( 'NONE',  ( -12.36495966000000024, -101.1848541609999899, -8.980491836739998845 ) ) ;
#1351 = AXIS2_PLACEMENT_3D ( 'NONE', #26615, #26327, #12885 ) ;
#1352 = VECTOR ( 'NONE', #1229, 1000.000000000000000 ) ;
#1353 = DIRECTION ( 'NONE',  ( 0.4794255386042041156, 0.000000000000000000, 0.8775825618903722036 ) ) ;
#1354 = CARTESIAN_POINT ( 'NONE',  ( 1.673545578960000224, -92.65509162889999573, 27.65323681370000131 ) ) ;
#1355 = CARTESIAN_POINT ( 'NONE',  ( 7.482057485060000346, -36.56833510180000246, -21.43629755389999758 ) ) ;
#1356 = LINE ( 'NONE', #11841, #17621 ) ;
#1357 = ORIENTED_EDGE ( 'NONE', *, *, #15472, .T. ) ;
#1358 = CARTESIAN_POINT ( 'NONE',  ( 12.66014534235611322, -101.5526869446726153, -9.904007292906472415 ) ) ;
#1359 = B_SPLINE_CURVE_WITH_KNOTS ( 'NONE', 3,
 ( #8352, #25446, #12573, #23258, #18890, #3301, #8085, #27772, #21077, #10386, #1138, #25724, #5755, #23538, #9975, #27907, #25588, #5615, #21486, #14496, #28185, #23397, #3439, #12304, #19022, #1544, #16835, #25864, #3575, #11089, #4426, #13297, #3992 ),
 .UNSPECIFIED., .F., .F.,
 ( 4, 2, 1, 1, 2, 2, 1, 1, 1, 2, 2, 2, 1, 1, 2, 2, 1, 1, 2, 2, 4 ),
 ( 0.000000000000000000, 0.06249999999986458055, 0.09374999999978507470, 0.1093749999997540440, 0.1171874999997460920, 0.1249999999997381261, 0.1874999999997520594, 0.2187499999997566669, 0.2343749999997590261, 0.2421874999997645772, 0.2499999999997701283, 0.3749999999998100964, 0.4374999999998272493, 0.4687499999998345768, 0.4843749999998410716, 0.4999999999998475664, 0.6249999999998780975, 0.6874999999998955280, 0.7187499999999057421, 0.7499999999999159561, 1.000000000000000000 ),
 .UNSPECIFIED. ) ;
#1360 = DIRECTION ( 'NONE',  ( 0.000000000000000000, -1.000000000000000000, 0.000000000000000000 ) ) ;
#1361 = CARTESIAN_POINT ( 'NONE',  ( 25.88476489150000148, -71.55793241529998738, 11.20710331009999905 ) ) ;
#1362 = CARTESIAN_POINT ( 'NONE',  ( 0.3059185938709999553, -93.00000000000000000, 14.72672055670000013 ) ) ;
#1363 = ORIENTED_EDGE ( 'NONE', *, *, #7055, .F. ) ;
#1364 = CARTESIAN_POINT ( 'NONE',  ( 20.47461295229999934, -19.46889316100000045, -8.153555280290001761 ) ) ;
#1365 = ADVANCED_FACE ( 'NONE', ( #10434 ), #14955, .T. ) ;
#1366 = CARTESIAN_POINT ( 'NONE',  ( 11.50679452860000040, -101.1848541609999899, -10.05659687459999851 ) ) ;
#1367 = CARTESIAN_POINT ( 'NONE',  ( -14.65665286289999969, -74.43375220249998847, 36.94583910070000599 ) ) ;
#1368 = CARTESIAN_POINT ( 'NONE',  ( 46.25000000000000000, -74.00000000000000000, -9.166287847479999584 ) ) ;
#1369 = CARTESIAN_POINT ( 'NONE',  ( -31.00000000000000000, 0.000000000000000000, -4.500000000000000000 ) ) ;
#1370 = EDGE_LOOP ( 'NONE', ( #24888, #4484, #6016, #12627, #6708, #11813, #11488, #135, #2101, #11875, #891, #8626, #18680, #12669, #5294, #11926 ) ) ;
#1371 = EDGE_CURVE ( 'NONE', #24292, #7086, #7735, .T. ) ;
#1372 = DIRECTION ( 'NONE',  ( 0.000000000000000000, -1.000000000000000000, 0.000000000000000000 ) ) ;
#1373 = AXIS2_PLACEMENT_3D ( 'NONE', #19047, #27930, #7968 ) ;
#1374 = CARTESIAN_POINT ( 'NONE',  ( 0.002146109654809999837, -101.6311724339999927, -16.01369408300000075 ) ) ;
#1375 = CARTESIAN_POINT ( 'NONE',  ( 7.452486935440000515, -63.63835192340000191, -23.33420648839999956 ) ) ;
#1376 = CARTESIAN_POINT ( 'NONE',  ( -39.69297836749999675, -73.74954830059999722, -7.260231713199999604 ) ) ;
#1377 = EDGE_CURVE ( 'NONE', #2012, #20039, #5529, .T. ) ;
#1378 = FACE_OUTER_BOUND ( 'NONE', #27136, .T. ) ;
#1379 = CARTESIAN_POINT ( 'NONE',  ( 40.65508461000000295, -75.00000000000000000, -13.75000000000000000 ) ) ;
#1380 = ORIENTED_EDGE ( 'NONE', *, *, #26895, .T. ) ;
#1381 = EDGE_CURVE ( 'NONE', #22328, #8830, #3355, .T. ) ;
#1382 = CIRCLE ( 'NONE', #17641, 5.000000000000000888 ) ;
#1383 = TOROIDAL_SURFACE ( 'NONE', #5566, 14.25000000000000000, 2.000000000000000000 ) ;
#1384 = CARTESIAN_POINT ( 'NONE',  ( 6.719470054089999422, -100.4650220110000021, 15.43601254670000067 ) ) ;
#1385 = CARTESIAN_POINT ( 'NONE',  ( 15.64536997099999915, -101.3878691800000098, 3.811131059900000118 ) ) ;
#1386 = AXIS2_PLACEMENT_3D ( 'NONE', #5883, #3432, #1535 ) ;
#1387 = CARTESIAN_POINT ( 'NONE',  ( -11.63405728910000114, -94.86303146849999735, -21.38493624129999660 ) ) ;
#1388 = DIRECTION ( 'NONE',  ( 1.000000000000000000, 0.000000000000000000, 0.000000000000000000 ) ) ;
#1389 = CARTESIAN_POINT ( 'NONE',  ( 5.376469156563769225, -92.59033770611050329, -30.02271131604222987 ) ) ;
#1390 = CARTESIAN_POINT ( 'NONE',  ( -8.209474437350001708, -99.53431242750001218, 15.35746870819999899 ) ) ;
#1391 = CARTESIAN_POINT ( 'NONE',  ( 8.067175576580000396, -93.91547326120000605, -23.40448531159999845 ) ) ;
#1392 =( LENGTH_UNIT ( ) NAMED_UNIT ( * ) SI_UNIT ( .MILLI., .METRE. ) );
#1393 = ORIENTED_EDGE ( 'NONE', *, *, #27899, .F. ) ;
#1394 = AXIS2_PLACEMENT_3D ( 'NONE', #27280, #26988, #18533 ) ;
#1395 = DIRECTION ( 'NONE',  ( 0.000000000000000000, 1.000000000000000000, 0.000000000000000000 ) ) ;
#1396 = CARTESIAN_POINT ( 'NONE',  ( 6.114061450880000415, -111.0000000000000000, -13.40104985119999981 ) ) ;
#1397 = ORIENTED_EDGE ( 'NONE', *, *, #8218, .F. ) ;
#1398 = DIRECTION ( 'NONE',  ( 0.000000000000000000, -1.000000000000000000, 0.000000000000000000 ) ) ;
#1399 = ORIENTED_EDGE ( 'NONE', *, *, #11498, .F. ) ;
#1400 = AXIS2_PLACEMENT_3D ( 'NONE', #15830, #25329, #20664 ) ;
#1401 = CIRCLE ( 'NONE', #5114, 61.35000000000000142 ) ;
#1402 = CARTESIAN_POINT ( 'NONE',  ( 0.3445358076898260014, -101.3846248973681838, -16.20041589813614280 ) ) ;
#1403 = CARTESIAN_POINT ( 'NONE',  ( 6.018657797749999538, -100.4792519539999915, 15.03391506150000012 ) ) ;
#1404 = CARTESIAN_POINT ( 'NONE',  ( 41.00000000000000000, -74.00000000000000000, 10.20110288159999890 ) ) ;
#1405 = CARTESIAN_POINT ( 'NONE',  ( 25.07614445930000002, -74.11216212930001745, -30.15806252000000143 ) ) ;
#1406 = EDGE_CURVE ( 'NONE', #18883, #9768, #15708, .T. ) ;
#1407 = CARTESIAN_POINT ( 'NONE',  ( -22.88338618799999935, -72.19388347460001398, 16.81479657839999931 ) ) ;
#1408 = DIRECTION ( 'NONE',  ( 0.8775825618903718706, 0.000000000000000000, 0.4794255386042046152 ) ) ;
#1409 = DIRECTION ( 'NONE',  ( 0.000000000000000000, 1.000000000000000000, 0.000000000000000000 ) ) ;
#1410 = CARTESIAN_POINT ( 'NONE',  ( 24.33297166435627190, -93.99439547207676071, -9.447863160898569035 ) ) ;
#1411 = CARTESIAN_POINT ( 'NONE',  ( -13.49020432579999884, -18.50000000000000000, 18.73880173299999896 ) ) ;
#1412 = EDGE_LOOP ( 'NONE', ( #2757, #20982, #9366, #23861 ) ) ;
#1413 = EDGE_CURVE ( 'NONE', #19124, #14119, #21633, .T. ) ;
#1414 = CARTESIAN_POINT ( 'NONE',  ( 9.463625755926194927, -35.99991740498153092, -20.02750111241616437 ) ) ;
#1415 = ORIENTED_EDGE ( 'NONE', *, *, #25728, .T. ) ;
#1416 = VECTOR ( 'NONE', #19385, 1000.000000000000000 ) ;
#1417 = STYLED_ITEM ( 'NONE', ( #26599 ), #15528 ) ;
#1418 = CARTESIAN_POINT ( 'NONE',  ( -1.172419020520000021, -61.85641277710000452, -23.98846277950000072 ) ) ;
#1419 = CARTESIAN_POINT ( 'NONE',  ( 9.497542575549999810, -37.06806481049999746, -22.65555190710000133 ) ) ;
#1420 = DIRECTION ( 'NONE',  ( 0.09756097560976760563, 0.000000000000000000, 0.9952295494196654602 ) ) ;
#1421 = CARTESIAN_POINT ( 'NONE',  ( 20.52569424150000188, -35.38531346950000511, -8.770435587459999738 ) ) ;
#1422 = ORIENTED_EDGE ( 'NONE', *, *, #9345, .F. ) ;
#1423 = CARTESIAN_POINT ( 'NONE',  ( 21.51138255720000103, -35.67530038919999669, -6.929578944110000194 ) ) ;
#1424 = ORIENTED_EDGE ( 'NONE', *, *, #18031, .F. ) ;
#1425 = CARTESIAN_POINT ( 'NONE',  ( 25.26718046270000073, -19.50000000000000000, 6.129403842640000377 ) ) ;
#1426 = CARTESIAN_POINT ( 'NONE',  ( 9.061401562000000354, -35.89920192559999634, -20.19233861389999873 ) ) ;
#1427 = CARTESIAN_POINT ( 'NONE',  ( -4.459621975350000156, -72.00000000000000000, -28.73485931899999812 ) ) ;
#1428 = EDGE_CURVE ( 'NONE', #22101, #2397, #23522, .T. ) ;
#1429 =( REPRESENTATION_RELATIONSHIP ('NONE','NONE', #26008, #24690 ) REPRESENTATION_RELATIONSHIP_WITH_TRANSFORMATION ( #22737 )SHAPE_REPRESENTATION_RELATIONSHIP( ) );
#1430 = AXIS2_PLACEMENT_3D ( 'NONE', #3345, #20696, #14129 ) ;
#1431 = CARTESIAN_POINT ( 'NONE',  ( -22.19637807654410366, -74.23987217703098906, -32.69975610228092933 ) ) ;
#1432 = AXIS2_PLACEMENT_3D ( 'NONE', #23804, #12705, #1805 ) ;
#1433 = CARTESIAN_POINT ( 'NONE',  ( -22.25450259269999975, -94.89197151650000706, -8.089821617090001027 ) ) ;
#1434 = ADVANCED_FACE ( 'NONE', ( #8401 ), #24419, .F. ) ;
#1435 = CIRCLE ( 'NONE', #21428, 1.000000000000000888 ) ;
#1436 = DIRECTION ( 'NONE',  ( 0.000000000000000000, 1.000000000000000000, 0.000000000000000000 ) ) ;
#1437 = CARTESIAN_POINT ( 'NONE',  ( 0.000000000000000000, -107.1975888269999899, 0.000000000000000000 ) ) ;
#1438 = CARTESIAN_POINT ( 'NONE',  ( -14.34373124439999891, -92.50000000000000000, -26.25602392650000283 ) ) ;
#1439 = ORIENTED_EDGE ( 'NONE', *, *, #13143, .F. ) ;
#1440 = B_SPLINE_CURVE_WITH_KNOTS ( 'NONE', 3,
 ( #6733, #19970, #24055, #15598 ),
 .UNSPECIFIED., .F., .F.,
 ( 4, 4 ),
 ( -6.855861996829999860, 0.000000000000000000 ),
 .UNSPECIFIED. ) ;
#1441 = DIRECTION ( 'NONE',  ( 0.000000000000000000, 1.000000000000000000, 0.000000000000000000 ) ) ;
#1442 = CARTESIAN_POINT ( 'NONE',  ( -2.021043494270000185, -18.61827554290000108, -21.98709576639999952 ) ) ;
#1443 = CARTESIAN_POINT ( 'NONE',  ( -7.681814765061617756, -100.9570234913570488, 14.64644060644491574 ) ) ;
#1444 = ORIENTED_EDGE ( 'NONE', *, *, #27666, .F. ) ;
#1445 = ADVANCED_FACE ( 'NONE', ( #15233 ), #10997, .F. ) ;
#1446 = DIRECTION ( 'NONE',  ( 0.000000000000000000, 1.000000000000000000, 0.000000000000000000 ) ) ;
#1447 = DIRECTION ( 'NONE',  ( -0.7071067811865475727, 0.000000000000000000, 0.7071067811865475727 ) ) ;
#1448 = CARTESIAN_POINT ( 'NONE',  ( 36.93448770119999836, -79.95108530920001044, -14.10799736659999937 ) ) ;
#1449 = ORIENTED_EDGE ( 'NONE', *, *, #5830, .T. ) ;
#1450 = CARTESIAN_POINT ( 'NONE',  ( 6.659152648053978218, -101.1248211537192958, 14.99462091354799220 ) ) ;
#1451 = CIRCLE ( 'NONE', #4700, 0.4999999999999981126 ) ;
#1452 = CARTESIAN_POINT ( 'NONE',  ( -2.671186077582594631, -80.39081555798996703, 46.73997660184883784 ) ) ;
#1453 = AXIS2_PLACEMENT_3D ( 'NONE', #10854, #6519, #15376 ) ;
#1454 = ORIENTED_EDGE ( 'NONE', *, *, #12507, .T. ) ;
#1455 = AXIS2_PLACEMENT_3D ( 'NONE', #12126, #21042, #8048 ) ;
#1456 = CARTESIAN_POINT ( 'NONE',  ( 31.00000000000000000, -11.00000000000000000, 1.953992523340000041E-14 ) ) ;
#1457 = ORIENTED_EDGE ( 'NONE', *, *, #19024, .T. ) ;
#1458 = CARTESIAN_POINT ( 'NONE',  ( 27.17390343950000187, -92.54807936089999032, 9.505859965289999991 ) ) ;
#1459 = CARTESIAN_POINT ( 'NONE',  ( -38.31827398130649698, -63.05366291735832363, 2.839252009381883823 ) ) ;
#1460 = FACE_OUTER_BOUND ( 'NONE', #5969, .T. ) ;
#1461 = ORIENTED_EDGE ( 'NONE', *, *, #16424, .F. ) ;
#1462 = CARTESIAN_POINT ( 'NONE',  ( -3.292855076097166656, -97.38870237746982639, -20.36241341912896985 ) ) ;
#1463 = CARTESIAN_POINT ( 'NONE',  ( 0.000000000000000000, -65.07443093669999712, 0.000000000000000000 ) ) ;
#1464 = CARTESIAN_POINT ( 'NONE',  ( -40.50000000000000000, -63.00000000000000000, -2.309401076760000393 ) ) ;
#1465 = CARTESIAN_POINT ( 'NONE',  ( 9.885503724449998586, -36.00000000000000000, -20.33566493500000050 ) ) ;
#1466 = CARTESIAN_POINT ( 'NONE',  ( 16.83483077069999823, -99.92967571559999840, 4.239603657359999112 ) ) ;
#1467 = CARTESIAN_POINT ( 'NONE',  ( -3.807886452449999570, -80.00000000000000000, 46.75000000000000000 ) ) ;
#1468 = EDGE_LOOP ( 'NONE', ( #2304, #3722, #15574, #8835 ) ) ;
#1469 = DIRECTION ( 'NONE',  ( 0.000000000000000000, 1.000000000000000000, 0.000000000000000000 ) ) ;
#1470 = EDGE_CURVE ( 'NONE', #1149, #13839, #11901, .T. ) ;
#1471 = CARTESIAN_POINT ( 'NONE',  ( 15.83524192907358596, -101.5839620086842956, 2.606923154417748467 ) ) ;
#1472 = CARTESIAN_POINT ( 'NONE',  ( -20.27478635940000373, -94.70873263889998839, 12.26043739520000031 ) ) ;
#1473 = CARTESIAN_POINT ( 'NONE',  ( 23.55422583189999841, -93.65023553250000532, -9.043238345449999827 ) ) ;
#1474 = CARTESIAN_POINT ( 'NONE',  ( -0.8459307125330000066, -55.05548131569999981, -23.26322409530000002 ) ) ;
#1475 = AXIS2_PLACEMENT_3D ( 'NONE', #5724, #19825, #15149 ) ;
#1476 = CARTESIAN_POINT ( 'NONE',  ( -1.501869189730000054, -79.88809860310000488, 47.16627303149999761 ) ) ;
#1477 = CARTESIAN_POINT ( 'NONE',  ( -2.578307999469999778, -52.56313962710000709, -25.11373953509999879 ) ) ;
#1478 = VERTEX_POINT ( 'NONE', #27890 ) ;
#1479 = AXIS2_PLACEMENT_3D ( 'NONE', #19800, #8292, #21709 ) ;
#1480 = CARTESIAN_POINT ( 'NONE',  ( -15.21246488650000117, -100.9405327639999967, 4.776672761669999545 ) ) ;
#1481 = CIRCLE ( 'NONE', #21469, 0.4999999999999985567 ) ;
#1482 = CARTESIAN_POINT ( 'NONE',  ( 20.52749306944123830, -97.43022994675339987, 1.376655802589148880 ) ) ;
#1483 = CARTESIAN_POINT ( 'NONE',  ( 28.89564796280000181, -73.80968813319999811, -26.61317346570000097 ) ) ;
#1484 = CARTESIAN_POINT ( 'NONE',  ( -15.78701020529999965, -72.82938648530000592, 23.94860758700000147 ) ) ;
#1485 = FACE_OUTER_BOUND ( 'NONE', #1288, .T. ) ;
#1486 = B_SPLINE_SURFACE_WITH_KNOTS ( 'NONE', 5, 5, ( 
 ( #7989, #6067, #28222, #14410, #12758, #5658 ),
 ( #10149, #16596, #21390, #5799, #23854, #14682 ),
 ( #3895, #21669, #23574, #12620, #16882, #1719 ),
 ( #23299, #10559, #14539, #5522, #19070, #12211 ),
 ( #5927, #21122, #1179, #8126, #3617, #12476 ),
 ( #19345, #1448, #23447, #17016, #10018, #21531 ),
 ( #1306, #18932, #14811, #7853, #16736, #23713 ),
 ( #3756, #17151, #25629, #28787, #10850, #28506 ),
 ( #28362, #23996, #8393, #24142, #1865, #2011 ) ),
 .UNSPECIFIED., .F., .F., .F.,
 ( 6, 3, 6 ),
 ( 6, 6 ),
 ( 4.463004670310000144, 6.097538245950000046, 7.424416524390000660 ),
 ( 0.000000000000000000, 0.5000000000000000000 ),
 .UNSPECIFIED. ) ;
#1487 = SHAPE_REPRESENTATION_RELATIONSHIP ( 'NONE' , 'NONE' ,  #10908, #15419 ) ;
#1488 = VERTEX_POINT ( 'NONE', #20921 ) ;
#1489 = EDGE_CURVE ( 'NONE', #21683, #25610, #7372, .T. ) ;
#1490 = CARTESIAN_POINT ( 'NONE',  ( 21.47791254800000260, -36.56811099849999636, -7.356933688149999817 ) ) ;
#1491 = ORIENTED_EDGE ( 'NONE', *, *, #7558, .T. ) ;
#1492 = ADVANCED_FACE ( 'NONE', ( #12008 ), #27763, .T. ) ;
#1493 = CARTESIAN_POINT ( 'NONE',  ( 21.47791242350000118, -36.56811125149999953, -7.356933663620000452 ) ) ;
#1494 = CARTESIAN_POINT ( 'NONE',  ( 0.000000000000000000, -40.00000000000000000, 60.85000000000000142 ) ) ;
#1495 = ORIENTED_EDGE ( 'NONE', *, *, #6337, .T. ) ;
#1496 = CARTESIAN_POINT ( 'NONE',  ( -12.54641657280000011, -101.1292389600000092, -9.112281375189999366 ) ) ;
#1497 = CONICAL_SURFACE ( 'NONE', #22909, 57.74999999999999289, 1.152571997220000144 ) ;
#1498 = CARTESIAN_POINT ( 'NONE',  ( -7.903212057390000211, -99.83167681540000160, 15.42228797350000136 ) ) ;
#1499 = ORIENTED_EDGE ( 'NONE', *, *, #10277, .F. ) ;
#1500 = CARTESIAN_POINT ( 'NONE',  ( -2.986711171310000079, -94.79581646409999962, 23.48470800579999818 ) ) ;
#1501 = B_SPLINE_CURVE_WITH_KNOTS ( 'NONE', 3,
 ( #14967, #8273, #19495, #21410, #23733, #3777, #2029, #1467 ),
 .UNSPECIFIED., .F., .F.,
 ( 4, 2, 2, 4 ),
 ( 0.000000000000000000, 0.4999999999999997780, 0.7499999999999998890, 1.000000000000000000 ),
 .UNSPECIFIED. ) ;
#1502 = CARTESIAN_POINT ( 'NONE',  ( 9.486381418089997908, -49.04525650320000807, -23.29174250550000025 ) ) ;
#1503 = DIRECTION ( 'NONE',  ( 0.000000000000000000, -1.000000000000000000, 0.000000000000000000 ) ) ;
#1504 = ORIENTED_EDGE ( 'NONE', *, *, #6819, .F. ) ;
#1505 = CARTESIAN_POINT ( 'NONE',  ( 12.88080974073147189, -101.3846248973631958, -9.831425157082634314 ) ) ;
#1506 = PLANE ( 'NONE',  #14915 ) ;
#1507 = CARTESIAN_POINT ( 'NONE',  ( -16.91430575710000284, -100.0771588430000065, 3.341621066080000091 ) ) ;
#1508 = ORIENTED_EDGE ( 'NONE', *, *, #11910, .T. ) ;
#1509 = CARTESIAN_POINT ( 'NONE',  ( 20.14564099000000041, -18.61853073029999805, -7.938153854090000294 ) ) ;
#1510 = CARTESIAN_POINT ( 'NONE',  ( -14.76202981470000175, -74.22231530550000400, 36.28478801819999688 ) ) ;
#1511 = CARTESIAN_POINT ( 'NONE',  ( -41.48055058678063034, -63.07121106306871638, -2.875522221980898241 ) ) ;
#1512 = DIRECTION ( 'NONE',  ( 0.000000000000000000, 1.000000000000000000, 0.000000000000000000 ) ) ;
#1513 = ORIENTED_EDGE ( 'NONE', *, *, #4915, .T. ) ;
#1514 = CYLINDRICAL_SURFACE ( 'NONE', #7223, 18.64285714290000229 ) ;
#1515 = CARTESIAN_POINT ( 'NONE',  ( 7.150868990479999354, -60.60240929710000302, -22.51513940059999896 ) ) ;
#1516 = CARTESIAN_POINT ( 'NONE',  ( 7.627566167509999495, -74.00000000000000000, -38.62788938250000115 ) ) ;
#1517 = CARTESIAN_POINT ( 'NONE',  ( 20.85556312030000115, -57.91337896769999816, 10.70610008499999921 ) ) ;
#1518 = PLANE ( 'NONE',  #7141 ) ;
#1519 = VECTOR ( 'NONE', #12148, 1000.000000000000000 ) ;
#1520 = ORIENTED_EDGE ( 'NONE', *, *, #196, .T. ) ;
#1521 = CARTESIAN_POINT ( 'NONE',  ( 6.649881675840000561, -101.0405520670000072, 14.82396520390000028 ) ) ;
#1522 = CARTESIAN_POINT ( 'NONE',  ( 15.60420274139999997, -101.2927714249999980, 3.777748170229999758 ) ) ;
#1523 = EDGE_CURVE ( 'NONE', #10585, #11090, #26766, .T. ) ;
#1524 = CARTESIAN_POINT ( 'NONE',  ( -40.50000000000000000, -65.63577453799999262, -2.309401076760000393 ) ) ;
#1525 = CARTESIAN_POINT ( 'NONE',  ( 3.787197165510000296, -93.00000000000000000, -30.26395773239999798 ) ) ;
#1526 = CARTESIAN_POINT ( 'NONE',  ( 3.355978770230000130, -90.50000000000000000, 6.143077933229999843 ) ) ;
#1527 = CARTESIAN_POINT ( 'NONE',  ( 34.89999999999999858, -84.50000000000000000, 4.273876174839999917E-15 ) ) ;
#1528 = CARTESIAN_POINT ( 'NONE',  ( 3.263855493430000365, -92.57423544259999915, -28.67967719789999848 ) ) ;
#1529 = EDGE_CURVE ( 'NONE', #23252, #17228, #8426, .T. ) ;
#1530 = CARTESIAN_POINT ( 'NONE',  ( -7.196178079599999222, -73.81415926540000783, -38.70548889989999708 ) ) ;
#1531 = CARTESIAN_POINT ( 'NONE',  ( -1.869200974745226063, -93.63284908718598842, 25.01357699951009295 ) ) ;
#1532 = ORIENTED_EDGE ( 'NONE', *, *, #17302, .F. ) ;
#1533 = CIRCLE ( 'NONE', #3842, 18.64285714289999873 ) ;
#1534 = DIRECTION ( 'NONE',  ( 1.000000000000000000, 0.000000000000000000, 0.000000000000000000 ) ) ;
#1535 = DIRECTION ( 'NONE',  ( 0.4794255386042040601, 0.000000000000000000, 0.8775825618903720926 ) ) ;
#1536 = EDGE_LOOP ( 'NONE', ( #13375, #8343, #24939, #21800 ) ) ;
#1537 = EDGE_CURVE ( 'NONE', #23472, #19113, #3292, .T. ) ;
#1538 = CONICAL_SURFACE ( 'NONE', #624, 25.14975229270001833, 0.4276056667390000787 ) ;
#1539 = ADVANCED_FACE ( 'NONE', ( #21064 ), #9057, .T. ) ;
#1540 = ORIENTED_EDGE ( 'NONE', *, *, #12604, .F. ) ;
#1541 = CARTESIAN_POINT ( 'NONE',  ( -0.7205257404120000153, -101.5369810359999860, -15.98376809940000065 ) ) ;
#1542 = CARTESIAN_POINT ( 'NONE',  ( -11.25859204269364078, -19.46519122827088566, 19.08718618545535861 ) ) ;
#1543 = CARTESIAN_POINT ( 'NONE',  ( -43.23056608648008137, -63.07120704560069413, 0.1555577424909893314 ) ) ;
#1544 = CARTESIAN_POINT ( 'NONE',  ( 13.83675081990681122, -92.54938211476543586, 27.18091423687219788 ) ) ;
#1545 = CARTESIAN_POINT ( 'NONE',  ( 27.75394116159999669, -74.50000000000000000, -27.75394116159999669 ) ) ;
#1546 = CARTESIAN_POINT ( 'NONE',  ( -22.41375146320000056, -69.63326797740000984, 15.46718870090000131 ) ) ;
#1547 = PRODUCT_DEFINITION_SHAPE ( 'NONE', 'NONE',  #28806 ) ;
#1548 = VECTOR ( 'NONE', #13237, 1000.000000000000000 ) ;
#1549 = DIRECTION ( 'NONE',  ( 0.000000000000000000, 0.000000000000000000, -1.000000000000000000 ) ) ;
#1550 = DIRECTION ( 'NONE',  ( 1.000000000000000000, 0.000000000000000000, 0.000000000000000000 ) ) ;
#1551 = CARTESIAN_POINT ( 'NONE',  ( 7.044629870050000520, -36.15937179259999823, -21.49951968199999897 ) ) ;
#1552 = CARTESIAN_POINT ( 'NONE',  ( 14.28941763439999946, -93.00000000000000000, -3.575252188409999921 ) ) ;
#1553 = ORIENTED_EDGE ( 'NONE', *, *, #13410, .T. ) ;
#1554 = DIRECTION ( 'NONE',  ( -0.9952295494196655712, 0.000000000000000000, -0.09756097560976655092 ) ) ;
#1555 = CIRCLE ( 'NONE', #27139, 15.19391340349999986 ) ;
#1556 = ORIENTED_EDGE ( 'NONE', *, *, #10088, .F. ) ;
#1557 = AXIS2_PLACEMENT_3D ( 'NONE', #12996, #1958, #1287 ) ;
#1558 = ORIENTED_EDGE ( 'NONE', *, *, #9808, .F. ) ;
#1559 = CARTESIAN_POINT ( 'NONE',  ( 26.69293917519999937, -22.69689110870000093, 48.86109741659999628 ) ) ;
#1560 = CARTESIAN_POINT ( 'NONE',  ( 10.41102187780000143, -36.06096454729999579, -21.78369632219999730 ) ) ;
#1561 = DIRECTION ( 'NONE',  ( 0.000000000000000000, -1.000000000000000000, 0.000000000000000000 ) ) ;
#1562 = DIRECTION ( 'NONE',  ( 0.000000000000000000, -1.000000000000000000, 0.000000000000000000 ) ) ;
#1563 = DIRECTION ( 'NONE',  ( 0.000000000000000000, -1.000000000000000000, 0.000000000000000000 ) ) ;
#1564 = ADVANCED_FACE ( 'NONE', ( #16388 ), #3011, .T. ) ;
#1565 = CARTESIAN_POINT ( 'NONE',  ( 15.35943464070000175, -100.7833805400000102, 4.159771655669999291 ) ) ;
#1566 = ORIENTED_EDGE ( 'NONE', *, *, #11570, .T. ) ;
#1567 = CIRCLE ( 'NONE', #15021, 60.66666666670000296 ) ;
#1568 = CARTESIAN_POINT ( 'NONE',  ( 21.31951852150000093, -34.95415007660000128, -7.429758059829999262 ) ) ;
#1569 = VERTEX_POINT ( 'NONE', #9962 ) ;
#1570 = CARTESIAN_POINT ( 'NONE',  ( 11.31764174110000098, -38.00000000000000000, -22.43277175240000076 ) ) ;
#1571 = EDGE_CURVE ( 'NONE', #1349, #23532, #266, .T. ) ;
#1572 = B_SPLINE_CURVE_WITH_KNOTS ( 'NONE', 3,
 ( #2936, #15721, #4666, #5811, #27560, #14690 ),
 .UNSPECIFIED., .F., .F.,
 ( 4, 2, 4 ),
 ( 0.000000000000000000, 0.5000000000000000000, 1.000000000000000000 ),
 .UNSPECIFIED. ) ;
#1573 = AXIS2_PLACEMENT_3D ( 'NONE', #13511, #6979, #438 ) ;
#1574 = CARTESIAN_POINT ( 'NONE',  ( -22.13204528394974346, -74.08924643999768023, -32.43483521824870053 ) ) ;
#1575 = CARTESIAN_POINT ( 'NONE',  ( 21.85035090750000109, -18.50000000000000000, 8.503095831829998730 ) ) ;
#1576 = CARTESIAN_POINT ( 'NONE',  ( -32.64229262974771473, -74.19321449783478784, -22.18246179812063090 ) ) ;
#1577 = CARTESIAN_POINT ( 'NONE',  ( -20.58900368409999970, -58.81362829640000456, 14.87320149399999991 ) ) ;
#1578 = ORIENTED_EDGE ( 'NONE', *, *, #18993, .T. ) ;
#1579 = CARTESIAN_POINT ( 'NONE',  ( 22.83659466689194062, -95.90275867365805595, -4.923095664741855337 ) ) ;
#1580 = CARTESIAN_POINT ( 'NONE',  ( -11.69640386740000082, -101.0875971110000080, -10.03173011250000002 ) ) ;
#1581 = CARTESIAN_POINT ( 'NONE',  ( -0.5753802177429999665, -18.61794786970000359, -21.64101937650000096 ) ) ;
#1582 = CARTESIAN_POINT ( 'NONE',  ( -7.501065465934297016, -101.2145573445136222, 14.51273970916295752 ) ) ;
#1583 = ORIENTED_EDGE ( 'NONE', *, *, #25734, .F. ) ;
#1584 = AXIS2_PLACEMENT_3D ( 'NONE', #14440, #21562, #16910 ) ;
#1585 = TOROIDAL_SURFACE ( 'NONE', #2055, 21.03431122519999974, 1.000000000000000000 ) ;
#1586 = CARTESIAN_POINT ( 'NONE',  ( 10.34250236315985028, -65.75540811119959983, -25.31863394739911399 ) ) ;
#1587 = CARTESIAN_POINT ( 'NONE',  ( -5.329070518200000398E-15, -19.46510050329999686, 0.000000000000000000 ) ) ;
#1588 = VERTEX_POINT ( 'NONE', #25714 ) ;
#1589 = ADVANCED_FACE ( 'NONE', ( #13916 ), #28211, .T. ) ;
#1590 = AXIS2_PLACEMENT_3D ( 'NONE', #2444, #11741, #28782 ) ;
#1591 = ORIENTED_EDGE ( 'NONE', *, *, #15954, .F. ) ;
#1592 = EDGE_CURVE ( 'NONE', #16528, #28629, #10836, .T. ) ;
#1593 = DIRECTION ( 'NONE',  ( 0.000000000000000000, 1.000000000000000000, 0.000000000000000000 ) ) ;
#1594 = CARTESIAN_POINT ( 'NONE',  ( 47.25009368219999573, -74.76204734789999407, -0.5461026333709999570 ) ) ;
#1595 = EDGE_LOOP ( 'NONE', ( #10372, #9875, #25781, #7720 ) ) ;
#1596 = CARTESIAN_POINT ( 'NONE',  ( 21.08559791560000107, -57.47122622300000216, 10.49905601410000067 ) ) ;
#1597 = DIRECTION ( 'NONE',  ( 0.000000000000000000, -1.000000000000000000, 0.000000000000000000 ) ) ;
#1598 = CARTESIAN_POINT ( 'NONE',  ( 1.421085471519999843E-14, -69.00000000000000000, 46.75000000000000000 ) ) ;
#1599 = EDGE_LOOP ( 'NONE', ( #20525, #22685, #3053, #14488 ) ) ;
#1600 = CARTESIAN_POINT ( 'NONE',  ( -41.80254054884269976, -63.35496709430440632, 1.228761571272451780 ) ) ;
#1601 = CARTESIAN_POINT ( 'NONE',  ( 41.00000000000000000, -84.00000000000000000, -10.20110288159999890 ) ) ;
#1602 = EDGE_CURVE ( 'NONE', #4968, #212, #2098, .T. ) ;
#1603 = CONICAL_SURFACE ( 'NONE', #17400, 5.499999999999999112, 0.3217505543970000104 ) ;
#1604 = CARTESIAN_POINT ( 'NONE',  ( -22.43272078519999724, -80.50000000000000000, -32.20769377289999369 ) ) ;
#1605 = CARTESIAN_POINT ( 'NONE',  ( -14.15498507100000047, -93.99830544900000007, -21.64661225829999935 ) ) ;
#1606 = CARTESIAN_POINT ( 'NONE',  ( -0.5590517731190000061, -18.50000000000000000, -21.02688049580000040 ) ) ;
#1607 = ORIENTED_EDGE ( 'NONE', *, *, #22080, .T. ) ;
#1608 = CARTESIAN_POINT ( 'NONE',  ( -18.71306389469999942, -96.65227117089999354, -10.09692839740000103 ) ) ;
#1609 = CARTESIAN_POINT ( 'NONE',  ( 13.51933813770000015, -100.3517545579999961, -9.891026358559999565 ) ) ;
#1610 = CARTESIAN_POINT ( 'NONE',  ( -27.68682485439999752, -32.30000000000000426, -50.68039294919999804 ) ) ;
#1611 = CARTESIAN_POINT ( 'NONE',  ( 23.80455697029999840, -93.92589062420000801, -8.153550017880000667 ) ) ;
#1612 = VERTEX_POINT ( 'NONE', #20289 ) ;
#1613 = VECTOR ( 'NONE', #24837, 1000.000000000000000 ) ;
#1614 = CARTESIAN_POINT ( 'NONE',  ( 10.81555269790697871, -72.52478263476059794, -26.82924833248659624 ) ) ;
#1615 = CARTESIAN_POINT ( 'NONE',  ( -19.73459502929999587, -19.18584080579999807, 14.41863472910000077 ) ) ;
#1616 = VERTEX_POINT ( 'NONE', #15913 ) ;
#1617 = DIRECTION ( 'NONE',  ( 0.3687499999999814260, 0.000000000000000000, -0.9295286103719527793 ) ) ;
#1618 = AXIS2_PLACEMENT_3D ( 'NONE', #8826, #2740, #575 ) ;
#1619 = CARTESIAN_POINT ( 'NONE',  ( -18.87406717280000024, -19.42987840520000020, 13.82478526419999909 ) ) ;
#1620 = CARTESIAN_POINT ( 'NONE',  ( 20.65093475452214022, -97.34036579196893513, 1.255409981387750173 ) ) ;
#1621 = CARTESIAN_POINT ( 'NONE',  ( 0.000000000000000000, -33.49689110869999809, 0.000000000000000000 ) ) ;
#1622 = CARTESIAN_POINT ( 'NONE',  ( 27.75394116159999669, -74.50000000000000000, -27.75394116159999669 ) ) ;
#1623 = CARTESIAN_POINT ( 'NONE',  ( 29.11677867130000052, -92.50000000000000000, 6.880015861159999524 ) ) ;
#1624 = VECTOR ( 'NONE', #20003, 1000.000000000000114 ) ;
#1625 = ORIENTED_EDGE ( 'NONE', *, *, #14208, .T. ) ;
#1626 = ADVANCED_FACE ( 'NONE', ( #26713 ), #13285, .T. ) ;
#1627 = CARTESIAN_POINT ( 'NONE',  ( 36.24656994149999889, -82.25000000000000000, -15.05817610060000078 ) ) ;
#1628 = CARTESIAN_POINT ( 'NONE',  ( -38.08875739639999836, -74.50000000000000000, -9.476764215410000247 ) ) ;
#1629 = ORIENTED_EDGE ( 'NONE', *, *, #14978, .T. ) ;
#1630 = CARTESIAN_POINT ( 'NONE',  ( 21.54829813079999923, -37.62468161500000008, -7.859468734160000025 ) ) ;
#1631 = CARTESIAN_POINT ( 'NONE',  ( 9.323408666494477970, -35.97776767532982234, -19.72111573045538790 ) ) ;
#1632 = ORIENTED_EDGE ( 'NONE', *, *, #14850, .F. ) ;
#1633 = EDGE_CURVE ( 'NONE', #14431, #13203, #23844, .T. ) ;
#1634 = CARTESIAN_POINT ( 'NONE',  ( -13.23436873610000042, -101.5317765570000006, -9.147552046289998628 ) ) ;
#1635 = DIRECTION ( 'NONE',  ( 0.9863585068926603583, 0.000000000000000000, 0.1646113479699432003 ) ) ;
#1636 = B_SPLINE_CURVE_WITH_KNOTS ( 'NONE', 3,
 ( #8884, #8309, #22760, #7311, #782, #9037, #11212, #5125, #4677, #486, #634, #336, #9482, #13406, #24493, #2356, #20724, #26984, #9179, #9624 ),
 .UNSPECIFIED., .F., .F.,
 ( 4, 2, 2, 1, 1, 1, 1, 1, 1, 2, 2, 2, 4 ),
 ( 0.000000000000000000, 0.2499999999997837841, 0.3749999999996731503, 0.4374999999996190270, 0.4687499999995919375, 0.4843749999995772271, 0.4921874999995687339, 0.4960937499995645705, 0.4980468749995613509, 0.4990234374995608513, 0.4999999999995603517, 0.7499999999997800648, 1.000000000000000000 ),
 .UNSPECIFIED. ) ;
#1637 = FACE_OUTER_BOUND ( 'NONE', #11830, .T. ) ;
#1638 = ORIENTED_EDGE ( 'NONE', *, *, #14608, .T. ) ;
#1639 = AXIS2_PLACEMENT_3D ( 'NONE', #14487, #7674, #5464 ) ;
#1640 = DIRECTION ( 'NONE',  ( 1.000000000000000000, 0.000000000000000000, 0.000000000000000000 ) ) ;
#1641 = CARTESIAN_POINT ( 'NONE',  ( 20.76917537309745043, -34.61672842233151215, -8.508194708340036883 ) ) ;
#1642 = CYLINDRICAL_SURFACE ( 'NONE', #4136, 20.64285714289999163 ) ;
#1643 = ORIENTED_EDGE ( 'NONE', *, *, #23439, .F. ) ;
#1644 = CARTESIAN_POINT ( 'NONE',  ( 12.60821841358252193, -101.5829753080987814, -9.932320047300365218 ) ) ;
#1645 = DIRECTION ( 'NONE',  ( 0.000000000000000000, 1.000000000000000000, 0.000000000000000000 ) ) ;
#1646 = CARTESIAN_POINT ( 'NONE',  ( 25.35362416179999911, -70.54208558190001099, 11.30155583190000002 ) ) ;
#1647 = CARTESIAN_POINT ( 'NONE',  ( 7.181689689069999716, -99.92967571559999840, 15.80535034289999885 ) ) ;
#1648 = ORIENTED_EDGE ( 'NONE', *, *, #18541, .T. ) ;
#1649 = CIRCLE ( 'NONE', #16987, 0.3500000000000003664 ) ;
#1650 = DIRECTION ( 'NONE',  ( 0.000000000000000000, 1.000000000000000000, 0.000000000000000000 ) ) ;
#1651 = CARTESIAN_POINT ( 'NONE',  ( -14.03661932880000052, -74.01263034700001242, 36.31171197689999985 ) ) ;
#1652 = LINE ( 'NONE', #10076, #25553 ) ;
#1653 = CARTESIAN_POINT ( 'NONE',  ( -20.59421057834115842, -93.07145594888166329, 16.81328959876951856 ) ) ;
#1654 = ORIENTED_EDGE ( 'NONE', *, *, #12704, .T. ) ;
#1655 = DIRECTION ( 'NONE',  ( -1.000000000000000000, 0.000000000000000000, 0.000000000000000000 ) ) ;
#1656 = EDGE_CURVE ( 'NONE', #15453, #19773, #6655, .T. ) ;
#1657 = CARTESIAN_POINT ( 'NONE',  ( 9.133379025440000021, -64.81170986960000846, -23.88371660259999985 ) ) ;
#1658 = CARTESIAN_POINT ( 'NONE',  ( 15.76644911200000188, -101.6484611580000035, 2.726874312449999671 ) ) ;
#1659 = CARTESIAN_POINT ( 'NONE',  ( 20.71609666450000020, -58.79428935229999098, 10.97841134070000102 ) ) ;
#1660 = CARTESIAN_POINT ( 'NONE',  ( -11.05584978989999989, -26.99662418170000322, -22.00022356550000069 ) ) ;
#1661 = ORIENTED_EDGE ( 'NONE', *, *, #15036, .F. ) ;
#1662 = CARTESIAN_POINT ( 'NONE',  ( 6.540410660740000104, -100.9364576079999978, 14.54829053200000111 ) ) ;
#1663 = CARTESIAN_POINT ( 'NONE',  ( -15.61689027843468480, -92.57936004669802799, -24.03289022899482674 ) ) ;
#1664 = ADVANCED_FACE ( 'NONE', ( #15461 ), #15415, .F. ) ;
#1665 = CARTESIAN_POINT ( 'NONE',  ( -39.95446396948431556, -65.74401273904912557, -2.175432824119099884 ) ) ;
#1666 = CARTESIAN_POINT ( 'NONE',  ( 21.76289735059999941, -18.50000000000000000, 1.487608604080000063 ) ) ;
#1667 = CARTESIAN_POINT ( 'NONE',  ( 5.326862811529999898E-15, -69.50000000000000000, -32.75000000000000000 ) ) ;
#1668 = EDGE_LOOP ( 'NONE', ( #8051, #17208, #12347, #594 ) ) ;
#1669 = CARTESIAN_POINT ( 'NONE',  ( 9.010434747179999704, -94.45168166339999516, -23.20781253819999890 ) ) ;
#1670 = CARTESIAN_POINT ( 'NONE',  ( 20.26062886849999956, -31.59895360039999801, -8.804563333769998223 ) ) ;
#1671 = CARTESIAN_POINT ( 'NONE',  ( 6.954809927569434613, -101.6297509123136535, 14.42559876608666514 ) ) ;
#1672 = CARTESIAN_POINT ( 'NONE',  ( 1.673548719218163061, -92.65509297688285528, 27.65323130849352395 ) ) ;
#1673 = ORIENTED_EDGE ( 'NONE', *, *, #12243, .T. ) ;
#1674 = CARTESIAN_POINT ( 'NONE',  ( 7.670973119660000172, -34.59820496239999699, -21.21808926809999818 ) ) ;
#1675 = CARTESIAN_POINT ( 'NONE',  ( -12.73945486129048454, -100.6338045024292995, -10.94379842081711551 ) ) ;
#1676 = ORIENTED_EDGE ( 'NONE', *, *, #12743, .T. ) ;
#1677 = CARTESIAN_POINT ( 'NONE',  ( -1.283022169079999886, -101.3150705500000157, -16.20107500659999644 ) ) ;
#1678 = DIRECTION ( 'NONE',  ( 1.000000000000000000, 0.000000000000000000, 0.000000000000000000 ) ) ;
#1679 = B_SPLINE_CURVE_WITH_KNOTS ( 'NONE', 5,
 ( #23387, #16240, #20639, #25153, #20785, #1128, #14068, #12155, #695 ),
 .UNSPECIFIED., .F., .F.,
 ( 6, 3, 6 ),
 ( 0.000000000000000000, 0.5000000000000000000, 1.000000000000000000 ),
 .UNSPECIFIED. ) ;
#1680 = DIRECTION ( 'NONE',  ( 1.000000000000000000, 0.000000000000000000, 0.000000000000000000 ) ) ;
#1681 = CARTESIAN_POINT ( 'NONE',  ( 16.15437062272748037, -94.72386903546126291, 17.24227625337255176 ) ) ;
#1682 = CARTESIAN_POINT ( 'NONE',  ( -22.52719173530000063, -71.34739024110000116, 17.13464880949999980 ) ) ;
#1683 = EDGE_CURVE ( 'NONE', #16368, #27297, #20268, .T. ) ;
#1684 = CARTESIAN_POINT ( 'NONE',  ( -15.39276618183619583, -101.4254873439999329, 4.250919977501043334 ) ) ;
#1685 = CARTESIAN_POINT ( 'NONE',  ( -12.89904887990000049, -65.07443093669999712, -21.58991473350000234 ) ) ;
#1686 = CARTESIAN_POINT ( 'NONE',  ( 7.248976484529999098, -36.19499434569999607, -21.47059228039999823 ) ) ;
#1687 = CIRCLE ( 'NONE', #21673, 4.999999999999997335 ) ;
#1688 = DIRECTION ( 'NONE',  ( 0.000000000000000000, 1.000000000000000000, 0.000000000000000000 ) ) ;
#1689 = EDGE_LOOP ( 'NONE', ( #7473, #20189, #20911 ) ) ;
#1690 = DIRECTION ( 'NONE',  ( 1.000000000000000000, 0.000000000000000000, 0.000000000000000000 ) ) ;
#1691 = VERTEX_POINT ( 'NONE', #20747 ) ;
#1692 = CARTESIAN_POINT ( 'NONE',  ( 21.46129390369999967, -36.00000000000000000, -10.95532196250000112 ) ) ;
#1693 = ADVANCED_FACE ( 'NONE', ( #13878 ), #7601, .F. ) ;
#1694 = ORIENTED_EDGE ( 'NONE', *, *, #22234, .F. ) ;
#1695 = CARTESIAN_POINT ( 'NONE',  ( 7.253824468913529167, -36.56890885699328209, -21.48302338317096272 ) ) ;
#1696 = CARTESIAN_POINT ( 'NONE',  ( -29.44685991679999759, -92.54628605920001405, 6.396492330759999234 ) ) ;
#1697 = CARTESIAN_POINT ( 'NONE',  ( 19.97576656849999921, -72.00000000000000000, -19.97576656849999921 ) ) ;
#1698 = CARTESIAN_POINT ( 'NONE',  ( -19.65068252670001669, -52.63280639840017017, 12.32128691209999971 ) ) ;
#1699 = CARTESIAN_POINT ( 'NONE',  ( -9.348798002780000616, -17.50000000000000000, -17.11285995690000306 ) ) ;
#1700 = VERTEX_POINT ( 'NONE', #25115 ) ;
#1701 = DIRECTION ( 'NONE',  ( 1.000000000000000000, 0.000000000000000000, 0.000000000000000000 ) ) ;
#1702 = DIRECTION ( 'NONE',  ( -0.9952295494196654602, 0.000000000000000000, 0.09756097560976770278 ) ) ;
#1703 = ORIENTED_EDGE ( 'NONE', *, *, #11122, .T. ) ;
#1704 = CARTESIAN_POINT ( 'NONE',  ( 0.000000000000000000, -11.79999999999999893, 0.000000000000000000 ) ) ;
#1705 = ORIENTED_EDGE ( 'NONE', *, *, #7502, .F. ) ;
#1706 = CARTESIAN_POINT ( 'NONE',  ( 39.48500436340665232, -74.13942000237629770, 7.435977657333745938 ) ) ;
#1707 = CARTESIAN_POINT ( 'NONE',  ( -15.29947873360000088, -101.1716782170000073, 3.671501766180000459 ) ) ;
#1708 = CARTESIAN_POINT ( 'NONE',  ( -22.00137621023848666, -95.57586223585661855, -5.105060933739808959 ) ) ;
#1709 = CARTESIAN_POINT ( 'NONE',  ( -19.68101754359999944, -59.01563984649999384, 13.03622722340000095 ) ) ;
#1710 = VERTEX_POINT ( 'NONE', #9929 ) ;
#1711 = DIRECTION ( 'NONE',  ( 1.000000000000000000, 0.000000000000000000, 0.000000000000000000 ) ) ;
#1712 = CARTESIAN_POINT ( 'NONE',  ( -12.58639594889999991, -100.8746138070000029, -10.82789256390000077 ) ) ;
#1713 = EDGE_CURVE ( 'NONE', #19059, #1149, #27914, .T. ) ;
#1714 = FACE_OUTER_BOUND ( 'NONE', #309, .T. ) ;
#1715 = VERTEX_POINT ( 'NONE', #25265 ) ;
#1716 = EDGE_CURVE ( 'NONE', #21012, #3837, #1830, .T. ) ;
#1717 = CARTESIAN_POINT ( 'NONE',  ( -0.9302893022191279782, -101.6077248516953091, -16.00345022493254632 ) ) ;
#1718 = CARTESIAN_POINT ( 'NONE',  ( -32.46211842109999424, -74.14773635299999910, -21.81756538839999848 ) ) ;
#1719 = CARTESIAN_POINT ( 'NONE',  ( 36.27185351749999853, -79.54415414250000538, -14.99731109350000047 ) ) ;
#1720 = ORIENTED_EDGE ( 'NONE', *, *, #25096, .T. ) ;
#1721 = EDGE_CURVE ( 'NONE', #7623, #8093, #9792, .T. ) ;
#1722 = EDGE_CURVE ( 'NONE', #27046, #26262, #25796, .T. ) ;
#1723 = CARTESIAN_POINT ( 'NONE',  ( 6.669678980424931680, -101.2145573445209408, 14.91311433900129124 ) ) ;
#1724 = CARTESIAN_POINT ( 'NONE',  ( -1.738885961541629666, -80.13325245167779087, 47.03841520617770300 ) ) ;
#1725 = EDGE_LOOP ( 'NONE', ( #14448, #4958, #14088, #20508 ) ) ;
#1726 = CARTESIAN_POINT ( 'NONE',  ( -19.97841359259663463, -95.83493812764778852, 9.662536293482050453 ) ) ;
#1727 = EDGE_LOOP ( 'NONE', ( #27654, #27698, #9884 ) ) ;
#1728 = CARTESIAN_POINT ( 'NONE',  ( 20.64374438970000014, -57.47815920199999340, 10.93952083480000148 ) ) ;
#1729 = CARTESIAN_POINT ( 'NONE',  ( -10.20110288159999890, -74.50000000000000000, -41.00000000000000000 ) ) ;
#1730 = ORIENTED_EDGE ( 'NONE', *, *, #25632, .T. ) ;
#1731 = CARTESIAN_POINT ( 'NONE',  ( -3.236852559049167244, -97.42330309947865885, -20.32638677250028891 ) ) ;
#1732 = CARTESIAN_POINT ( 'NONE',  ( 0.000000000000000000, -11.00000000000000000, 0.000000000000000000 ) ) ;
#1733 = EDGE_LOOP ( 'NONE', ( #13344, #12764, #17680, #18232 ) ) ;
#1734 = CARTESIAN_POINT ( 'NONE',  ( 22.48186363828591894, -37.98173178126330640, -9.189959888866203741 ) ) ;
#1735 = CARTESIAN_POINT ( 'NONE',  ( -11.62178420722295691, -60.93032377504753327, -22.92104515723715608 ) ) ;
#1736 = CARTESIAN_POINT ( 'NONE',  ( -18.26810397560000254, -94.98812477769999418, 16.32728546869999775 ) ) ;
#1737 = ORIENTED_EDGE ( 'NONE', *, *, #10273, .F. ) ;
#1738 = FACE_OUTER_BOUND ( 'NONE', #12011, .T. ) ;
#1739 = CARTESIAN_POINT ( 'NONE',  ( 12.67716433170000023, -100.8815367389999977, -9.218731588149999823 ) ) ;
#1740 = DIRECTION ( 'NONE',  ( -0.5439177849611204207, 0.000000000000000000, 0.8391385125251898947 ) ) ;
#1741 = DIRECTION ( 'NONE',  ( 0.000000000000000000, 0.000000000000000000, 1.000000000000000000 ) ) ;
#1742 = CIRCLE ( 'NONE', #25487, 24.40223267850000255 ) ;
#1743 = CARTESIAN_POINT ( 'NONE',  ( 29.90142803373326430, -92.53260370668940027, 6.013043342471341646 ) ) ;
#1744 = FACE_OUTER_BOUND ( 'NONE', #12394, .T. ) ;
#1745 = EDGE_LOOP ( 'NONE', ( #28367, #3983, #28795, #25857, #18074, #16586 ) ) ;
#1746 = EDGE_CURVE ( 'NONE', #914, #1181, #8053, .T. ) ;
#1747 = CARTESIAN_POINT ( 'NONE',  ( -35.61208719050000582, -63.50000000000000000, 2.397127693020000283 ) ) ;
#1748 = CARTESIAN_POINT ( 'NONE',  ( 8.677144207910000517, -37.95796631070000160, -21.92880662259999980 ) ) ;
#1749 = CARTESIAN_POINT ( 'NONE',  ( 38.71641001238787538, -73.63089972761061119, 7.135467692469591228 ) ) ;
#1750 = DIRECTION ( 'NONE',  ( 0.4794255386042040046, 0.000000000000000000, 0.8775825618903722036 ) ) ;
#1751 = CARTESIAN_POINT ( 'NONE',  ( 0.04581334808960710325, -92.83865970263813949, -30.49996578665741964 ) ) ;
#1752 = DIRECTION ( 'NONE',  ( 0.4794255386042059475, 0.000000000000000000, 0.8775825618903710934 ) ) ;
#1753 = EDGE_CURVE ( 'NONE', #8830, #25924, #27612, .T. ) ;
#1754 = AXIS2_PLACEMENT_3D ( 'NONE', #18412, #27301, #9794 ) ;
#1755 = DIRECTION ( 'NONE',  ( 1.000000000000000000, 0.000000000000000000, 0.000000000000000000 ) ) ;
#1756 = DIRECTION ( 'NONE',  ( 0.3687499999999825917, 0.000000000000000000, -0.9295286103719523352 ) ) ;
#1757 = ORIENTED_EDGE ( 'NONE', *, *, #22845, .T. ) ;
#1758 = B_SPLINE_CURVE_WITH_KNOTS ( 'NONE', 3,
 ( #21021, #28254, #17188, #26076, #23337, #25524, #6108, #3384, #14982, #1215, #1081, #10050, #18964 ),
 .UNSPECIFIED., .F., .F.,
 ( 4, 2, 1, 1, 1, 2, 2, 4 ),
 ( 0.000000000000000000, 0.2500000000000480171, 0.3750000000000684452, 0.4375000000000789369, 0.4687500000000875411, 0.4843750000000882627, 0.5000000000000889289, 1.000000000000000000 ),
 .UNSPECIFIED. ) ;
#1759 = CARTESIAN_POINT ( 'NONE',  ( 20.08451038129999944, -35.57151704429999484, -8.961080048699999523 ) ) ;
#1760 = ORIENTED_EDGE ( 'NONE', *, *, #23659, .T. ) ;
#1761 = CARTESIAN_POINT ( 'NONE',  ( 21.38844997820000060, -36.30219044460000077, -7.879643458169998560 ) ) ;
#1762 = CARTESIAN_POINT ( 'NONE',  ( 9.405437324544319466, -35.99659153760200780, -19.87545419078008635 ) ) ;
#1763 = VERTEX_POINT ( 'NONE', #25404 ) ;
#1764 = CARTESIAN_POINT ( 'NONE',  ( -13.00841234930000034, -100.9763228559999959, -8.758810206009998822 ) ) ;
#1765 = B_SPLINE_SURFACE_WITH_KNOTS ( 'NONE', 5, 5, ( 
 ( #27754, #27623, #7793, #23237, #978, #18727, #20772, #16084, #5018 ),
 ( #24985, #13907, #25428, #20624, #12140, #27474, #5458, #7520, #14341 ),
 ( #5321, #16664, #3284, #9531, #25562, #14478, #18433, #27322, #25291 ),
 ( #7363, #16226, #3142, #25140, #14209, #14054, #3003, #23101, #11998 ),
 ( #28030, #12832, #19003, #7928, #25848, #17377, #26270, #6292, #4108 ),
 ( #3692, #15159, #28294, #27883, #1662, #14748, #10365, #19279, #12554 ),
 ( #24068, #17085, #1521, #21744, #28167, #16812, #5735, #1793, #23933 ),
 ( #8066, #16957, #12979, #14619, #21891, #3972, #19138, #3831, #8328 ),
 ( #25708, #1384, #5869, #8199, #10500, #19414, #23649, #21466, #25978 ),
 ( #6004, #14884, #26121, #10639, #10085, #12411, #23520, #8475, #23793 ),
 ( #19551, #12693, #17230, #21607, #3556, #21325, #10227, #6149, #15019 ),
 ( #28440, #2524, #15903, #24662, #4693, #9193, #15301, #27001, #348 ) ),
 .UNSPECIFIED., .F., .F., .F.,
 ( 6, 3, 3, 6 ),
 ( 6, 3, 6 ),
 ( 0.8942436407639999807, 1.876087175710000166, 3.176036816339999902, 5.425307607549999744 ),
 ( 0.000000000000000000, 0.2500000000000000000, 0.5000000000000000000 ),
 .UNSPECIFIED. ) ;
#1766 = DIRECTION ( 'NONE',  ( 0.4794255386042040046, 0.000000000000000000, 0.8775825618903720926 ) ) ;
#1767 = CARTESIAN_POINT ( 'NONE',  ( 8.185346967789998374, -101.1889999979999999, 14.03998109830000018 ) ) ;
#1768 = DIRECTION ( 'NONE',  ( 0.4794255386042000078, 0.000000000000000000, 0.8775825618903743131 ) ) ;
#1769 = DIRECTION ( 'NONE',  ( 0.000000000000000000, 1.000000000000000000, 0.000000000000000000 ) ) ;
#1770 = CARTESIAN_POINT ( 'NONE',  ( -29.74546239500669031, -92.83865970263998690, 6.742216160683305759 ) ) ;
#1771 = DIRECTION ( 'NONE',  ( 0.000000000000000000, 1.000000000000000000, 0.000000000000000000 ) ) ;
#1772 = ORIENTED_EDGE ( 'NONE', *, *, #19405, .T. ) ;
#1773 = VECTOR ( 'NONE', #7996, 1000.000000000000000 ) ;
#1774 = CARTESIAN_POINT ( 'NONE',  ( 13.62782804938226100, -100.4211561362012333, -10.10291547818408908 ) ) ;
#1775 = CARTESIAN_POINT ( 'NONE',  ( 22.29336127690000069, -27.06642317520000063, -0.5094344447499999928 ) ) ;
#1776 = CARTESIAN_POINT ( 'NONE',  ( 24.56539770530000055, -65.28594186049998882, 10.83220590859999888 ) ) ;
#1777 = CARTESIAN_POINT ( 'NONE',  ( -15.69013080879999933, -101.5700432450000079, 3.430602099230000146 ) ) ;
#1778 = ORIENTED_EDGE ( 'NONE', *, *, #20203, .T. ) ;
#1779 = CARTESIAN_POINT ( 'NONE',  ( 25.26718046270000073, -19.50000000000000000, 6.129403842640000377 ) ) ;
#1780 = CARTESIAN_POINT ( 'NONE',  ( 46.25000000000000000, -75.00000000000000000, -14.75000000000000000 ) ) ;
#1781 = DIRECTION ( 'NONE',  ( 1.000000000000000000, 0.000000000000000000, 0.000000000000000000 ) ) ;
#1782 = CARTESIAN_POINT ( 'NONE',  ( -10.20110288159999890, -84.50000000000000000, 41.00000000000000000 ) ) ;
#1783 = ORIENTED_EDGE ( 'NONE', *, *, #3085, .F. ) ;
#1784 = ADVANCED_FACE ( 'NONE', ( #5432 ), #27992, .T. ) ;
#1785 = DIRECTION ( 'NONE',  ( 0.000000000000000000, -1.000000000000000000, 0.000000000000000000 ) ) ;
#1786 =( GEOMETRIC_REPRESENTATION_CONTEXT ( 3 ) GLOBAL_UNCERTAINTY_ASSIGNED_CONTEXT ( ( #20546 ) ) GLOBAL_UNIT_ASSIGNED_CONTEXT ( ( #25669, #21288, #14718 ) ) REPRESENTATION_CONTEXT ( 'NONE', 'WORKASPACE' ) );
#1787 = CARTESIAN_POINT ( 'NONE',  ( -0.1068060827170000116, -101.3256027139999986, -15.90648277770000085 ) ) ;
#1788 = CARTESIAN_POINT ( 'NONE',  ( 10.08508133319999978, -64.24504434620000382, -24.78974410990000266 ) ) ;
#1789 = CARTESIAN_POINT ( 'NONE',  ( 14.95019707159999989, -101.2530993000000024, 2.710463435300000334 ) ) ;
#1790 = CARTESIAN_POINT ( 'NONE',  ( -7.135467526410000261, -73.50000000000000000, -38.71641004229999794 ) ) ;
#1791 = CARTESIAN_POINT ( 'NONE',  ( -36.87700573890000300, -65.19264941160000149, 0.2176643648599999870 ) ) ;
#1792 = ORIENTED_EDGE ( 'NONE', *, *, #3223, .F. ) ;
#1793 = CARTESIAN_POINT ( 'NONE',  ( 6.130772363030000172, -100.7776802639999971, 14.57128679989999931 ) ) ;
#1794 = CARTESIAN_POINT ( 'NONE',  ( 15.61826386989999982, -101.5964542560000012, 3.655520785480000256 ) ) ;
#1795 = B_SPLINE_CURVE_WITH_KNOTS ( 'NONE', 3,
 ( #12986, #4262, #8757, #13282, #28447, #17818, #22047, #8333, #26558, #2097, #21895 ),
 .UNSPECIFIED., .F., .F.,
 ( 4, 2, 1, 2, 2, 4 ),
 ( 0.000000000000000000, 0.2499999999999964473, 0.3750000000000006661, 0.4375000000000029976, 0.5000000000000053291, 1.000000000000000000 ),
 .UNSPECIFIED. ) ;
#1796 = AXIS2_PLACEMENT_3D ( 'NONE', #16588, #449, #9298 ) ;
#1797 = ORIENTED_EDGE ( 'NONE', *, *, #15743, .F. ) ;
#1798 = CARTESIAN_POINT ( 'NONE',  ( -40.42464116754384662, -65.66731758214605463, -2.269131925652129400 ) ) ;
#1799 = CARTESIAN_POINT ( 'NONE',  ( 4.060520888432426645, -92.92035259772417533, -30.22975431335808594 ) ) ;
#1800 = TOROIDAL_SURFACE ( 'NONE', #9229, 3.500000000000000000, 0.5000000000000000000 ) ;
#1801 = CARTESIAN_POINT ( 'NONE',  ( -25.02601311510000315, -11.00000000000000000, -45.80980973070000317 ) ) ;
#1802 = ORIENTED_EDGE ( 'NONE', *, *, #26480, .T. ) ;
#1803 = CARTESIAN_POINT ( 'NONE',  ( 6.508840722400000445, -93.07154530319999708, -26.20378082560000266 ) ) ;
#1804 = ADVANCED_FACE ( 'NONE', ( #10471 ), #5652, .T. ) ;
#1805 = DIRECTION ( 'NONE',  ( 1.000000000000000000, 0.000000000000000000, 0.000000000000000000 ) ) ;
#1806 = CARTESIAN_POINT ( 'NONE',  ( -6.863006950479999979, -101.6484611540000031, 14.45362438769999969 ) ) ;
#1807 = ORIENTED_EDGE ( 'NONE', *, *, #16120, .T. ) ;
#1808 =( LENGTH_UNIT ( ) NAMED_UNIT ( * ) SI_UNIT ( .MILLI., .METRE. ) );
#1809 = CARTESIAN_POINT ( 'NONE',  ( -38.08919256720000135, -65.74290439030001210, 1.043878858160000034 ) ) ;
#1810 = ORIENTED_EDGE ( 'NONE', *, *, #2181, .T. ) ;
#1811 = CARTESIAN_POINT ( 'NONE',  ( 25.50885178510000273, -93.36531860459999166, -5.860088577239999985 ) ) ;
#1812 = CARTESIAN_POINT ( 'NONE',  ( -1.303833584549999980, -101.1364147039999892, -15.29041300709999796 ) ) ;
#1813 = CARTESIAN_POINT ( 'NONE',  ( -38.08875739639999836, -84.00000000000000000, -9.476764215410000247 ) ) ;
#1814 = CARTESIAN_POINT ( 'NONE',  ( -38.62788938250000115, -74.00000000000000000, -7.627566167509999495 ) ) ;
#1815 = B_SPLINE_CURVE_WITH_KNOTS ( 'NONE', 3,
 ( #16986, #5900, #1148, #14778, #20946, #5489 ),
 .UNSPECIFIED., .F., .F.,
 ( 4, 2, 4 ),
 ( 0.000000000000000000, 0.5000000000000000000, 1.000000000000000000 ),
 .UNSPECIFIED. ) ;
#1816 = CARTESIAN_POINT ( 'NONE',  ( 24.78974732560000405, -64.24504771300000527, -10.08508462690000052 ) ) ;
#1817 = EDGE_LOOP ( 'NONE', ( #741, #20053, #4243, #19995 ) ) ;
#1818 = DIRECTION ( 'NONE',  ( -0.5301416321220535632, 0.000000000000000000, -0.8479091047340895360 ) ) ;
#1819 = AXIS2_PLACEMENT_3D ( 'NONE', #7307, #9621, #5264 ) ;
#1820 = AXIS2_PLACEMENT_3D ( 'NONE', #12023, #27649, #7692 ) ;
#1821 = EDGE_CURVE ( 'NONE', #15112, #10772, #1555, .T. ) ;
#1822 = CARTESIAN_POINT ( 'NONE',  ( 0.000000000000000000, -94.59276292389999696, 0.000000000000000000 ) ) ;
#1823 = AXIS2_PLACEMENT_3D ( 'NONE', #14152, #18674, #23052 ) ;
#1824 = TOROIDAL_SURFACE ( 'NONE', #18111, 33.64999999999999858, 1.250000000000000000 ) ;
#1825 = CARTESIAN_POINT ( 'NONE',  ( -36.79999999999999716, -63.07912966450000880, -0.1732050807570000017 ) ) ;
#1826 = CARTESIAN_POINT ( 'NONE',  ( -18.60622341941390800, -19.47370675684462427, 13.24439685365035757 ) ) ;
#1827 = CARTESIAN_POINT ( 'NONE',  ( 7.356933014059999998, -36.56811127230000125, -21.47791253540000156 ) ) ;
#1828 = DIRECTION ( 'NONE',  ( 1.000000000000000000, 0.000000000000000000, 0.000000000000000000 ) ) ;
#1829 = ORIENTED_EDGE ( 'NONE', *, *, #7541, .F. ) ;
#1830 = B_SPLINE_CURVE_WITH_KNOTS ( 'NONE', 5,
 ( #7638, #953, #18842, #18258, #21168, #9645, #7194, #14027, #1091 ),
 .UNSPECIFIED., .F., .F.,
 ( 6, 3, 6 ),
 ( 0.000000000000000000, 0.3540406197649746955, 1.000000000000000000 ),
 .UNSPECIFIED. ) ;
#1831 = EDGE_CURVE ( 'NONE', #6421, #3937, #6162, .T. ) ;
#1832 = CARTESIAN_POINT ( 'NONE',  ( 36.50549972520000352, -74.62369755570000507, -14.71598444119999982 ) ) ;
#1833 = CARTESIAN_POINT ( 'NONE',  ( -2.637362731009999628, -63.41849336990000552, -25.81630194210000084 ) ) ;
#1834 = AXIS2_PLACEMENT_3D ( 'NONE', #19061, #20420, #490 ) ;
#1835 = CARTESIAN_POINT ( 'NONE',  ( 9.119206670260000536, -37.35114128690000257, -22.23223931510000284 ) ) ;
#1836 = CARTESIAN_POINT ( 'NONE',  ( -25.52588841249999874, -93.67384740769999496, -2.372690985960000276 ) ) ;
#1837 = CARTESIAN_POINT ( 'NONE',  ( -20.05193632720000352, -56.21886023140000077, 14.45194103890000115 ) ) ;
#1838 = CARTESIAN_POINT ( 'NONE',  ( -7.325370793560000315, -18.50000000000000000, -24.94672208400000102 ) ) ;
#1839 = VECTOR ( 'NONE', #23657, 1000.000000000000000 ) ;
#1840 = ADVANCED_FACE ( 'NONE', ( #6565 ), #11765, .T. ) ;
#1841 = CARTESIAN_POINT ( 'NONE',  ( 15.73597609990000024, -101.0405520670000072, 4.043504278899999527 ) ) ;
#1842 = ORIENTED_EDGE ( 'NONE', *, *, #21864, .F. ) ;
#1843 = CARTESIAN_POINT ( 'NONE',  ( -29.08514934200000113, -20.00000000000000000, -53.24000875469999983 ) ) ;
#1844 = CARTESIAN_POINT ( 'NONE',  ( -13.14229048259999999, -100.8869813350000015, -8.528548640909999534 ) ) ;
#1845 = ORIENTED_EDGE ( 'NONE', *, *, #10335, .T. ) ;
#1846 = CYLINDRICAL_SURFACE ( 'NONE', #7110, 57.74999999999999289 ) ;
#1847 = CARTESIAN_POINT ( 'NONE',  ( -14.01337419900000114, -80.50000122480000186, 36.66316728649999845 ) ) ;
#1848 = B_SPLINE_CURVE_WITH_KNOTS ( 'NONE', 3,
 ( #17090, #4113, #21330, #21747 ),
 .UNSPECIFIED., .F., .F.,
 ( 4, 4 ),
 ( 43.40831274110000493, 64.82354956899999365 ),
 .UNSPECIFIED. ) ;
#1849 = CARTESIAN_POINT ( 'NONE',  ( 21.68822907590000071, -32.69575302460000188, 9.703736337280000512 ) ) ;
#1850 = B_SPLINE_CURVE_WITH_KNOTS ( 'NONE', 5,
 ( #10509, #3704, #1672, #1953, #1531, #10376 ),
 .UNSPECIFIED., .F., .F.,
 ( 6, 6 ),
 ( 0.000000000000000000, 1.000000000000000000 ),
 .UNSPECIFIED. ) ;
#1851 = EDGE_CURVE ( 'NONE', #17518, #1013, #13144, .T. ) ;
#1852 = CARTESIAN_POINT ( 'NONE',  ( -22.17746619903529393, -74.18074980451231681, -32.62167336490611547 ) ) ;
#1853 = CARTESIAN_POINT ( 'NONE',  ( 21.93023569320000021, -18.86697026210000061, 9.455903453530000391 ) ) ;
#1854 = CARTESIAN_POINT ( 'NONE',  ( -32.27586754510721789, -74.04145547921538650, -22.09313380603792965 ) ) ;
#1855 = FACE_OUTER_BOUND ( 'NONE', #11619, .T. ) ;
#1856 = VERTEX_POINT ( 'NONE', #10899 ) ;
#1857 = CARTESIAN_POINT ( 'NONE',  ( -11.35954001540000036, -77.00000000000000000, 47.25000000000000000 ) ) ;
#1858 = CARTESIAN_POINT ( 'NONE',  ( -12.49636764419999935, -101.4908759489999994, -10.04157132919999995 ) ) ;
#1859 = CARTESIAN_POINT ( 'NONE',  ( -29.71161737690000137, -93.00000000000000000, 6.352311025380000586 ) ) ;
#1860 = ORIENTED_EDGE ( 'NONE', *, *, #26039, .T. ) ;
#1861 = AXIS2_PLACEMENT_3D ( 'NONE', #17056, #5971, #17345 ) ;
#1862 = CIRCLE ( 'NONE', #27464, 0.8000000000000003775 ) ;
#1863 = CARTESIAN_POINT ( 'NONE',  ( -0.9821106753968790182, -101.5839620086842814, -16.01831432786889664 ) ) ;
#1864 = CARTESIAN_POINT ( 'NONE',  ( -32.72159597179999935, -74.32000120609998817, -21.62349002899999917 ) ) ;
#1865 = CARTESIAN_POINT ( 'NONE',  ( 36.82697887429999639, -80.34292022450000559, -13.57704389889999952 ) ) ;
#1866 = ORIENTED_EDGE ( 'NONE', *, *, #9808, .T. ) ;
#1867 = CARTESIAN_POINT ( 'NONE',  ( -5.390285367900000679, -100.8869813350000015, 14.71056643040000012 ) ) ;
#1868 = CARTESIAN_POINT ( 'NONE',  ( -29.41275679339999982, -25.00000000000000000, -53.83969017199999740 ) ) ;
#1869 = ORIENTED_EDGE ( 'NONE', *, *, #16399, .F. ) ;
#1870 = CARTESIAN_POINT ( 'NONE',  ( -19.26625410581794995, -97.04909278841957132, 7.359652529508150742 ) ) ;
#1871 = VERTEX_POINT ( 'NONE', #26828 ) ;
#1872 = CARTESIAN_POINT ( 'NONE',  ( 20.80630267519999776, -56.26441942339999969, 10.67761382389999980 ) ) ;
#1873 = CARTESIAN_POINT ( 'NONE',  ( -15.43525743989999910, -101.1461852590000063, 4.782895807790000120 ) ) ;
#1874 = ORIENTED_EDGE ( 'NONE', *, *, #16751, .T. ) ;
#1875 = EDGE_CURVE ( 'NONE', #1478, #12096, #8721, .T. ) ;
#1876 = AXIS2_PLACEMENT_3D ( 'NONE', #18888, #21344, #19160 ) ;
#1877 = CARTESIAN_POINT ( 'NONE',  ( -41.84021856431421327, -65.74136842487146737, 1.169644296513078663 ) ) ;
#1878 = DIRECTION ( 'NONE',  ( 0.000000000000000000, 1.000000000000000000, 0.000000000000000000 ) ) ;
#1880 = EDGE_CURVE ( 'NONE', #10144, #21742, #24393, .T. ) ;
#1879 = VECTOR ( 'NONE', #28593, 1000.000000000000000 ) ;
#1881 = ORIENTED_EDGE ( 'NONE', *, *, #16956, .T. ) ;
#1882 = CARTESIAN_POINT ( 'NONE',  ( -14.42556421679999978, -92.50000000000000000, -2.978755036369999942 ) ) ;
#1883 = CARTESIAN_POINT ( 'NONE',  ( 8.677144179139999025, -37.95796631150000167, -21.92880660169999985 ) ) ;
#1884 = EDGE_CURVE ( 'NONE', #18491, #14378, #5952, .T. ) ;
#1885 = CARTESIAN_POINT ( 'NONE',  ( -18.77234060500000012, -92.65715406920001840, -20.69363841459999875 ) ) ;
#1886 = CARTESIAN_POINT ( 'NONE',  ( -15.94434063720000161, -93.10431551199999944, 24.00277150759999856 ) ) ;
#1887 = ORIENTED_EDGE ( 'NONE', *, *, #6683, .T. ) ;
#1888 = EDGE_CURVE ( 'NONE', #4529, #22228, #12584, .T. ) ;
#1889 = CARTESIAN_POINT ( 'NONE',  ( 12.67342850500000040, -100.8685038539999965, -9.320488510950001526 ) ) ;
#1890 = CARTESIAN_POINT ( 'NONE',  ( 43.75000000000000000, -69.00000000000000000, 5.357814579270000097E-15 ) ) ;
#1891 = CARTESIAN_POINT ( 'NONE',  ( -1.456904695340000000, -52.62618816519999854, -23.34673678599999747 ) ) ;
#1892 = CARTESIAN_POINT ( 'NONE',  ( 29.91164248172746198, -92.52640451552758805, 5.961874894218010645 ) ) ;
#1893 = CARTESIAN_POINT ( 'NONE',  ( -19.28592236889999612, -18.62259217289999924, 14.63927399419999986 ) ) ;
#1894 = ORIENTED_EDGE ( 'NONE', *, *, #28364, .T. ) ;
#1895 = CARTESIAN_POINT ( 'NONE',  ( 21.87916729830000051, -37.95567969540000064, -8.611777603180000185 ) ) ;
#1896 = FACE_OUTER_BOUND ( 'NONE', #24576, .T. ) ;
#1897 = CARTESIAN_POINT ( 'NONE',  ( -24.56259648705387022, -92.50000000000000000, -18.08169719992735480 ) ) ;
#1898 = CARTESIAN_POINT ( 'NONE',  ( -38.25000000000000000, -65.41419836839999391, 2.121055962339999823 ) ) ;
#1899 = CARTESIAN_POINT ( 'NONE',  ( 0.03433565797716789381, -92.82709422631805296, -30.49998078697906578 ) ) ;
#1900 = AXIS2_PLACEMENT_3D ( 'NONE', #27713, #25243, #5270 ) ;
#1901 = VECTOR ( 'NONE', #9739, 1000.000000000000000 ) ;
#1902 = CARTESIAN_POINT ( 'NONE',  ( 0.000000000000000000, 0.000000000000000000, 0.000000000000000000 ) ) ;
#1903 = CARTESIAN_POINT ( 'NONE',  ( 0.000000000000000000, -82.50000000000000000, 0.000000000000000000 ) ) ;
#1904 = ORIENTED_EDGE ( 'NONE', *, *, #14580, .T. ) ;
#1905 = CARTESIAN_POINT ( 'NONE',  ( 17.67606731260000075, -99.62155223519999936, 1.124352996140000061 ) ) ;
#1906 = ORIENTED_EDGE ( 'NONE', *, *, #23202, .T. ) ;
#1907 = CARTESIAN_POINT ( 'NONE',  ( 21.49312271550000020, -37.09790470500000481, -7.530701653909999571 ) ) ;
#1908 = CARTESIAN_POINT ( 'NONE',  ( -27.40038777100000189, -79.50000000000000000, -36.59277592640000165 ) ) ;
#1909 = ORIENTED_EDGE ( 'NONE', *, *, #3181, .F. ) ;
#1910 = CARTESIAN_POINT ( 'NONE',  ( 14.91172220540000026, -95.31428172910000285, 17.37540928339999979 ) ) ;
#1911 = ADVANCED_FACE ( 'NONE', ( #6716 ), #17337, .T. ) ;
#1912 = CARTESIAN_POINT ( 'NONE',  ( -3.380041727002253360, -68.16711249679821094, -27.59188392963350722 ) ) ;
#1913 = DIRECTION ( 'NONE',  ( 1.000000000000000000, 0.000000000000000000, 0.000000000000000000 ) ) ;
#1914 = ORIENTED_EDGE ( 'NONE', *, *, #6174, .F. ) ;
#1915 = DIRECTION ( 'NONE',  ( 0.000000000000000000, 1.000000000000000000, 0.000000000000000000 ) ) ;
#1916 = DIRECTION ( 'NONE',  ( 1.000000000000000000, 0.000000000000000000, 0.000000000000000000 ) ) ;
#1917 = CARTESIAN_POINT ( 'NONE',  ( 7.877988450750000204, -44.92713668140000038, -21.74683343669999758 ) ) ;
#1918 = CARTESIAN_POINT ( 'NONE',  ( -10.30842662390000086, -18.85738404119999956, -19.98383211290000006 ) ) ;
#1919 = AXIS2_PLACEMENT_3D ( 'NONE', #17218, #19402, #17074 ) ;
#1920 = CARTESIAN_POINT ( 'NONE',  ( -39.50000000000000000, -65.63577453799999262, 2.309401076760000393 ) ) ;
#1921 = ORIENTED_EDGE ( 'NONE', *, *, #12161, .F. ) ;
#1922 = VECTOR ( 'NONE', #14020, 1000.000000000000000 ) ;
#1923 = EDGE_CURVE ( 'NONE', #25992, #4890, #20258, .T. ) ;
#1924 = CARTESIAN_POINT ( 'NONE',  ( 38.08875739639999836, -80.50000000000000000, -9.476764215410000247 ) ) ;
#1925 = CIRCLE ( 'NONE', #12587, 0.5000000000000027756 ) ;
#1926 = CYLINDRICAL_SURFACE ( 'NONE', #6555, 2.999999999999996447 ) ;
#1927 = CARTESIAN_POINT ( 'NONE',  ( 25.61816187999999883, -70.36214388610000015, 11.04518488439999935 ) ) ;
#1928 = CARTESIAN_POINT ( 'NONE',  ( 10.17429874589999983, -95.72998414199999218, -19.97250627529999889 ) ) ;
#1929 = ORIENTED_EDGE ( 'NONE', *, *, #4004, .F. ) ;
#1930 = LINE ( 'NONE', #19682, #6678 ) ;
#1931 = CARTESIAN_POINT ( 'NONE',  ( -17.06129450210000087, -93.25667418180000823, 21.77310057969999946 ) ) ;
#1932 = CARTESIAN_POINT ( 'NONE',  ( 12.01015229399999917, -101.6484611540000031, -9.798277495349999811 ) ) ;
#1933 = ORIENTED_EDGE ( 'NONE', *, *, #10541, .T. ) ;
#1934 = CARTESIAN_POINT ( 'NONE',  ( 28.11846399170000055, -70.41239039510000453, 2.285062484099999569 ) ) ;
#1935 = CARTESIAN_POINT ( 'NONE',  ( 0.6434015132710000362, -100.4650220110000021, -16.82283554099999989 ) ) ;
#1936 = CARTESIAN_POINT ( 'NONE',  ( 8.064915741549999240, -60.56337174330000295, -22.40630470649999850 ) ) ;
#1937 = DIRECTION ( 'NONE',  ( 0.000000000000000000, -1.000000000000000000, 0.000000000000000000 ) ) ;
#1938 = CARTESIAN_POINT ( 'NONE',  ( 7.100559683520000220, -35.25283571269999783, -21.44183144160000154 ) ) ;
#1939 = CARTESIAN_POINT ( 'NONE',  ( 24.33707037739999990, -62.95235822580000473, -9.864745197619999573 ) ) ;
#1940 = EDGE_LOOP ( 'NONE', ( #1439, #20708, #6249, #12128, #12080 ) ) ;
#1941 = FACE_OUTER_BOUND ( 'NONE', #8168, .T. ) ;
#1942 = CARTESIAN_POINT ( 'NONE',  ( 15.52117313229999951, -101.2902355740000075, 3.579205768200000026 ) ) ;
#1943 = AXIS2_PLACEMENT_3D ( 'NONE', #22771, #11669, #20426 ) ;
#1944 = VERTEX_POINT ( 'NONE', #26975 ) ;
#1945 = DIRECTION ( 'NONE',  ( 0.000000000000000000, 1.000000000000000000, 0.000000000000000000 ) ) ;
#1946 = CARTESIAN_POINT ( 'NONE',  ( 21.21808891099999883, -34.59820414320000026, -7.670974023059999425 ) ) ;
#1947 = EDGE_CURVE ( 'NONE', #19954, #26186, #16169, .T. ) ;
#1948 = DIRECTION ( 'NONE',  ( 0.000000000000000000, 1.000000000000000000, 0.000000000000000000 ) ) ;
#1949 = EDGE_LOOP ( 'NONE', ( #6217, #17280, #3392, #19503 ) ) ;
#1950 = CARTESIAN_POINT ( 'NONE',  ( 3.404243284160000105, -93.04780269100000112, -28.95354108839999796 ) ) ;
#1951 = EDGE_CURVE ( 'NONE', #11794, #15559, #4788, .T. ) ;
#1952 = CARTESIAN_POINT ( 'NONE',  ( 47.25000000000000000, -82.25000000000000000, -2.331807164890000089E-15 ) ) ;
#1953 = CARTESIAN_POINT ( 'NONE',  ( -0.2283525300826651505, -93.01584921915402049, 26.42460210401236154 ) ) ;
#1954 = VERTEX_POINT ( 'NONE', #25078 ) ;
#1955 = LINE ( 'NONE', #3984, #21735 ) ;
#1956 = CARTESIAN_POINT ( 'NONE',  ( -13.25237707705474399, -99.99762666416590662, -11.12887180797588194 ) ) ;
#1957 = ORIENTED_EDGE ( 'NONE', *, *, #7433, .F. ) ;
#1958 = DIRECTION ( 'NONE',  ( 0.000000000000000000, -1.000000000000000000, 0.000000000000000000 ) ) ;
#1959 = CARTESIAN_POINT ( 'NONE',  ( 25.60466699379999866, -93.13207089229999269, -5.766591832619999636 ) ) ;
#1960 = EDGE_CURVE ( 'NONE', #26414, #9396, #2958, .T. ) ;
#1961 = CARTESIAN_POINT ( 'NONE',  ( -1.526197323679999940, -100.8869817940000075, -15.59251925729999932 ) ) ;
#1962 = CARTESIAN_POINT ( 'NONE',  ( 21.95427213460000004, -18.85488210659999808, 0.1375582407400000040 ) ) ;
#1963 = CARTESIAN_POINT ( 'NONE',  ( -38.70686962976382972, -73.76099270142834996, -7.188502612221714827 ) ) ;
#1964 = AXIS2_PLACEMENT_3D ( 'NONE', #16281, #18341, #9721 ) ;
#1965 = DIRECTION ( 'NONE',  ( 0.000000000000000000, 1.000000000000000000, 0.000000000000000000 ) ) ;
#1966 = B_SPLINE_CURVE_WITH_KNOTS ( 'NONE', 3,
 ( #12469, #3105, #929, #21380 ),
 .UNSPECIFIED., .F., .F.,
 ( 4, 4 ),
 ( 12.39809316140000028, 33.81329059560000161 ),
 .UNSPECIFIED. ) ;
#1967 = ORIENTED_EDGE ( 'NONE', *, *, #10658, .F. ) ;
#1968 = CARTESIAN_POINT ( 'NONE',  ( -14.58939485729999852, -101.2530991829999891, 4.248445246460000213 ) ) ;
#1969 = CIRCLE ( 'NONE', #18251, 20.64285714289999873 ) ;
#1970 = FACE_OUTER_BOUND ( 'NONE', #5837, .T. ) ;
#1971 = CARTESIAN_POINT ( 'NONE',  ( -36.77331348028479852, -65.13491442160928102, 0.1557320299044409329 ) ) ;
#1972 = CARTESIAN_POINT ( 'NONE',  ( 13.78283651632031770, -100.0559847774664775, -10.38643546923515970 ) ) ;
#1973 = CARTESIAN_POINT ( 'NONE',  ( -12.41808103320000001, -68.06111992670000177, -23.59934042399999754 ) ) ;
#1974 =( NAMED_UNIT ( * ) SI_UNIT ( $, .STERADIAN. ) SOLID_ANGLE_UNIT ( ) );
#1975 = CARTESIAN_POINT ( 'NONE',  ( 19.08554773649999703, -23.77700550180000150, -9.011477467469999780 ) ) ;
#1976 = ORIENTED_EDGE ( 'NONE', *, *, #15304, .F. ) ;
#1977 = CARTESIAN_POINT ( 'NONE',  ( 8.477761133450002262, -18.62065275650000018, -19.62439763160000084 ) ) ;
#1979 = CARTESIAN_POINT ( 'NONE',  ( 22.43277176080000146, -36.00000000000000000, -11.31764183710000005 ) ) ;
#1978 =( REPRESENTATION_RELATIONSHIP ('NONE','NONE', #26008, #24690 ) REPRESENTATION_RELATIONSHIP_WITH_TRANSFORMATION ( #18364 )SHAPE_REPRESENTATION_RELATIONSHIP( ) );
#1980 = TOROIDAL_SURFACE ( 'NONE', #18270, 3.500000000000000000, 0.5000000000000000000 ) ;
#1981 = CARTESIAN_POINT ( 'NONE',  ( -0.5884599110899999541, -61.88564085890000399, -23.95484640009999922 ) ) ;
#1982 = CARTESIAN_POINT ( 'NONE',  ( 9.276353521389999912, -36.53050716039999912, -21.68616227190000245 ) ) ;
#1983 = CARTESIAN_POINT ( 'NONE',  ( -18.88944331899999796, -101.1889999979999999, -23.13319212550000259 ) ) ;
#1984 = AXIS2_PLACEMENT_3D ( 'NONE', #28253, #19510, #26226 ) ;
#1985 = DIRECTION ( 'NONE',  ( 0.000000000000000000, 1.000000000000000000, 0.000000000000000000 ) ) ;
#1986 = LINE ( 'NONE', #6486, #21980 ) ;
#1987 = EDGE_CURVE ( 'NONE', #10101, #14792, #11184, .T. ) ;
#1988 = ORIENTED_EDGE ( 'NONE', *, *, #18804, .T. ) ;
#1989 = CARTESIAN_POINT ( 'NONE',  ( 21.18700933639999917, -34.99644735399999718, -7.990241917319999665 ) ) ;
#1990 = CARTESIAN_POINT ( 'NONE',  ( 7.250122995579999952, -74.26794181930000605, -40.35968420239999688 ) ) ;
#1991 = ORIENTED_EDGE ( 'NONE', *, *, #2998, .F. ) ;
#1992 = DIRECTION ( 'NONE',  ( 1.000000000000000000, 0.000000000000000000, 0.000000000000000000 ) ) ;
#1993 = EDGE_CURVE ( 'NONE', #12701, #3611, #23180, .T. ) ;
#1994 = DIRECTION ( 'NONE',  ( 0.000000000000000000, 0.000000000000000000, 1.000000000000000000 ) ) ;
#1995 = CARTESIAN_POINT ( 'NONE',  ( 22.75370980639999985, -39.29539198459999483, 10.16485029849999933 ) ) ;
#1996 = CARTESIAN_POINT ( 'NONE',  ( 27.18988201479999844, -31.10155444569999617, 49.77074518290000071 ) ) ;
#1997 = CARTESIAN_POINT ( 'NONE',  ( 20.89748452499999942, -18.85965710059999978, 9.255084173580000240 ) ) ;
#1998 = CARTESIAN_POINT ( 'NONE',  ( -31.64302845809999809, -80.00000000000000000, -31.64302845809999809 ) ) ;
#1999 = CARTESIAN_POINT ( 'NONE',  ( -17.58226716778080956, -94.81956704558760407, 15.60250440155592422 ) ) ;
#2000 = EDGE_LOOP ( 'NONE', ( #9337, #20592, #14416, #15306 ) ) ;
#2001 = AXIS2_PLACEMENT_3D ( 'NONE', #9830, #16390, #18737 ) ;
#2002 = AXIS2_PLACEMENT_3D ( 'NONE', #16319, #2648, #20557 ) ;
#2003 = DIRECTION ( 'NONE',  ( 0.000000000000000000, 1.000000000000000000, 0.000000000000000000 ) ) ;
#2004 = CARTESIAN_POINT ( 'NONE',  ( -11.86297998370000073, -101.1402801299999936, -9.726116368819999636 ) ) ;
#2005 = VECTOR ( 'NONE', #1563, 1000.000000000000000 ) ;
#2006 = SURFACE_STYLE_USAGE ( .BOTH. , #21957 ) ;
#2007 = CARTESIAN_POINT ( 'NONE',  ( 22.26662627820000040, -57.47855601759999900, -7.066909182079999852 ) ) ;
#2008 = EDGE_LOOP ( 'NONE', ( #908, #8153, #15070, #18161 ) ) ;
#2009 = EDGE_CURVE ( 'NONE', #27945, #3729, #16402, .T. ) ;
#2010 = CARTESIAN_POINT ( 'NONE',  ( -32.65293188559999749, -74.37556698459998472, -21.99847587569999874 ) ) ;
#2011 = CARTESIAN_POINT ( 'NONE',  ( 36.82697887990000396, -80.49999984420000487, -13.57704388640000026 ) ) ;
#2012 = VERTEX_POINT ( 'NONE', #7159 ) ;
#2013 = AXIS2_PLACEMENT_3D ( 'NONE', #7891, #16770, #5693 ) ;
#2014 = CARTESIAN_POINT ( 'NONE',  ( 28.69894351740000360, -74.00000000000000000, -10.33698117210000156 ) ) ;
#2015 = CARTESIAN_POINT ( 'NONE',  ( -11.91266501540000000, -74.00000000000000000, 46.64429291560000479 ) ) ;
#2016 = CARTESIAN_POINT ( 'NONE',  ( -0.6273717453279999967, -62.97603269449999885, -24.27362655359999977 ) ) ;
#2017 = ORIENTED_EDGE ( 'NONE', *, *, #11344, .F. ) ;
#2018 = SHAPE_REPRESENTATION ( 'Pump Drive Shaft', ( #26433 ), #4100 ) ;
#2019 = CARTESIAN_POINT ( 'NONE',  ( -19.74515506783779628, -96.28273967183713467, 8.793340612910874654 ) ) ;
#2020 = VERTEX_POINT ( 'NONE', #2939 ) ;
#2021 = CARTESIAN_POINT ( 'NONE',  ( 22.10956385849999961, -93.90388243319999617, 13.35155070529999932 ) ) ;
#2022 = VERTEX_POINT ( 'NONE', #18224 ) ;
#2023 = AXIS2_PLACEMENT_3D ( 'NONE', #12263, #20751, #18979 ) ;
#2024 = CARTESIAN_POINT ( 'NONE',  ( -41.80262105942959749, -65.72848773093366503, 1.265555823039845151 ) ) ;
#2025 = CARTESIAN_POINT ( 'NONE',  ( -42.25000000000000000, -63.30468293320000583, -0.7216878364880000563 ) ) ;
#2026 = ORIENTED_EDGE ( 'NONE', *, *, #15396, .F. ) ;
#2027 = CARTESIAN_POINT ( 'NONE',  ( 11.99447238389999981, -101.1411470200000053, -9.642266023979999545 ) ) ;
#2028 = CARTESIAN_POINT ( 'NONE',  ( -20.38769392570000250, -92.57423544259999915, -20.43327123240000276 ) ) ;
#2029 = CARTESIAN_POINT ( 'NONE',  ( -3.501402190497391764, -79.99970154920160326, 46.83644880644524022 ) ) ;
#2030 = VERTEX_POINT ( 'NONE', #22749 ) ;
#2031 = DIRECTION ( 'NONE',  ( 0.000000000000000000, -1.000000000000000000, 0.000000000000000000 ) ) ;
#2032 = CARTESIAN_POINT ( 'NONE',  ( 13.24160441829999968, -100.4808658609999981, -9.370009802470001148 ) ) ;
#2033 = CARTESIAN_POINT ( 'NONE',  ( -9.348798002780000616, -13.50000000000000000, -17.11285995690000306 ) ) ;
#2034 = CARTESIAN_POINT ( 'NONE',  ( -2.565581297390000071, -56.20810645120000260, -24.89562038480000083 ) ) ;
#2035 = CIRCLE ( 'NONE', #21558, 3.750000000000000000 ) ;
#2036 = CARTESIAN_POINT ( 'NONE',  ( 21.91842626080000045, -37.33819205729999879, -8.685017708060000174 ) ) ;
#2037 = CARTESIAN_POINT ( 'NONE',  ( 11.35129741066615772, -72.28566294331933761, -26.99897349783034173 ) ) ;
#2038 = DIRECTION ( 'NONE',  ( 1.000000000000000000, 0.000000000000000000, 0.000000000000000000 ) ) ;
#2039 = VERTEX_POINT ( 'NONE', #2791 ) ;
#2040 = DIRECTION ( 'NONE',  ( 1.000000000000000000, 0.000000000000000000, 0.000000000000000000 ) ) ;
#2041 = DIRECTION ( 'NONE',  ( 0.4794255386042036715, 0.000000000000000000, 0.8775825618903724257 ) ) ;
#2042 = CARTESIAN_POINT ( 'NONE',  ( 0.000000000000000000, -17.50000000000000000, 0.000000000000000000 ) ) ;
#2043 = CARTESIAN_POINT ( 'NONE',  ( -0.1264782718447538534, -92.71619979444359672, -30.49973804731671478 ) ) ;
#2044 = DIRECTION ( 'NONE',  ( 0.000000000000000000, -1.000000000000000000, 0.000000000000000000 ) ) ;
#2045 = EDGE_CURVE ( 'NONE', #2214, #18911, #16432, .T. ) ;
#2046 = DIRECTION ( 'NONE',  ( 1.000000000000000000, 0.000000000000000000, 0.000000000000000000 ) ) ;
#2047 = CARTESIAN_POINT ( 'NONE',  ( 23.35417726369999869, -57.47855601759999900, -0.5711878298099999363 ) ) ;
#2048 = EDGE_CURVE ( 'NONE', #4023, #14266, #12241, .T. ) ;
#2049 = CYLINDRICAL_SURFACE ( 'NONE', #16359, 7.249999999999999112 ) ;
#2050 = EDGE_CURVE ( 'NONE', #2986, #9393, #22604, .T. ) ;
#2051 = ORIENTED_EDGE ( 'NONE', *, *, #10364, .F. ) ;
#2052 = VECTOR ( 'NONE', #28538, 1000.000000000000114 ) ;
#2053 = CARTESIAN_POINT ( 'NONE',  ( 15.58784585939999978, -100.8733984769999950, 2.070707821839999685 ) ) ;
#2054 = EDGE_LOOP ( 'NONE', ( #13030, #5016, #1072, #11165 ) ) ;
#2055 = AXIS2_PLACEMENT_3D ( 'NONE', #20796, #27499, #3031 ) ;
#2056 = CARTESIAN_POINT ( 'NONE',  ( -13.24460949610000071, -57.44036993110000111, 20.55651328140000089 ) ) ;
#2057 = CARTESIAN_POINT ( 'NONE',  ( 7.734359568749999525, -19.46510050329999686, -20.63161913629999944 ) ) ;
#2058 = ORIENTED_EDGE ( 'NONE', *, *, #21512, .F. ) ;
#2059 = CARTESIAN_POINT ( 'NONE',  ( 15.98190517250000120, -101.1461874320000049, 2.387865266659999985 ) ) ;
#2060 = CARTESIAN_POINT ( 'NONE',  ( -3.158285342964013864, -66.99924750834972542, -27.22922173955624103 ) ) ;
#2061 = ORIENTED_EDGE ( 'NONE', *, *, #5282, .T. ) ;
#2062 = CARTESIAN_POINT ( 'NONE',  ( -0.7543003842240000312, -111.0000000000000000, -16.73300722909999649 ) ) ;
#2063 = CARTESIAN_POINT ( 'NONE',  ( 7.844113379649998663, -101.1184174639999895, 13.21637662110000022 ) ) ;
#2064 = CARTESIAN_POINT ( 'NONE',  ( 1.375225265779999928, -94.98812079580000045, 24.46248543800000164 ) ) ;
#2065 = CARTESIAN_POINT ( 'NONE',  ( 7.554088719370000149, -44.93138465010000004, -21.71814693689999842 ) ) ;
#2066 = CIRCLE ( 'NONE', #26248, 4.999999999999999112 ) ;
#2067 = CARTESIAN_POINT ( 'NONE',  ( -29.70880753679850628, -92.72059904818995335, 6.901939759926293938 ) ) ;
#2068 = DIRECTION ( 'NONE',  ( 0.4794255386042040601, 0.000000000000000000, 0.8775825618903720926 ) ) ;
#2069 = ORIENTED_EDGE ( 'NONE', *, *, #6148, .T. ) ;
#2070 = DIRECTION ( 'NONE',  ( 1.000000000000000000, 0.000000000000000000, 0.000000000000000000 ) ) ;
#2071 = CARTESIAN_POINT ( 'NONE',  ( 23.77822920909999738, -34.63364287800000341, 1.297513282619999986 ) ) ;
#2072 = DIRECTION ( 'NONE',  ( 0.000000000000000000, -1.000000000000000000, 0.000000000000000000 ) ) ;
#2073 = CARTESIAN_POINT ( 'NONE',  ( 39.68146194264046045, -73.78481856921511906, 7.243236069894346763 ) ) ;
#2074 = ORIENTED_EDGE ( 'NONE', *, *, #13986, .F. ) ;
#2075 = CIRCLE ( 'NONE', #15073, 1.000000000000000888 ) ;
#2076 = CARTESIAN_POINT ( 'NONE',  ( -38.62788659690000515, -74.00000000000000000, 7.627568735119999666 ) ) ;
#2077 = CARTESIAN_POINT ( 'NONE',  ( -15.25169713729999899, -93.03108158919999937, 25.12655145109999921 ) ) ;
#2078 = CARTESIAN_POINT ( 'NONE',  ( -19.16019836899999618, -92.50000000000000000, 22.97842938279999814 ) ) ;
#2079 = ORIENTED_EDGE ( 'NONE', *, *, #21648, .T. ) ;
#2080 = CARTESIAN_POINT ( 'NONE',  ( 28.64987595179999857, -71.11747349450000399, 2.769230177229999867 ) ) ;
#2081 = AXIS2_PLACEMENT_3D ( 'NONE', #17645, #14108, #20674 ) ;
#2082 = CARTESIAN_POINT ( 'NONE',  ( 0.8390948241760000093, -99.74726900420000675, -17.13497999810000039 ) ) ;
#2083 = CARTESIAN_POINT ( 'NONE',  ( 7.066909115259999652, -57.47855582819999398, -22.26662700550000196 ) ) ;
#2084 = CARTESIAN_POINT ( 'NONE',  ( -12.80265261289999934, -69.66305826589999128, -24.04850811530000243 ) ) ;
#2085 = ADVANCED_FACE ( 'NONE', ( #25503 ), #5278, .F. ) ;
#2086 = CARTESIAN_POINT ( 'NONE',  ( -11.38378090099999973, -42.27112620159999778, -19.87481931789999834 ) ) ;
#2087 = ORIENTED_EDGE ( 'NONE', *, *, #429, .T. ) ;
#2088 = ADVANCED_FACE ( 'NONE', ( #9471 ), #18377, .F. ) ;
#2089 = CARTESIAN_POINT ( 'NONE',  ( 26.96515717169932458, -69.06126107724072938, 0.3323215380678566366 ) ) ;
#2090 = DIRECTION ( 'NONE',  ( 0.000000000000000000, -1.000000000000000000, 0.000000000000000000 ) ) ;
#2091 = ADVANCED_FACE ( 'NONE', ( #11496 ), #477, .T. ) ;
#2092 = EDGE_CURVE ( 'NONE', #20079, #20678, #14144, .T. ) ;
#2093 = ORIENTED_EDGE ( 'NONE', *, *, #3385, .T. ) ;
#2094 = CARTESIAN_POINT ( 'NONE',  ( 28.18364776602151167, -92.64884742710839305, 11.65904703969763112 ) ) ;
#2095 = CARTESIAN_POINT ( 'NONE',  ( 15.29251030651879439, -101.1416252791453019, 2.772524658013501675 ) ) ;
#2096 = AXIS2_PLACEMENT_3D ( 'NONE', #17159, #12767, #26049 ) ;
#2097 = CARTESIAN_POINT ( 'NONE',  ( -42.18414812522917146, -65.66527319018285880, -0.7597074341180621859 ) ) ;
#2098 = LINE ( 'NONE', #24516, #20244 ) ;
#2099 = CARTESIAN_POINT ( 'NONE',  ( -1.469243280769999993, -101.0356131030000029, -15.40539586329999899 ) ) ;
#2100 = DIRECTION ( 'NONE',  ( 0.000000000000000000, 1.000000000000000000, 0.000000000000000000 ) ) ;
#2101 = ORIENTED_EDGE ( 'NONE', *, *, #19442, .F. ) ;
#2102 = CIRCLE ( 'NONE', #21640, 34.89999999999999858 ) ;
#2103 = CARTESIAN_POINT ( 'NONE',  ( 47.25000000000000000, -80.00000000000000000, 8.881784196999999612E-15 ) ) ;
#2104 = CARTESIAN_POINT ( 'NONE',  ( -6.665307709260000379, -111.0000000000000000, -13.13558364449999871 ) ) ;
#2105 = ORIENTED_EDGE ( 'NONE', *, *, #8436, .T. ) ;
#2106 = CARTESIAN_POINT ( 'NONE',  ( 8.882291244119999263, -35.85669613890000562, -20.42811047029999827 ) ) ;
#2107 = CARTESIAN_POINT ( 'NONE',  ( 9.356041104380000917, -74.00000000000000000, 37.60355029590000697 ) ) ;
#2108 = EDGE_LOOP ( 'NONE', ( #25166, #6629, #28009, #13082 ) ) ;
#2109 = CARTESIAN_POINT ( 'NONE',  ( -0.8337756410959999975, -101.5369810359999860, -15.97866295649999913 ) ) ;
#2110 = CARTESIAN_POINT ( 'NONE',  ( 21.84042253680000201, -18.61797548019999837, 0.5293533609709999421 ) ) ;
#2111 = CARTESIAN_POINT ( 'NONE',  ( -12.11328434900106288, -19.47102482557679437, 19.13567261410544162 ) ) ;
#2112 = FACE_OUTER_BOUND ( 'NONE', #6314, .T. ) ;
#2113 = CARTESIAN_POINT ( 'NONE',  ( -20.66056017707865422, -92.75430643271349140, -22.43644101044492700 ) ) ;
#2114 = DIRECTION ( 'NONE',  ( 0.000000000000000000, -1.000000000000000000, 0.000000000000000000 ) ) ;
#2115 = DIRECTION ( 'NONE',  ( 0.000000000000000000, 1.000000000000000000, 0.000000000000000000 ) ) ;
#2116 = CARTESIAN_POINT ( 'NONE',  ( 6.974892859179999682, -49.11505549650000546, -21.98941332900000134 ) ) ;
#2117 = AXIS2_PLACEMENT_3D ( 'NONE', #18371, #11937, #5104 ) ;
#2118 = DIRECTION ( 'NONE',  ( 0.4794255386042041156, 0.000000000000000000, 0.8775825618903722036 ) ) ;
#2119 = DIRECTION ( 'NONE',  ( 0.000000000000000000, 1.000000000000000000, 0.000000000000000000 ) ) ;
#2120 = DIRECTION ( 'NONE',  ( 0.2287893768880238932, 0.000000000000000000, -0.9734759478401044941 ) ) ;
#2121 = CARTESIAN_POINT ( 'NONE',  ( 26.51311248191242242, -93.18010901228015541, 10.50323123315586926 ) ) ;
#2122 = ORIENTED_EDGE ( 'NONE', *, *, #16389, .F. ) ;
#2123 = ADVANCED_FACE ( 'NONE', ( #915 ), #19653, .F. ) ;
#2124 = CARTESIAN_POINT ( 'NONE',  ( 8.426926234210000644, -18.85979317139999978, -20.10370215430000229 ) ) ;
#2125 = EDGE_CURVE ( 'NONE', #5033, #6426, #24805, .T. ) ;
#2126 = ORIENTED_EDGE ( 'NONE', *, *, #907, .F. ) ;
#2127 = CARTESIAN_POINT ( 'NONE',  ( -13.64611331559999918, -63.24140639400000197, 21.34096686680000232 ) ) ;
#2128 = CARTESIAN_POINT ( 'NONE',  ( -25.71305159770000159, -93.90388142500000868, -2.436348821509999762 ) ) ;
#2129 = DIRECTION ( 'NONE',  ( 0.9993816408608722224, 0.000000000000000000, -0.03516156865429610756 ) ) ;
#2130 = VERTEX_POINT ( 'NONE', #7867 ) ;
#2131 = SURFACE_SIDE_STYLE ('',( #22672 ) ) ;
#2132 = CYLINDRICAL_SURFACE ( 'NONE', #20604, 0.7999999999999994893 ) ;
#2133 = ORIENTED_EDGE ( 'NONE', *, *, #9374, .F. ) ;
#2134 = DIRECTION ( 'NONE',  ( 0.4794255386042040601, 0.000000000000000000, 0.8775825618903720926 ) ) ;
#2135 = FACE_OUTER_BOUND ( 'NONE', #19826, .T. ) ;
#2136 = CARTESIAN_POINT ( 'NONE',  ( 21.33821989950000031, -45.98073373389999574, 9.994986904390001925 ) ) ;
#2137 = CIRCLE ( 'NONE', #22635, 52.86371681420000357 ) ;
#2138 = PLANE ( 'NONE',  #18692 ) ;
#2139 = CARTESIAN_POINT ( 'NONE',  ( 24.45765515529999945, -92.57423544259999915, -15.32970127379999958 ) ) ;
#2140 = CARTESIAN_POINT ( 'NONE',  ( 19.85636362560000023, -19.46458168450000059, 9.829421693009999572 ) ) ;
#2141 = CARTESIAN_POINT ( 'NONE',  ( 9.797124920099999912, -69.55058719230000008, -25.58514975119999946 ) ) ;
#2142 = CARTESIAN_POINT ( 'NONE',  ( -16.17553334493379324, -99.16532134656523567, 7.643797697565219096 ) ) ;
#2143 = EDGE_LOOP ( 'NONE', ( #25750, #28206, #7134, #28651 ) ) ;
#2144 = CARTESIAN_POINT ( 'NONE',  ( -11.78425688200000110, -72.00000000000000000, -26.58404760160000180 ) ) ;
#2145 = CARTESIAN_POINT ( 'NONE',  ( -12.83089869019999973, -99.70407914540000149, -11.44895565849999919 ) ) ;
#2146 = CARTESIAN_POINT ( 'NONE',  ( -23.16986609970000188, -72.82938648530000592, 16.90925194980000157 ) ) ;
#2147 = CARTESIAN_POINT ( 'NONE',  ( 23.17288685498201417, -62.96215878643922537, -7.400562784300776187 ) ) ;
#2148 = VERTEX_POINT ( 'NONE', #14824 ) ;
#2149 = EDGE_CURVE ( 'NONE', #22535, #22268, #465, .T. ) ;
#2150 = DIRECTION ( 'NONE',  ( 0.4794255386042036715, 0.000000000000000000, 0.8775825618903724257 ) ) ;
#2151 = CARTESIAN_POINT ( 'NONE',  ( -32.57680276909999151, -74.14930846740000447, -22.16666910030000182 ) ) ;
#2152 = DIRECTION ( 'NONE',  ( 0.000000000000000000, 1.000000000000000000, 0.000000000000000000 ) ) ;
#2153 = VERTEX_POINT ( 'NONE', #27966 ) ;
#2154 = ADVANCED_FACE ( 'NONE', ( #23872, #16748 ), #8005, .T. ) ;
#2155 = B_SPLINE_CURVE_WITH_KNOTS ( 'NONE', 3,
 ( #24777, #18659, #763, #20704, #9313, #20844, #18508, #7452, #18803, #906, #27402, #16309, #20396, #27256, #20550, #12076, #20987, #5250, #25222, #1051, #7595, #27695, #25069, #2640, #18217, #9749, #7152, #25366, #18369, #9463, #22596, #27555, #22741, #14275, #16019, #4954, #7293 ),
 .UNSPECIFIED., .F., .F.,
 ( 4, 2, 2, 1, 1, 1, 2, 2, 2, 2, 1, 1, 1, 2, 2, 2, 2, 1, 1, 1, 2, 2, 4 ),
 ( 0.000000000000000000, 0.1250000000000014988, 0.1875000000000017208, 0.2187500000000023592, 0.2343750000000030254, 0.2421875000000027478, 0.2460937500000026368, 0.2500000000000025535, 0.3750000000000048850, 0.4375000000000060507, 0.4687500000000068834, 0.4843750000000068834, 0.4921875000000064948, 0.4960937500000062172, 0.5000000000000058842, 0.6250000000000046629, 0.6875000000000043299, 0.7187500000000041078, 0.7343750000000041078, 0.7421875000000041078, 0.7460937500000042188, 0.7500000000000042188, 1.000000000000000000 ),
 .UNSPECIFIED. ) ;
#2156 = DIRECTION ( 'NONE',  ( 0.000000000000000000, 1.000000000000000000, 0.000000000000000000 ) ) ;
#2157 = B_SPLINE_CURVE_WITH_KNOTS ( 'NONE', 3,
 ( #26786, #13497, #22405, #6667, #4181, #13052, #21965, #15532, #15680, #2158, #20211 ),
 .UNSPECIFIED., .F., .F.,
 ( 4, 1, 1, 1, 2, 2, 4 ),
 ( 0.000000000000000000, 0.2500000000000006661, 0.3750000000000009992, 0.4375000000000008882, 0.4687500000000011102, 0.5000000000000013323, 1.000000000000000000 ),
 .UNSPECIFIED. ) ;
#2158 = CARTESIAN_POINT ( 'NONE',  ( 24.55110012684054865, -25.78856419227151164, 1.431078990032156772 ) ) ;
#2159 = CARTESIAN_POINT ( 'NONE',  ( -22.46797588158592163, -80.18584073532525736, -32.25831116885107264 ) ) ;
#2160 = ORIENTED_EDGE ( 'NONE', *, *, #19790, .T. ) ;
#2161 = CARTESIAN_POINT ( 'NONE',  ( -12.72359307473547219, -94.60934249415720387, -21.54967800148987678 ) ) ;
#2162 = VERTEX_POINT ( 'NONE', #14555 ) ;
#2163 = CARTESIAN_POINT ( 'NONE',  ( 26.11960070690000180, -92.76550138599999684, 10.75202456979999965 ) ) ;
#2164 = CARTESIAN_POINT ( 'NONE',  ( 46.12332287689999788, -74.00000000000000000, -4.489694494070000097 ) ) ;
#2165 = ORIENTED_EDGE ( 'NONE', *, *, #16459, .T. ) ;
#2166 = CARTESIAN_POINT ( 'NONE',  ( 22.02882315030000271, -19.46510050329999686, -0.4636558402470000173 ) ) ;
#2167 = CARTESIAN_POINT ( 'NONE',  ( -43.20000000000000284, -63.07912966450000880, -0.1732050807570000017 ) ) ;
#2168 = EDGE_CURVE ( 'NONE', #7960, #3430, #17453, .T. ) ;
#2169 = CARTESIAN_POINT ( 'NONE',  ( 12.50568558790000040, -101.5216621940000152, -9.997196710569999922 ) ) ;
#2170 = CARTESIAN_POINT ( 'NONE',  ( -16.48967954220000109, -93.30149055190000240, -21.58637184819999888 ) ) ;
#2171 = LINE ( 'NONE', #24755, #20845 ) ;
#2172 = ORIENTED_EDGE ( 'NONE', *, *, #2522, .T. ) ;
#2173 = CARTESIAN_POINT ( 'NONE',  ( 36.22844186549999534, -74.00000000000000000, -13.75000000000000000 ) ) ;
#2174 = CARTESIAN_POINT ( 'NONE',  ( 13.26576849039999928, -100.7430069139999915, -9.799237773789998940 ) ) ;
#2175 = CARTESIAN_POINT ( 'NONE',  ( 0.000000000000000000, -17.50000000000000000, 9.000000000000000000 ) ) ;
#2176 = CARTESIAN_POINT ( 'NONE',  ( -1.283023294879999998, -101.3150694429999987, -16.20107482390000087 ) ) ;
#2177 = CARTESIAN_POINT ( 'NONE',  ( 19.97576656849999921, -38.00000000000000000, -19.97576656849999921 ) ) ;
#2178 = CARTESIAN_POINT ( 'NONE',  ( 11.27834831967279250, -72.32257210994342245, -26.96386658466257913 ) ) ;
#2179 = CARTESIAN_POINT ( 'NONE',  ( 21.46816240343896354, -36.17003871385012559, -7.279245513745156160 ) ) ;
#2180 = ORIENTED_EDGE ( 'NONE', *, *, #17837, .T. ) ;
#2181 = EDGE_CURVE ( 'NONE', #28363, #1763, #22679, .T. ) ;
#2182 = CARTESIAN_POINT ( 'NONE',  ( 20.34468230811009803, -73.94794535334492025, -32.44681540213797888 ) ) ;
#2183 = CARTESIAN_POINT ( 'NONE',  ( -24.33129403500096899, -92.53260370680638403, -18.39130825355575638 ) ) ;
#2184 = CARTESIAN_POINT ( 'NONE',  ( 7.105427357599999217E-15, -74.50000000000000000, 3.552713678799999608E-15 ) ) ;
#2185 = CARTESIAN_POINT ( 'NONE',  ( 23.70295537799999863, -94.59276292389999696, -2.111841813949999924 ) ) ;
#2186 = DIRECTION ( 'NONE',  ( 0.1988145312159089739, -0.9099612708765829616, 0.3639275582888334415 ) ) ;
#2187 = B_SPLINE_SURFACE_WITH_KNOTS ( 'NONE', 5, 5, ( 
 ( #13574, #501, #20282, #2968, #3113, #12250 ),
 ( #9497, #20880, #7328, #21024, #27590, #16631 ),
 ( #5563, #20841, #13834, #903, #759, #11633 ),
 ( #9745, #25066, #27251, #27553, #5098, #7447 ),
 ( #7732, #23169, #7290, #16599, #16305, #16158 ),
 ( #9605, #20392, #28608, #8639, #26577, #2249 ),
 ( #10812, #15329, #4719, #20160, #4870, #13300 ),
 ( #13448, #8776, #24246, #26733, #9218, #4284 ),
 ( #11092, #11255, #22508, #2552, #17689, #7064 ) ),
 .UNSPECIFIED., .F., .F., .F.,
 ( 6, 3, 6 ),
 ( 6, 6 ),
 ( 4.255758722390000039E-16, 2.251105601749999963, 5.576980223840000583 ),
 ( 0.000000000000000000, 1.000000000000000000 ),
 .UNSPECIFIED. ) ;
#2188 = APPLICATION_PROTOCOL_DEFINITION ( 'draft international standard', 'automotive_design', 1998, #16306 ) ;
#2189 = DIRECTION ( 'NONE',  ( 0.000000000000000000, -1.000000000000000000, 0.000000000000000000 ) ) ;
#2190 = CARTESIAN_POINT ( 'NONE',  ( 0.000000000000000000, -14.00000000000000000, 0.000000000000000000 ) ) ;
#2191 = CARTESIAN_POINT ( 'NONE',  ( 22.56413522780000136, -95.98460637690000397, -4.313985318640000344 ) ) ;
#2192 = ORIENTED_EDGE ( 'NONE', *, *, #27398, .F. ) ;
#2193 = CARTESIAN_POINT ( 'NONE',  ( 19.97576656849999921, -72.00000000000000000, -19.97576656849999921 ) ) ;
#2194 = DIRECTION ( 'NONE',  ( 0.000000000000000000, 1.000000000000000000, 0.000000000000000000 ) ) ;
#2195 = ORIENTED_EDGE ( 'NONE', *, *, #16351, .F. ) ;
#2196 = CARTESIAN_POINT ( 'NONE',  ( 0.000000000000000000, -101.2530993010000060, 0.000000000000000000 ) ) ;
#2197 = EDGE_CURVE ( 'NONE', #19419, #16942, #10351, .T. ) ;
#2198 = CARTESIAN_POINT ( 'NONE',  ( -6.602758024369999923, -97.12465307349999932, -19.67811079650000039 ) ) ;
#2199 = ADVANCED_FACE ( 'NONE', ( #10441 ), #18294, .T. ) ;
#2200 = CARTESIAN_POINT ( 'NONE',  ( 0.000000000000000000, -92.50000000000000000, 0.000000000000000000 ) ) ;
#2201 = CARTESIAN_POINT ( 'NONE',  ( 26.98670340789999855, -72.82938977469999031, -9.720255250690000182 ) ) ;
#2202 = CARTESIAN_POINT ( 'NONE',  ( -29.63153379720834835, -92.59735406124617896, 7.226533350539707357 ) ) ;
#2203 = CARTESIAN_POINT ( 'NONE',  ( 11.16696848683634435, -96.92941680577980890, -18.97929024651338636 ) ) ;
#2204 = VERTEX_POINT ( 'NONE', #8142 ) ;
#2205 = CARTESIAN_POINT ( 'NONE',  ( 11.56003560810000153, -93.05538536839999608, -23.65426206159999722 ) ) ;
#2206 = CARTESIAN_POINT ( 'NONE',  ( 24.43813899739999940, -34.61119146829999238, 1.434554263020000109 ) ) ;
#2207 = CARTESIAN_POINT ( 'NONE',  ( -14.57962358425329441, -80.29877500280160518, 36.44181020648760949 ) ) ;
#2208 = CARTESIAN_POINT ( 'NONE',  ( -13.24302487323487476, -92.80442066020155778, 27.47494743563386521 ) ) ;
#2209 = ORIENTED_EDGE ( 'NONE', *, *, #11403, .F. ) ;
#2210 = EDGE_CURVE ( 'NONE', #14378, #14143, #26484, .T. ) ;
#2211 = CARTESIAN_POINT ( 'NONE',  ( -40.70731707320000226, -82.25000000000000000, 7.215414233289999757 ) ) ;
#2212 = CARTESIAN_POINT ( 'NONE',  ( -15.94434063720000161, -93.10431551199999944, 24.00277150759999856 ) ) ;
#2213 = DIRECTION ( 'NONE',  ( -0.000000000000000000, 1.000000000000000000, 0.000000000000000000 ) ) ;
#2214 = VERTEX_POINT ( 'NONE', #13064 ) ;
#2215 = TOROIDAL_SURFACE ( 'NONE', #6375, 10.50000000000000000, 0.5000000000000000000 ) ;
#2216 = DIRECTION ( 'NONE',  ( -0.8775825618903722036, 0.000000000000000000, 0.4794255386042041156 ) ) ;
#2217 = CARTESIAN_POINT ( 'NONE',  ( 0.6447269329300000518, -100.1981337080000003, -16.97091045379999841 ) ) ;
#2218 = CARTESIAN_POINT ( 'NONE',  ( 11.81986579350000000, -72.00000321289999761, -27.35691362350000233 ) ) ;
#2219 = CARTESIAN_POINT ( 'NONE',  ( -12.21349012499999986, -68.60731645090001507, -24.28095208079999878 ) ) ;
#2220 = CARTESIAN_POINT ( 'NONE',  ( 23.83794015770000030, -65.05904285249999930, -7.999567420579999144 ) ) ;
#2221 = FACE_OUTER_BOUND ( 'NONE', #24886, .T. ) ;
#2222 = CARTESIAN_POINT ( 'NONE',  ( 0.000000000000000000, -19.46510050329999686, 0.000000000000000000 ) ) ;
#2223 = CIRCLE ( 'NONE', #14769, 58.54999999999999716 ) ;
#2224 = ORIENTED_EDGE ( 'NONE', *, *, #23202, .F. ) ;
#2225 = CARTESIAN_POINT ( 'NONE',  ( 28.29231644507293453, -92.71525149892931950, 11.39321545286071924 ) ) ;
#2226 = CYLINDRICAL_SURFACE ( 'NONE', #28044, 57.74999999999999289 ) ;
#2227 = CARTESIAN_POINT ( 'NONE',  ( 7.561758309989084381, -74.02518802157058531, 38.96765197712635143 ) ) ;
#2228 = ORIENTED_EDGE ( 'NONE', *, *, #26230, .F. ) ;
#2229 = CARTESIAN_POINT ( 'NONE',  ( 36.24656994149999889, -79.00000000000000000, -15.05817610060000078 ) ) ;
#2230 = CARTESIAN_POINT ( 'NONE',  ( 18.47239823780000023, -94.07620464520000780, 16.72834433539999921 ) ) ;
#2231 = AXIS2_PLACEMENT_3D ( 'NONE', #13767, #5179, #7226 ) ;
#2232 = CARTESIAN_POINT ( 'NONE',  ( 8.831064126840001194, -94.59276292389999696, -22.09756266850000017 ) ) ;
#2233 = ORIENTED_EDGE ( 'NONE', *, *, #13610, .T. ) ;
#2234 = CARTESIAN_POINT ( 'NONE',  ( 26.85898284228529675, -72.46277288053744314, -10.97019792874640842 ) ) ;
#2235 = CARTESIAN_POINT ( 'NONE',  ( -12.88998090559132237, -100.4103893717285843, -11.04208011740792372 ) ) ;
#2236 = CARTESIAN_POINT ( 'NONE',  ( 9.259752875310001130, -35.97005431750000071, -20.12202164109999813 ) ) ;
#2237 = EDGE_CURVE ( 'NONE', #7849, #25813, #19774, .T. ) ;
#2238 = CARTESIAN_POINT ( 'NONE',  ( 21.49223700067187082, -35.65578321604039758, -6.986316714794048366 ) ) ;
#2239 = ORIENTED_EDGE ( 'NONE', *, *, #14703, .T. ) ;
#2240 = ADVANCED_FACE ( 'NONE', ( #15238 ), #26346, .T. ) ;
#2241 = CARTESIAN_POINT ( 'NONE',  ( 0.000000000000000000, -20.89999999999999858, 0.000000000000000000 ) ) ;
#2242 = B_SPLINE_CURVE_WITH_KNOTS ( 'NONE', 3,
 ( #21844, #19936, #8856, #6845, #24321, #17919, #22143, #2182, #22283, #15709 ),
 .UNSPECIFIED., .F., .F.,
 ( 4, 2, 2, 2, 4 ),
 ( 0.000000000000000000, 0.2500000000000000000, 0.5000000000000000000, 0.7500000000000000000, 1.000000000000000000 ),
 .UNSPECIFIED. ) ;
#2243 = CARTESIAN_POINT ( 'NONE',  ( 21.12093416029999915, -18.50000000000000000, 0.3961283385739999829 ) ) ;
#2244 = CARTESIAN_POINT ( 'NONE',  ( -0.7858244733099999380, -98.73889367950000917, -18.62175195770000258 ) ) ;
#2245 = CARTESIAN_POINT ( 'NONE',  ( -20.54716539860091373, -92.71525149962195655, -22.54050847398934465 ) ) ;
#2246 = CIRCLE ( 'NONE', #16659, 0.5000000000000011102 ) ;
#2247 = EDGE_CURVE ( 'NONE', #22254, #14956, #14010, .T. ) ;
#2248 = CARTESIAN_POINT ( 'NONE',  ( 11.23715774159999903, -101.0848057460000007, -10.54863848640000157 ) ) ;
#2249 = CARTESIAN_POINT ( 'NONE',  ( -12.75967654059999923, -19.47871525829999939, 19.36958737249999984 ) ) ;
#2250 = CARTESIAN_POINT ( 'NONE',  ( 16.31604581177785107, -94.64681100434714267, 17.22669056164060208 ) ) ;
#2251 = EDGE_CURVE ( 'NONE', #11541, #1710, #15941, .T. ) ;
#2252 = PRODUCT ( 'Serpentine Belt Drive Pulley', 'Serpentine Belt Drive Pulley', '', ( #8864 ) ) ;
#2253 = DIRECTION ( 'NONE',  ( 0.4794255386042036160, 0.000000000000000000, 0.8775825618903723147 ) ) ;
#2254 = CARTESIAN_POINT ( 'NONE',  ( -41.75000000000000000, -65.00000000000000000, -1.587713240270000048 ) ) ;
#2255 = CARTESIAN_POINT ( 'NONE',  ( -38.41282619387080643, -65.10053925467562408, -2.881807801408382996 ) ) ;
#2256 = CARTESIAN_POINT ( 'NONE',  ( 0.000000000000000000, -20.00000000000000000, 0.000000000000000000 ) ) ;
#2257 = CARTESIAN_POINT ( 'NONE',  ( 24.06168706167060378, -93.59825775224986444, 12.30305419896300556 ) ) ;
#2258 = VERTEX_POINT ( 'NONE', #24299 ) ;
#2259 = CARTESIAN_POINT ( 'NONE',  ( 7.938154596009999509, -18.61853073680000037, -20.14564044980000190 ) ) ;
#2260 = VECTOR ( 'NONE', #22969, 999.9999999999998863 ) ;
#2261 = AXIS2_PLACEMENT_3D ( 'NONE', #18980, #20753, #19117 ) ;
#2262 = CARTESIAN_POINT ( 'NONE',  ( 7.648936895900000366, -101.0907558640000019, 13.53920073169999938 ) ) ;
#2263 = ORIENTED_EDGE ( 'NONE', *, *, #91, .T. ) ;
#2264 = CARTESIAN_POINT ( 'NONE',  ( -13.24460878530000052, -57.44036942000000323, 20.55651963289999884 ) ) ;
#2265 = DIRECTION ( 'NONE',  ( 1.000000000000000000, 0.000000000000000000, 0.000000000000000000 ) ) ;
#2266 = PRODUCT_DEFINITION_FORMATION_WITH_SPECIFIED_SOURCE ( 'ANY', '', #26438, .NOT_KNOWN. ) ;
#2267 = CARTESIAN_POINT ( 'NONE',  ( -24.56918193900000347, -94.36515553540000667, -3.609259138410000123 ) ) ;
#2268 = CARTESIAN_POINT ( 'NONE',  ( -20.56017862280000230, -57.40875702389999446, 14.85415739589999973 ) ) ;
#2269 = CARTESIAN_POINT ( 'NONE',  ( -12.17175180279999935, -57.47855601759999900, -19.93971687999999887 ) ) ;
#2270 = ORIENTED_EDGE ( 'NONE', *, *, #11763, .T. ) ;
#2271 = CARTESIAN_POINT ( 'NONE',  ( -7.229383731089999543, -73.50070240710000746, -39.23650411529999360 ) ) ;
#2272 = CARTESIAN_POINT ( 'NONE',  ( 29.82081051618066780, -74.26904473745747737, -25.43758724625505252 ) ) ;
#2273 = FACE_OUTER_BOUND ( 'NONE', #27962, .T. ) ;
#2274 = ORIENTED_EDGE ( 'NONE', *, *, #28406, .F. ) ;
#2275 = CARTESIAN_POINT ( 'NONE',  ( 0.000000000000000000, -16.50000000000000000, 0.000000000000000000 ) ) ;
#2276 = ORIENTED_EDGE ( 'NONE', *, *, #15508, .F. ) ;
#2277 = ADVANCED_FACE ( 'NONE', ( #17754 ), #24157, .F. ) ;
#2278 = AXIS2_PLACEMENT_3D ( 'NONE', #10141, #21663, #14531 ) ;
#2279 = CARTESIAN_POINT ( 'NONE',  ( 22.76317971519999972, -52.57401960329947599, 10.17780311019999040 ) ) ;
#2280 = AXIS2_PLACEMENT_3D ( 'NONE', #3506, #12364, #16326 ) ;
#2281 = CARTESIAN_POINT ( 'NONE',  ( 22.02546240290000057, -32.68478243020000207, 9.763264387630000485 ) ) ;
#2282 = FACE_OUTER_BOUND ( 'NONE', #10560, .T. ) ;
#2283 = CARTESIAN_POINT ( 'NONE',  ( 24.35204445910000004, -92.65715406910000240, -13.69691108600000184 ) ) ;
#2284 = EDGE_CURVE ( 'NONE', #11938, #13357, #2873, .T. ) ;
#2285 = CARTESIAN_POINT ( 'NONE',  ( -13.92979211509999971, -74.00000000010000178, 36.25622248599999864 ) ) ;
#2286 = CARTESIAN_POINT ( 'NONE',  ( -41.75000000000000000, -65.14977478849999670, 2.684678751729999480 ) ) ;
#2287 = CARTESIAN_POINT ( 'NONE',  ( -16.63477714874928637, -98.43098968254284387, 8.842934460737525981 ) ) ;
#2288 = ORIENTED_EDGE ( 'NONE', *, *, #12233, .T. ) ;
#2289 = DIRECTION ( 'NONE',  ( 0.09756097560976655092, 0.000000000000000000, 0.9952295494196655712 ) ) ;
#2290 = DIRECTION ( 'NONE',  ( 0.8775825618903718706, 0.000000000000000000, 0.4794255386042046152 ) ) ;
#2291 = CARTESIAN_POINT ( 'NONE',  ( -11.35954001540000036, -74.50000000000000000, 45.25000000000000000 ) ) ;
#2292 = FACE_OUTER_BOUND ( 'NONE', #7261, .T. ) ;
#2293 = CARTESIAN_POINT ( 'NONE',  ( -40.32207487330000362, -74.31847293650000097, -7.253641904939999385 ) ) ;
#2294 = ORIENTED_EDGE ( 'NONE', *, *, #16116, .F. ) ;
#2295 = CIRCLE ( 'NONE', #13919, 9.500000000000000000 ) ;
#2296 = CARTESIAN_POINT ( 'NONE',  ( 26.02259374959999860, -93.00000000000000000, -15.90831903569999994 ) ) ;
#2297 = ORIENTED_EDGE ( 'NONE', *, *, #25993, .T. ) ;
#2298 = AXIS2_PLACEMENT_3D ( 'NONE', #13070, #4488, #6535 ) ;
#2299 = CIRCLE ( 'NONE', #5564, 57.75000000000000000 ) ;
#2300 = CARTESIAN_POINT ( 'NONE',  ( -2.636840462319999912, -110.0000000000000000, -4.826704090399999814 ) ) ;
#2301 = CARTESIAN_POINT ( 'NONE',  ( -5.854055351700000465, -101.0685845459999967, 14.98984499340000198 ) ) ;
#2302 = DIRECTION ( 'NONE',  ( 0.000000000000000000, 1.000000000000000000, 0.000000000000000000 ) ) ;
#2303 = ORIENTED_EDGE ( 'NONE', *, *, #25496, .T. ) ;
#2304 = ORIENTED_EDGE ( 'NONE', *, *, #4696, .T. ) ;
#2305 = CARTESIAN_POINT ( 'NONE',  ( -26.00297803286303377, -94.00303307101484052, -2.070463084450466784 ) ) ;
#2306 = CARTESIAN_POINT ( 'NONE',  ( 20.66588605339999773, -94.54647057319999703, 13.95977755230000028 ) ) ;
#2307 = CARTESIAN_POINT ( 'NONE',  ( 46.58837163849999996, -73.69423725189999175, -3.076420046560000010 ) ) ;
#2308 = ORIENTED_EDGE ( 'NONE', *, *, #28313, .F. ) ;
#2309 = DIRECTION ( 'NONE',  ( 0.7071067811865474617, 0.000000000000000000, 0.7071067811865474617 ) ) ;
#2310 = CARTESIAN_POINT ( 'NONE',  ( -26.59500499809594487, -93.33134965528456917, -4.495659578470679207 ) ) ;
#2311 = ADVANCED_FACE ( 'NONE', ( #26636 ), #23665, .T. ) ;
#2312 = EDGE_LOOP ( 'NONE', ( #13806, #16379, #14686, #21407 ) ) ;
#2313 = CARTESIAN_POINT ( 'NONE',  ( 8.564557077759998194, -37.33500411810000230, -21.83114817979999955 ) ) ;
#2314 = CARTESIAN_POINT ( 'NONE',  ( 26.75649127029999619, -111.0000000000000000, -13.26822602019999842 ) ) ;
#2315 = ORIENTED_EDGE ( 'NONE', *, *, #7596, .T. ) ;
#2316 = AXIS2_PLACEMENT_3D ( 'NONE', #27762, #16822, #19287 ) ;
#2317 = EDGE_CURVE ( 'NONE', #11679, #11057, #9819, .T. ) ;
#2318 = CARTESIAN_POINT ( 'NONE',  ( -41.82037221943573968, -63.35319846926733334, -1.206297397086846690 ) ) ;
#2319 = CARTESIAN_POINT ( 'NONE',  ( 13.92892647020000041, -99.61736775859999682, -10.33597118630000011 ) ) ;
#2320 = CARTESIAN_POINT ( 'NONE',  ( -39.92836808239999868, -74.14144860030000928, 7.283536107469999799 ) ) ;
#2321 = CARTESIAN_POINT ( 'NONE',  ( -13.16183723299999997, -70.12921532840000793, -24.09258145020000086 ) ) ;
#2322 = CARTESIAN_POINT ( 'NONE',  ( -5.701030053896644745, -98.22875432232922321, -19.45415947712940863 ) ) ;
#2323 = FACE_OUTER_BOUND ( 'NONE', #5466, .T. ) ;
#2324 = DIRECTION ( 'NONE',  ( 0.000000000000000000, 1.000000000000000000, 0.000000000000000000 ) ) ;
#2325 = CARTESIAN_POINT ( 'NONE',  ( 7.435977656837697403, -74.13942000216081851, -39.48500436385279500 ) ) ;
#2326 = EDGE_LOOP ( 'NONE', ( #7698, #1566, #991, #23620, #5841, #13146 ) ) ;
#2327 = DIRECTION ( 'NONE',  ( 1.000000000000000000, 0.000000000000000000, 0.000000000000000000 ) ) ;
#2328 = DIRECTION ( 'NONE',  ( -0.000000000000000000, 1.000000000000000000, 0.000000000000000000 ) ) ;
#2329 = CARTESIAN_POINT ( 'NONE',  ( 0.000000000000000000, -92.50000000000000000, 0.000000000000000000 ) ) ;
#2330 = FACE_OUTER_BOUND ( 'NONE', #5988, .T. ) ;
#2331 = DIRECTION ( 'NONE',  ( 0.9704142011833033488, 0.000000000000000000, -0.2414462220490755373 ) ) ;
#2332 = CARTESIAN_POINT ( 'NONE',  ( -14.66822218795144295, -101.0767042429054641, 4.761812676672435352 ) ) ;
#2333 = EDGE_CURVE ( 'NONE', #15756, #5488, #26795, .T. ) ;
#2334 = PRODUCT_CONTEXT ( 'NONE', #18916, 'mechanical' ) ;
#2335 = CARTESIAN_POINT ( 'NONE',  ( 23.90606521969999676, -57.45864773929999814, 0.8443132633689999222 ) ) ;
#2336 = CIRCLE ( 'NONE', #7484, 15.19391340349999986 ) ;
#2337 = CARTESIAN_POINT ( 'NONE',  ( -11.35954001540000036, -80.00000000000000000, 46.75000000000000000 ) ) ;
#2338 = TOROIDAL_SURFACE ( 'NONE', #13961, 3.750000000000000000, 1.000000000000000000 ) ;
#2339 = EDGE_LOOP ( 'NONE', ( #24017, #18856, #23774, #28014 ) ) ;
#2340 = DIRECTION ( 'NONE',  ( 0.000000000000000000, 1.000000000000000000, 0.000000000000000000 ) ) ;
#2341 = CARTESIAN_POINT ( 'NONE',  ( 19.21071510300000185, -98.24302442670000346, -0.5565603496329999400 ) ) ;
#2342 = ORIENTED_EDGE ( 'NONE', *, *, #23406, .F. ) ;
#2343 = CARTESIAN_POINT ( 'NONE',  ( -13.15709823100000087, -49.83805748250000534, 20.35711383789999829 ) ) ;
#2344 = ORIENTED_EDGE ( 'NONE', *, *, #10399, .F. ) ;
#2345 = CARTESIAN_POINT ( 'NONE',  ( 2.220446049249999745E-14, -15.00000000000000000, -50.00000000000000000 ) ) ;
#2346 = EDGE_CURVE ( 'NONE', #10898, #19704, #19179, .T. ) ;
#2347 = ADVANCED_FACE ( 'NONE', ( #11160 ), #18185, .T. ) ;
#2348 = CARTESIAN_POINT ( 'NONE',  ( -6.605171516649999575, -97.48426834619999681, -20.14546412150000165 ) ) ;
#2349 = CARTESIAN_POINT ( 'NONE',  ( 7.904069757880235692, -94.04667188340653183, -24.76727834805952710 ) ) ;
#2350 = CARTESIAN_POINT ( 'NONE',  ( -24.06374496360000137, -94.22763312380000400, -3.197736329870000116 ) ) ;
#2351 = CARTESIAN_POINT ( 'NONE',  ( -17.98004918629999693, -98.73884893519999650, 4.909944750820000259 ) ) ;
#2352 = CARTESIAN_POINT ( 'NONE',  ( -29.57839868347437218, -92.54938211478190624, 7.441512166611892631 ) ) ;
#2353 = CARTESIAN_POINT ( 'NONE',  ( 47.19173749819621122, -79.33634930001392149, -1.160608118433608560 ) ) ;
#2354 = VERTEX_POINT ( 'NONE', #4785 ) ;
#2355 = FACE_OUTER_BOUND ( 'NONE', #19327, .T. ) ;
#2356 = CARTESIAN_POINT ( 'NONE',  ( -20.29409717112922706, -60.89354426525722630, 12.37746592674120905 ) ) ;
#2357 = CARTESIAN_POINT ( 'NONE',  ( -12.78325572749593064, -92.58608763741581527, 27.69184823660511796 ) ) ;
#2358 = ORIENTED_EDGE ( 'NONE', *, *, #19305, .T. ) ;
#2359 = AXIS2_PLACEMENT_3D ( 'NONE', #13477, #22829, #2870 ) ;
#2360 = CARTESIAN_POINT ( 'NONE',  ( -11.46863496920000003, -57.40875702469999453, -22.62382260909999943 ) ) ;
#2361 = LINE ( 'NONE', #11957, #7893 ) ;
#2362 = PLANE ( 'NONE',  #14051 ) ;
#2363 = ORIENTED_EDGE ( 'NONE', *, *, #27219, .F. ) ;
#2364 = CIRCLE ( 'NONE', #21427, 57.75000000000000000 ) ;
#2365 = CARTESIAN_POINT ( 'NONE',  ( 27.04142406090000250, -68.97505732880000551, 1.205035742480000005 ) ) ;
#2366 = AXIS2_PLACEMENT_3D ( 'NONE', #17586, #15526, #8822 ) ;
#2367 = CARTESIAN_POINT ( 'NONE',  ( 0.3813996810959999761, -101.2251655520000071, -16.21856860389999966 ) ) ;
#2368 = DIRECTION ( 'NONE',  ( 0.6184463001828860440, 0.000000000000000000, 0.7858270635388550085 ) ) ;
#2369 = CARTESIAN_POINT ( 'NONE',  ( -46.75000000000000000, -69.50000000000000000, -1.262878690509999918E-15 ) ) ;
#2370 = CARTESIAN_POINT ( 'NONE',  ( 23.84797911320000097, -63.15653191699999525, -9.592766500679999808 ) ) ;
#2371 = EDGE_CURVE ( 'NONE', #6736, #4998, #4926, .T. ) ;
#2372 = DIRECTION ( 'NONE',  ( 0.000000000000000000, 1.000000000000000000, 0.000000000000000000 ) ) ;
#2373 = DIRECTION ( 'NONE',  ( 0.9763395129702659991, 0.000000000000000000, -0.2162432783070585007 ) ) ;
#2374 = DIRECTION ( 'NONE',  ( 0.000000000000000000, 1.000000000000000000, 0.000000000000000000 ) ) ;
#2375 = EDGE_LOOP ( 'NONE', ( #4227, #7103, #488 ) ) ;
#2376 = CARTESIAN_POINT ( 'NONE',  ( 28.56828035858709924, -92.92035259817281201, 10.68546831372889550 ) ) ;
#2377 = CARTESIAN_POINT ( 'NONE',  ( -26.69293917519999937, -19.09689110869999951, -48.86109741659999628 ) ) ;
#2378 = CARTESIAN_POINT ( 'NONE',  ( 8.071146758930000331, -100.8816832290000036, 13.57632735329999996 ) ) ;
#2379 = ORIENTED_EDGE ( 'NONE', *, *, #8825, .F. ) ;
#2380 = CIRCLE ( 'NONE', #3760, 38.75000000000000000 ) ;
#2381 = CARTESIAN_POINT ( 'NONE',  ( 23.28812738402805138, -92.52249206702278173, -19.69551804736990874 ) ) ;
#2382 = CARTESIAN_POINT ( 'NONE',  ( 24.73953705929999813, -92.49999846069999876, 14.89634059649999998 ) ) ;
#2383 = TOROIDAL_SURFACE ( 'NONE', #10709, 55.85192378860000417, 0.3499999999999999778 ) ;
#2384 = CIRCLE ( 'NONE', #27960, 55.67692378859999991 ) ;
#2385 = CARTESIAN_POINT ( 'NONE',  ( 23.50367701526724673, -19.48459430185724273, 1.423420176684405902 ) ) ;
#2386 = CARTESIAN_POINT ( 'NONE',  ( -7.315719113890000180, -101.0640712160000021, 14.34151901279999919 ) ) ;
#2387 = ORIENTED_EDGE ( 'NONE', *, *, #2852, .F. ) ;
#2388 = DIRECTION ( 'NONE',  ( 0.2414462220490755373, 0.000000000000000000, -0.9704142011833033488 ) ) ;
#2389 = VECTOR ( 'NONE', #15810, 1000.000000000000000 ) ;
#2390 = EDGE_LOOP ( 'NONE', ( #10843, #12813 ) ) ;
#2391 = CARTESIAN_POINT ( 'NONE',  ( 8.690400270730000543, -36.30003840290000028, -21.06640817119999554 ) ) ;
#2392 = CARTESIAN_POINT ( 'NONE',  ( 21.55117138126461995, -36.19847887270072562, -6.864724801166914858 ) ) ;
#2393 = CARTESIAN_POINT ( 'NONE',  ( 8.257819997060000361, -98.83157882129999905, 16.36072119760000021 ) ) ;
#2394 = DIRECTION ( 'NONE',  ( 1.000000000000000000, 0.000000000000000000, 0.000000000000000000 ) ) ;
#2395 = CARTESIAN_POINT ( 'NONE',  ( -2.330049844439999962, -97.93128678269999909, -19.86603722859999976 ) ) ;
#2396 = CARTESIAN_POINT ( 'NONE',  ( 0.000000000000000000, -23.00000000000000000, 0.000000000000000000 ) ) ;
#2397 = VERTEX_POINT ( 'NONE', #26936 ) ;
#2398 = DIRECTION ( 'NONE',  ( 0.000000000000000000, 1.000000000000000000, 0.000000000000000000 ) ) ;
#2399 = CARTESIAN_POINT ( 'NONE',  ( -18.67420757599678893, -98.28141828938548485, -7.711871447694185200 ) ) ;
#2400 = CARTESIAN_POINT ( 'NONE',  ( 6.850353625200000351, -36.56979901409999911, -21.56931447779999900 ) ) ;
#2401 = CARTESIAN_POINT ( 'NONE',  ( 36.34915583725175026, -75.00000019643333360, -14.88857262638677703 ) ) ;
#2402 = CARTESIAN_POINT ( 'NONE',  ( 25.87390537659780776, -62.05304730950737024, 1.417947247737919358 ) ) ;
#2403 = DIRECTION ( 'NONE',  ( 1.000000000000000000, 0.000000000000000000, 0.000000000000000000 ) ) ;
#2404 = DIRECTION ( 'NONE',  ( 0.4794255386042040601, 0.000000000000000000, 0.8775825618903720926 ) ) ;
#2405 = CIRCLE ( 'NONE', #6097, 3.000000000000000888 ) ;
#2406 = ORIENTED_EDGE ( 'NONE', *, *, #16021, .T. ) ;
#2407 = CIRCLE ( 'NONE', #24256, 30.50381168839999901 ) ;
#2408 = CARTESIAN_POINT ( 'NONE',  ( -32.20769385759999892, -80.50000045429999318, -22.43272066369999962 ) ) ;
#2409 = CIRCLE ( 'NONE', #13490, 5.000000000000000888 ) ;
#2410 = EDGE_CURVE ( 'NONE', #5413, #723, #6976, .T. ) ;
#2411 = CARTESIAN_POINT ( 'NONE',  ( 7.962341111249999770, -101.1573270909999991, 13.90182050930000024 ) ) ;
#2412 = EDGE_CURVE ( 'NONE', #19945, #16942, #21521, .T. ) ;
#2413 = EDGE_LOOP ( 'NONE', ( #27282, #9515, #27107, #1037 ) ) ;
#2414 = CARTESIAN_POINT ( 'NONE',  ( -13.55408830789999897, -67.56935268729999677, 22.52790492979999826 ) ) ;
#2415 = CARTESIAN_POINT ( 'NONE',  ( -38.25000000000000000, -63.30468293320000583, -1.587713240270000048 ) ) ;
#2416 = FACE_OUTER_BOUND ( 'NONE', #12610, .T. ) ;
#2417 = EDGE_CURVE ( 'NONE', #8384, #18741, #27081, .T. ) ;
#2418 = DIRECTION ( 'NONE',  ( 0.000000000000000000, 1.000000000000000000, 0.000000000000000000 ) ) ;
#2419 = DIRECTION ( 'NONE',  ( 1.000000000000000000, 0.000000000000000000, 0.000000000000000000 ) ) ;
#2420 = ADVANCED_FACE ( 'NONE', ( #9284 ), #18720, .F. ) ;
#2421 = CIRCLE ( 'NONE', #22430, 32.39999999999999858 ) ;
#2422 = CARTESIAN_POINT ( 'NONE',  ( -11.31871641743052415, -57.41946977428668930, -22.35641880394745939 ) ) ;
#2423 = ORIENTED_EDGE ( 'NONE', *, *, #27873, .F. ) ;
#2424 = CARTESIAN_POINT ( 'NONE',  ( -7.196178079599999222, -73.81415926540000783, -38.70548889989999708 ) ) ;
#2425 = CARTESIAN_POINT ( 'NONE',  ( 30.59674585478018116, -74.18273825083886663, -24.40299353443661445 ) ) ;
#2426 = FACE_OUTER_BOUND ( 'NONE', #21411, .T. ) ;
#2427 = ORIENTED_EDGE ( 'NONE', *, *, #12208, .T. ) ;
#2428 = VECTOR ( 'NONE', #3553, 1000.000000000000000 ) ;
#2429 = CARTESIAN_POINT ( 'NONE',  ( -15.42363691649999957, -19.50000000000000000, 22.84488648889999851 ) ) ;
#2430 = ORIENTED_EDGE ( 'NONE', *, *, #15609, .T. ) ;
#2431 = DIRECTION ( 'NONE',  ( 0.4751828347227322613, 0.1327433628319252545, 0.8698163445285104212 ) ) ;
#2432 = CARTESIAN_POINT ( 'NONE',  ( 15.53338745080000116, -84.75000000000000000, 28.43367500519999780 ) ) ;
#2433 = CARTESIAN_POINT ( 'NONE',  ( 22.34015708469999950, -32.67314204010000367, 9.890958026079999854 ) ) ;
#2434 = FACE_OUTER_BOUND ( 'NONE', #10940, .T. ) ;
#2435 = CARTESIAN_POINT ( 'NONE',  ( -7.248366623730185587, -73.88016183361062872, -39.84605369631500338 ) ) ;
#2436 = CARTESIAN_POINT ( 'NONE',  ( 22.14322190709999916, -64.99357404969998697, 11.84671812930000101 ) ) ;
#2437 = CARTESIAN_POINT ( 'NONE',  ( 9.855634484279999441, -64.48636388919999263, -24.31831199750000039 ) ) ;
#2438 = CARTESIAN_POINT ( 'NONE',  ( 14.05983683630000058, -99.53431242750001218, -10.27464373080000115 ) ) ;
#2439 = B_SPLINE_SURFACE_WITH_KNOTS ( 'NONE', 5, 5, ( 
 ( #4421, #4123, #23560, #24238, #8627, #22058, #7835, #3594, #7972 ),
 ( #21908, #16716, #6310, #2106, #10653, #17681, #16862, #26569, #24086 ),
 ( #10129, #15469, #1162, #18914, #25752, #21106, #9999, #27794, #5642 ),
 ( #14521, #23424, #3463, #19712, #12329, #28599, #21237, #19050, #5777 ),
 ( #14665, #21370, #1426, #19570, #28457, #8493, #17393, #20295, #22196 ),
 ( #18414, #24823, #2541, #4861, #2391, #22498, #363, #13742, #15917 ),
 ( #27011, #24522, #19998, #9069, #24966, #20151, #22788, #27303, #22343 ),
 ( #13292, #11082, #11689, #11394, #71, #4558, #24674, #20447, #25119 ),
 ( #13886, #7341, #15622, #17826, #20600, #11246, #7054, #7198, #6904 ),
 ( #8917, #2236, #26721, #16207, #4710, #15768, #6760, #13437, #26865 ),
 ( #222, #17971, #9208, #517, #16064, #13590, #4996, #18118, #22642 ),
 ( #9512, #2681, #2827, #659, #11538, #9364, #18265, #27158, #21303 ) ),
 .UNSPECIFIED., .F., .F., .F.,
 ( 6, 3, 3, 6 ),
 ( 6, 3, 6 ),
 ( 8.754352264609998713, 10.05054279850000043, 10.42202991689999969, 11.17956741670000120 ),
 ( 0.000000000000000000, 1.000000000000000000, 2.000000000000000000 ),
 .UNSPECIFIED. ) ;
#2440 = ORIENTED_EDGE ( 'NONE', *, *, #13450, .F. ) ;
#2441 = DIRECTION ( 'NONE',  ( 1.000000000000000000, 0.000000000000000000, 1.224606353820001308E-16 ) ) ;
#2442 = CARTESIAN_POINT ( 'NONE',  ( 27.35691632010000163, -72.00000328939999861, -11.81987169600000165 ) ) ;
#2443 = CARTESIAN_POINT ( 'NONE',  ( -12.82129959709999945, -100.1459902240000019, -11.09448884939999935 ) ) ;
#2444 = CARTESIAN_POINT ( 'NONE',  ( 40.00000000000000000, -82.25000000000000000, 0.000000000000000000 ) ) ;
#2445 = CARTESIAN_POINT ( 'NONE',  ( 22.76364019028259023, -61.39309059898780419, -7.242868441357485310 ) ) ;
#2446 = ORIENTED_EDGE ( 'NONE', *, *, #3753, .F. ) ;
#2447 = B_SPLINE_CURVE_WITH_KNOTS ( 'NONE', 3,
 ( #11671, #20582, #16192, #7483, #16345, #25253, #15902, #24809, #4846, #13725, #20427, #18247, #7183, #16050, #24952, #5963, #9920, #12248, #27990, #7764, #10459, #14445, #21285, #16914, #14578, #5836, #3797, #25667, #25810, #19377, #19102, #21160 ),
 .UNSPECIFIED., .F., .F.,
 ( 4, 2, 2, 1, 1, 2, 2, 2, 1, 1, 1, 2, 2, 2, 1, 1, 1, 2, 2, 4 ),
 ( 0.000000000000000000, 0.1250000000000721367, 0.1875000000001230960, 0.2187500000001387501, 0.2343750000001453282, 0.2421875000001490752, 0.2500000000001527667, 0.3750000000000960343, 0.4375000000000670575, 0.4687500000000578981, 0.4843750000000533462, 0.4921875000000504596, 0.5000000000000475175, 0.6250000000000074385, 0.6874999999999900080, 0.7187499999999837907, 0.7343749999999824585, 0.7421874999999835687, 0.7499999999999845679, 1.000000000000000000 ),
 .UNSPECIFIED. ) ;
#2448 = PLANE ( 'NONE',  #27941 ) ;
#2449 = ORIENTED_EDGE ( 'NONE', *, *, #24039, .F. ) ;
#2450 = AXIS2_PLACEMENT_3D ( 'NONE', #8942, #11416, #6635 ) ;
#2451 = B_SPLINE_CURVE_WITH_KNOTS ( 'NONE', 5,
 ( #16029, #24934, #4963, #22751, #20558, #627 ),
 .UNSPECIFIED., .F., .F.,
 ( 6, 6 ),
 ( 0.000000000000000000, 1.000000000000000000 ),
 .UNSPECIFIED. ) ;
#2452 = ADVANCED_FACE ( 'NONE', ( #2610 ), #3361, .F. ) ;
#2453 = CARTESIAN_POINT ( 'NONE',  ( -0.1868532263790000092, -111.0000000000000000, -16.79896085689999907 ) ) ;
#2454 = CARTESIAN_POINT ( 'NONE',  ( -7.325370793560000315, -19.50000000000000000, -24.94672208400000102 ) ) ;
#2455 = CARTESIAN_POINT ( 'NONE',  ( 20.06309763089999620, -36.00000000000000000, -9.476129751679998492 ) ) ;
#2456 = CARTESIAN_POINT ( 'NONE',  ( 12.03711594220000158, -93.00000311470000725, 27.59851862110000198 ) ) ;
#2457 = ADVANCED_FACE ( 'NONE', ( #3186 ), #1122, .T. ) ;
#2458 = VERTEX_POINT ( 'NONE', #11907 ) ;
#2459 = ORIENTED_EDGE ( 'NONE', *, *, #8543, .T. ) ;
#2460 = CARTESIAN_POINT ( 'NONE',  ( -21.35786096709999882, -65.07443093669999712, 13.27975207949999970 ) ) ;
#2461 = CARTESIAN_POINT ( 'NONE',  ( 21.96855572870000017, -93.67384841979999521, 13.21298988309999878 ) ) ;
#2462 = CARTESIAN_POINT ( 'NONE',  ( -14.79537251110000007, -100.9197086940000077, 5.022279785309999411 ) ) ;
#2463 = ORIENTED_EDGE ( 'NONE', *, *, #9703, .F. ) ;
#2464 = CARTESIAN_POINT ( 'NONE',  ( 31.00000000000000000, 0.000000000000000000, 4.500000000000000000 ) ) ;
#2465 = CARTESIAN_POINT ( 'NONE',  ( -22.00249006139999963, -79.69117347819999964, -32.67527200749999849 ) ) ;
#2466 = VECTOR ( 'NONE', #1221, 1000.000000000000000 ) ;
#2467 = CARTESIAN_POINT ( 'NONE',  ( 11.86373224459999776, -101.2530993010000060, -9.493548918760000177 ) ) ;
#2468 = CARTESIAN_POINT ( 'NONE',  ( -12.50340864429999854, -94.22763312360000043, -20.80754938939999832 ) ) ;
#2469 = TOROIDAL_SURFACE ( 'NONE', #20611, 2.500000000000000000, 0.5000000000000000000 ) ;
#2470 = CARTESIAN_POINT ( 'NONE',  ( -23.61875799909552143, -94.52293547164087784, -3.856443778712968395 ) ) ;
#2471 = ORIENTED_EDGE ( 'NONE', *, *, #13476, .F. ) ;
#2472 = LINE ( 'NONE', #18046, #22324 ) ;
#2473 = CARTESIAN_POINT ( 'NONE',  ( 14.01198241910000064, -99.55609327400000552, -10.29247172640000052 ) ) ;
#2474 = CARTESIAN_POINT ( 'NONE',  ( -39.04179453189999549, -73.95640471630001400, 7.432602092579998931 ) ) ;
#2475 = CARTESIAN_POINT ( 'NONE',  ( -22.22906645670000003, -74.50000000000000000, -32.83566817450000030 ) ) ;
#2476 = CARTESIAN_POINT ( 'NONE',  ( 0.000000000000000000, -92.50000000000000000, 0.000000000000000000 ) ) ;
#2477 = FACE_OUTER_BOUND ( 'NONE', #6147, .T. ) ;
#2478 = CARTESIAN_POINT ( 'NONE',  ( -7.557074492643517161, -73.99988188839131453, 38.78621575433889035 ) ) ;
#2479 = EDGE_LOOP ( 'NONE', ( #4183, #10396, #25072, #3925 ) ) ;
#2480 = CARTESIAN_POINT ( 'NONE',  ( -7.333308059120000166, -94.59276479689999917, -22.63874320469999901 ) ) ;
#2481 = FACE_OUTER_BOUND ( 'NONE', #14830, .T. ) ;
#2482 = CARTESIAN_POINT ( 'NONE',  ( 8.508194257199999555, -34.61672919229999934, -20.76917589150000154 ) ) ;
#2483 = CARTESIAN_POINT ( 'NONE',  ( -23.92451332507025441, -92.71619979444980686, -18.91739093709076158 ) ) ;
#2484 = EDGE_CURVE ( 'NONE', #19473, #26756, #19205, .T. ) ;
#2485 = LINE ( 'NONE', #11341, #28396 ) ;
#2486 = CARTESIAN_POINT ( 'NONE',  ( 20.34628061889999984, -52.63293862049999916, 11.13082833170000008 ) ) ;
#2487 = DIRECTION ( 'NONE',  ( 0.4794255386042040601, 0.000000000000000000, 0.8775825618903720926 ) ) ;
#2488 = EDGE_CURVE ( 'NONE', #22088, #22416, #24822, .T. ) ;
#2489 = DIRECTION ( 'NONE',  ( 0.000000000000000000, 0.000000000000000000, 1.000000000000000000 ) ) ;
#2490 = CIRCLE ( 'NONE', #13571, 61.35000000000000142 ) ;
#2491 = AXIS2_PLACEMENT_3D ( 'NONE', #18706, #27860, #8044 ) ;
#2492 = CARTESIAN_POINT ( 'NONE',  ( 3.551183598479999925E-15, -73.00000000000000000, -32.75000000000000000 ) ) ;
#2493 = EDGE_CURVE ( 'NONE', #14660, #16936, #15966, .T. ) ;
#2494 = ORIENTED_EDGE ( 'NONE', *, *, #25919, .T. ) ;
#2495 = CARTESIAN_POINT ( 'NONE',  ( 17.82341631479999933, -99.75094652120000660, 1.185189151289999909 ) ) ;
#2496 = EDGE_LOOP ( 'NONE', ( #17005, #22893, #7729, #27076 ) ) ;
#2497 = CARTESIAN_POINT ( 'NONE',  ( -11.20604483669999851, -42.27289973529999401, 19.89334194550000134 ) ) ;
#2498 = ORIENTED_EDGE ( 'NONE', *, *, #27253, .T. ) ;
#2499 = CARTESIAN_POINT ( 'NONE',  ( 8.607507029887250027, -36.72040101226378539, -21.55953479827181951 ) ) ;
#2500 = AXIS2_PLACEMENT_3D ( 'NONE', #304, #150, #9143 ) ;
#2501 = CARTESIAN_POINT ( 'NONE',  ( 7.472221251747646065, -93.86130746277306969, -25.29698305997012042 ) ) ;
#2502 = CARTESIAN_POINT ( 'NONE',  ( 9.698193454340000130, -36.00000000010000178, -20.58262106160000116 ) ) ;
#2503 = CARTESIAN_POINT ( 'NONE',  ( 26.13446004556505287, -70.56829302196123876, -9.039107915225594425 ) ) ;
#2504 = CARTESIAN_POINT ( 'NONE',  ( -10.43683906909999948, -19.16174980609999778, -20.01792584879999737 ) ) ;
#2505 = CARTESIAN_POINT ( 'NONE',  ( 21.59423340250210543, -37.77125957295557868, -8.020740188427190276 ) ) ;
#2506 = EDGE_LOOP ( 'NONE', ( #7714, #6725, #4166, #19968 ) ) ;
#2507 = DIRECTION ( 'NONE',  ( 0.000000000000000000, -1.000000000000000000, 0.000000000000000000 ) ) ;
#2508 = CARTESIAN_POINT ( 'NONE',  ( -38.25000000000000000, -65.65254685980617921, -1.544478930961744156 ) ) ;
#2509 = CARTESIAN_POINT ( 'NONE',  ( -31.89935321680000158, -74.00000000000000000, -21.99985828019999801 ) ) ;
#2510 = VERTEX_POINT ( 'NONE', #25751 ) ;
#2511 = CIRCLE ( 'NONE', #27652, 4.750000000000000888 ) ;
#2512 = DIRECTION ( 'NONE',  ( -5.788992577199999305E-17, 0.000000000000000000, 1.000000000000000000 ) ) ;
#2513 = CARTESIAN_POINT ( 'NONE',  ( -17.01429261839999896, -93.08199881499999151, 21.72620143179999985 ) ) ;
#2514 = DIRECTION ( 'NONE',  ( 0.000000000000000000, -1.000000000000000000, 0.000000000000000000 ) ) ;
#2515 = ORIENTED_EDGE ( 'NONE', *, *, #16076, .T. ) ;
#2516 = CARTESIAN_POINT ( 'NONE',  ( -17.64295153049999954, -98.69230457299998704, 8.917116780599998904 ) ) ;
#2517 = CARTESIAN_POINT ( 'NONE',  ( -12.65195851542230265, -101.1586404113024429, -9.188934965808664757 ) ) ;
#2518 = CARTESIAN_POINT ( 'NONE',  ( 0.6630435622020000030, -100.4071172650000108, -16.77778116909999895 ) ) ;
#2519 = CARTESIAN_POINT ( 'NONE',  ( 22.79517987939305002, -74.07354942525847719, -31.66438262344599508 ) ) ;
#2520 = CARTESIAN_POINT ( 'NONE',  ( 0.000000000000000000, -10.50000000000000000, 0.000000000000000000 ) ) ;
#2521 = CARTESIAN_POINT ( 'NONE',  ( -11.18016183240000139, -57.44036992910000095, -21.74842400150000188 ) ) ;
#2522 = EDGE_CURVE ( 'NONE', #1018, #22701, #8968, .T. ) ;
#2523 = CIRCLE ( 'NONE', #19242, 0.5000000000000004441 ) ;
#2524 = CARTESIAN_POINT ( 'NONE',  ( 7.157200201290000230, -99.88067631459999518, 15.79636883619999921 ) ) ;
#2525 = AXIS2_PLACEMENT_3D ( 'NONE', #24621, #4504, #24469 ) ;
#2526 = B_SPLINE_CURVE_WITH_KNOTS ( 'NONE', 2,
 ( #25786, #8006, #12910 ),
 .UNSPECIFIED., .F., .F.,
 ( 3, 3 ),
 ( 0.000000000000000000, 1.000000000000000000 ),
 .UNSPECIFIED. ) ;
#2527 = CARTESIAN_POINT ( 'NONE',  ( 0.000000000000000000, -90.50000000000000000, 30.50000000000000000 ) ) ;
#2528 = EDGE_CURVE ( 'NONE', #11029, #12945, #19681, .T. ) ;
#2529 = ORIENTED_EDGE ( 'NONE', *, *, #27466, .F. ) ;
#2530 = CARTESIAN_POINT ( 'NONE',  ( 27.95526608003522639, -92.54383083955177369, 12.19645322206126359 ) ) ;
#2531 = CARTESIAN_POINT ( 'NONE',  ( 23.17395180239999775, -18.50000000000000000, 2.380615958829999990 ) ) ;
#2532 = DIRECTION ( 'NONE',  ( 0.000000000000000000, 1.000000000000000000, 0.000000000000000000 ) ) ;
#2533 = DIRECTION ( 'NONE',  ( 0.7071067811865474617, 0.000000000000000000, 0.7071067811865474617 ) ) ;
#2534 = CARTESIAN_POINT ( 'NONE',  ( -40.50000000000000000, -63.00000000000000000, -2.309401076760000393 ) ) ;
#2535 = CARTESIAN_POINT ( 'NONE',  ( 22.10171175959985845, -19.46474104946126005, 0.03556608548572790657 ) ) ;
#2536 = CARTESIAN_POINT ( 'NONE',  ( -7.296432207050000507, -100.9364576079999978, 14.18420974400000034 ) ) ;
#2537 = ORIENTED_EDGE ( 'NONE', *, *, #16918, .T. ) ;
#2538 = FACE_OUTER_BOUND ( 'NONE', #3298, .T. ) ;
#2539 = CARTESIAN_POINT ( 'NONE',  ( -12.45118061580227042, -101.3846248974119248, -10.37016303958056263 ) ) ;
#2540 =( REPRESENTATION_RELATIONSHIP ('NONE','NONE', #26008, #2018 ) REPRESENTATION_RELATIONSHIP_WITH_TRANSFORMATION ( #25065 )SHAPE_REPRESENTATION_RELATIONSHIP( ) );
#2541 = CARTESIAN_POINT ( 'NONE',  ( 9.085163553980001083, -35.93116987310000354, -20.23957076829999835 ) ) ;
#2542 = CARTESIAN_POINT ( 'NONE',  ( 8.280691199402831160, -19.47200836853050632, -20.32438904306839333 ) ) ;
#2543 = ORIENTED_EDGE ( 'NONE', *, *, #21487, .F. ) ;
#2544 = LINE ( 'NONE', #9072, #14632 ) ;
#2545 = EDGE_CURVE ( 'NONE', #20314, #20323, #27932, .T. ) ;
#2546 = DIRECTION ( 'NONE',  ( 0.000000000000000000, -1.000000000000000000, 0.000000000000000000 ) ) ;
#2547 = CARTESIAN_POINT ( 'NONE',  ( 0.4820043924829999771, -99.73367660430000115, -17.30272240089999869 ) ) ;
#2548 = VECTOR ( 'NONE', #15134, 1000.000000000000000 ) ;
#2549 = FACE_BOUND ( 'NONE', #1042, .T. ) ;
#2550 = EDGE_LOOP ( 'NONE', ( #24878, #21852, #15857, #8556 ) ) ;
#2551 = FACE_OUTER_BOUND ( 'NONE', #3271, .T. ) ;
#2552 = CARTESIAN_POINT ( 'NONE',  ( -13.57909544900000043, -18.87168146910000033, 20.35758746379999806 ) ) ;
#2553 = CARTESIAN_POINT ( 'NONE',  ( 9.119802927630001221, -98.28914429610000525, 16.69368728350000097 ) ) ;
#2554 = CARTESIAN_POINT ( 'NONE',  ( -38.55000000000000426, -63.07912966450000880, -2.857883832489999776 ) ) ;
#2555 = FACE_OUTER_BOUND ( 'NONE', #3581, .T. ) ;
#2556 = AXIS2_PLACEMENT_3D ( 'NONE', #19032, #25321, #16843 ) ;
#2557 = PLANE ( 'NONE',  #24883 ) ;
#2558 = DIRECTION ( 'NONE',  ( 1.000000000000000000, 0.000000000000000000, 9.436895709310000674E-16 ) ) ;
#2559 = ORIENTED_EDGE ( 'NONE', *, *, #23576, .T. ) ;
#2560 = DIRECTION ( 'NONE',  ( 0.000000000000000000, 1.000000000000000000, 0.000000000000000000 ) ) ;
#2561 = EDGE_CURVE ( 'NONE', #27080, #7740, #21105, .T. ) ;
#2562 = CIRCLE ( 'NONE', #18847, 3.750000000000000000 ) ;
#2563 = CARTESIAN_POINT ( 'NONE',  ( 8.069590842209999337, -101.0685850230000113, 13.92289867959999938 ) ) ;
#2564 = ORIENTED_EDGE ( 'NONE', *, *, #12606, .T. ) ;
#2565 = CARTESIAN_POINT ( 'NONE',  ( 0.000000000000000000, -20.89999999999999858, 0.000000000000000000 ) ) ;
#2566 = CARTESIAN_POINT ( 'NONE',  ( -11.20999108620000051, -59.03959220630000004, 20.55796391140000168 ) ) ;
#2567 = CARTESIAN_POINT ( 'NONE',  ( -10.37698671729999766, -80.00000000000000000, 42.77322331710000469 ) ) ;
#2568 = TOROIDAL_SURFACE ( 'NONE', #7697, 29.91857981989999971, 10.00000000000000000 ) ;
#2569 = CARTESIAN_POINT ( 'NONE',  ( -40.00000000000000000, -84.50000000000000000, 6.883382752679998869E-16 ) ) ;
#2570 = CARTESIAN_POINT ( 'NONE',  ( 20.68428921539999976, -36.00000000000000000, -9.307966650710000067 ) ) ;
#2571 = CARTESIAN_POINT ( 'NONE',  ( -6.306066779869998999E-15, -74.00000000000000000, -2.597921877619999821E-15 ) ) ;
#2572 = CYLINDRICAL_SURFACE ( 'NONE', #22474, 1.000000000000000888 ) ;
#2573 = ORIENTED_EDGE ( 'NONE', *, *, #17303, .T. ) ;
#2574 = CARTESIAN_POINT ( 'NONE',  ( -7.215414233289999757, -74.50000000000000000, -40.70731707320000226 ) ) ;
#2575 = CARTESIAN_POINT ( 'NONE',  ( -40.50000000000000000, -64.47022873560000278, -2.309401076760000393 ) ) ;
#2576 = CARTESIAN_POINT ( 'NONE',  ( -17.54973872020000059, -98.24302442859999474, -7.833773352749999752 ) ) ;
#2577 = EDGE_LOOP ( 'NONE', ( #9350, #10710, #7557, #28137 ) ) ;
#2578 = CARTESIAN_POINT ( 'NONE',  ( -30.44716603537182564, -92.66455718075737025, 1.794472358657231981 ) ) ;
#2579 = VERTEX_POINT ( 'NONE', #5776 ) ;
#2580 = CYLINDRICAL_SURFACE ( 'NONE', #13699, 9.500000000000001776 ) ;
#2581 = ADVANCED_FACE ( 'NONE', ( #14932 ), #27566, .T. ) ;
#2582 = CARTESIAN_POINT ( 'NONE',  ( -41.08545581620644072, -63.17361819572722936, -2.647414149845592313 ) ) ;
#2583 = AXIS2_PLACEMENT_3D ( 'NONE', #11642, #3086, #9466 ) ;
#2584 = CARTESIAN_POINT ( 'NONE',  ( -11.77695074595358804, -64.47177034477923030, -23.22164032104561571 ) ) ;
#2585 = DIRECTION ( 'NONE',  ( 0.000000000000000000, -1.000000000000000000, 0.000000000000000000 ) ) ;
#2586 = CARTESIAN_POINT ( 'NONE',  ( -17.80822692750000158, -92.50000000000000000, -18.25149456069999943 ) ) ;
#2587 = CARTESIAN_POINT ( 'NONE',  ( 19.76788193120000159, -18.85499412049999890, 9.715484483839999186 ) ) ;
#2588 = CARTESIAN_POINT ( 'NONE',  ( 7.727575544279999598, -65.07443709589999514, -23.93310889699999677 ) ) ;
#2589 = CARTESIAN_POINT ( 'NONE',  ( -16.62245297557188906, -98.45243480120420543, 8.807067550475276008 ) ) ;
#2590 = ORIENTED_EDGE ( 'NONE', *, *, #6883, .T. ) ;
#2591 = CARTESIAN_POINT ( 'NONE',  ( -11.88137749259999865, -72.18745160699998564, -26.31958153910000320 ) ) ;
#2592 = FACE_OUTER_BOUND ( 'NONE', #9327, .T. ) ;
#2593 = CARTESIAN_POINT ( 'NONE',  ( -12.96062981900000111, -99.85455315880000171, -11.21122132580000041 ) ) ;
#2594 = EDGE_CURVE ( 'NONE', #19704, #12283, #3875, .T. ) ;
#2595 = CARTESIAN_POINT ( 'NONE',  ( 7.120909764619999412E-15, -74.00000000000000000, 40.00000000000000000 ) ) ;
#2596 = CARTESIAN_POINT ( 'NONE',  ( -13.32816333360000094, -99.92967571559999840, -11.12411022969999941 ) ) ;
#2597 = ORIENTED_EDGE ( 'NONE', *, *, #11344, .T. ) ;
#2598 = LINE ( 'NONE', #20061, #20520 ) ;
#2599 = ORIENTED_EDGE ( 'NONE', *, *, #20782, .F. ) ;
#2600 = CARTESIAN_POINT ( 'NONE',  ( 20.63161943080000071, -19.46510050319999863, -7.734358783100000245 ) ) ;
#2601 = CARTESIAN_POINT ( 'NONE',  ( -2.247526421790000395, -96.97547177169998633, 20.70814103409999873 ) ) ;
#2602 = CARTESIAN_POINT ( 'NONE',  ( 2.602364616200000036, -94.19923974040000303, 25.28353855870000189 ) ) ;
#2603 = ORIENTED_EDGE ( 'NONE', *, *, #23973, .T. ) ;
#2604 = ORIENTED_EDGE ( 'NONE', *, *, #23443, .T. ) ;
#2605 = B_SPLINE_CURVE_WITH_KNOTS ( 'NONE', 5,
 ( #27078, #11756, #12565, #18333, #23660, #13801, #23000, #3703, #7263, #18772, #13952, #27366 ),
 .UNSPECIFIED., .F., .F.,
 ( 6, 3, 3, 6 ),
 ( -25.08217527079999698, -18.82032368495484675, -10.56887946708883064, -7.186327137116709451 ),
 .UNSPECIFIED. ) ;
#2606 = LINE ( 'NONE', #26633, #8801 ) ;
#2607 = CARTESIAN_POINT ( 'NONE',  ( 21.40421767500000172, -94.24983954939999364, 13.68415878530000107 ) ) ;
#2608 = CARTESIAN_POINT ( 'NONE',  ( 47.19280742699999820, -74.66666680390001432, -1.149945984370000174 ) ) ;
#2609 = ORIENTED_EDGE ( 'NONE', *, *, #6058, .F. ) ;
#2610 = FACE_OUTER_BOUND ( 'NONE', #14099, .T. ) ;
#2611 = CARTESIAN_POINT ( 'NONE',  ( -21.60034897659999942, -79.81702851609999527, -32.77174746360000057 ) ) ;
#2612 = CARTESIAN_POINT ( 'NONE',  ( -13.24831469989999988, -74.00000000000000000, 34.75169505839999573 ) ) ;
#2613 = EDGE_CURVE ( 'NONE', #2654, #21728, #2421, .T. ) ;
#2614 = CARTESIAN_POINT ( 'NONE',  ( -14.04594405749999986, -93.61368346409999219, -21.04238476760000154 ) ) ;
#2615 = LINE ( 'NONE', #11465, #15190 ) ;
#2616 = VERTEX_POINT ( 'NONE', #25611 ) ;
#2617 = EDGE_CURVE ( 'NONE', #24085, #5350, #6294, .T. ) ;
#2618 = CARTESIAN_POINT ( 'NONE',  ( 36.22844186549999534, -74.00000000000000000, -13.75000000000000000 ) ) ;
#2619 = B_SPLINE_CURVE_WITH_KNOTS ( 'NONE', 3,
 ( #5011, #3138, #20907, #18863, #7515, #1111, #5313, #14202, #5453, #27748, #27171, #22955 ),
 .UNSPECIFIED., .F., .F.,
 ( 4, 2, 2, 2, 2, 4 ),
 ( 0.000000000000000000, 0.2500000000000108802, 0.3750000000000217604, 0.4375000000000137113, 0.5000000000000056621, 1.000000000000000000 ),
 .UNSPECIFIED. ) ;
#2620 = CARTESIAN_POINT ( 'NONE',  ( 14.05983650520000161, -99.53431386179998697, -10.27466730669999961 ) ) ;
#2621 = CARTESIAN_POINT ( 'NONE',  ( -38.70548889989999708, -73.81415926540000783, 7.196178079599999222 ) ) ;
#2622 = CARTESIAN_POINT ( 'NONE',  ( -21.99725903910000113, -74.00000000020000357, -32.02260505910000177 ) ) ;
#2623 = CARTESIAN_POINT ( 'NONE',  ( -27.68682485439999752, -14.30000000000000071, -50.68039294919999804 ) ) ;
#2624 = LINE ( 'NONE', #25351, #26929 ) ;
#2625 = EDGE_CURVE ( 'NONE', #7539, #5596, #14520, .T. ) ;
#2626 = CARTESIAN_POINT ( 'NONE',  ( -7.383625343918562400, -73.99964414703678983, 39.24706873604019819 ) ) ;
#2627 = CARTESIAN_POINT ( 'NONE',  ( 5.789150354839999823E-15, -69.50000000000000000, 32.75000000000000000 ) ) ;
#2628 = VERTEX_POINT ( 'NONE', #9998 ) ;
#2629 = EDGE_CURVE ( 'NONE', #8365, #14272, #16715, .T. ) ;
#2630 = DIRECTION ( 'NONE',  ( 0.000000000000000000, 1.000000000000000000, 0.000000000000000000 ) ) ;
#2631 = CARTESIAN_POINT ( 'NONE',  ( 21.03973548180000108, -61.88564085890000399, 11.46780196789999984 ) ) ;
#2632 = CARTESIAN_POINT ( 'NONE',  ( 1.421085471519999843E-14, -69.00000000000000000, 33.25000000000000000 ) ) ;
#2633 = CARTESIAN_POINT ( 'NONE',  ( 15.71757121830843751, -101.3846248974404460, 3.940829251724543791 ) ) ;
#2634 = CARTESIAN_POINT ( 'NONE',  ( -40.70731707320000226, -77.00000000000000000, -7.215414233289999757 ) ) ;
#2635 = ORIENTED_EDGE ( 'NONE', *, *, #22928, .T. ) ;
#2636 = FACE_OUTER_BOUND ( 'NONE', #22744, .T. ) ;
#2637 = AXIS2_PLACEMENT_3D ( 'NONE', #379, #9223, #9376 ) ;
#2638 = CARTESIAN_POINT ( 'NONE',  ( -11.97719338340000128, -64.78279197330000727, -22.48401985850000173 ) ) ;
#2639 = LINE ( 'NONE', #8865, #17284 ) ;
#2640 = CARTESIAN_POINT ( 'NONE',  ( 7.077994251930249447, -93.31461711599030195, 27.00880202536949426 ) ) ;
#2641 = VERTEX_POINT ( 'NONE', #3462 ) ;
#2642 = CARTESIAN_POINT ( 'NONE',  ( -32.20769385759999892, -80.50000045429999318, -22.43272066369999962 ) ) ;
#2643 = CARTESIAN_POINT ( 'NONE',  ( -41.75000000000000000, -65.49083508809999898, -1.947031612740000028 ) ) ;
#2644 = ORIENTED_EDGE ( 'NONE', *, *, #7665, .T. ) ;
#2645 = CARTESIAN_POINT ( 'NONE',  ( -14.40572000550000098, -18.50000000000000000, 20.06574520719999910 ) ) ;
#2646 = CARTESIAN_POINT ( 'NONE',  ( 7.181689689069999716, -99.92967571559999840, 15.80535034289999885 ) ) ;
#2647 = EDGE_LOOP ( 'NONE', ( #5849, #24143, #22261, #1283 ) ) ;
#2648 = DIRECTION ( 'NONE',  ( 0.000000000000000000, 1.000000000000000000, 0.000000000000000000 ) ) ;
#2649 = CARTESIAN_POINT ( 'NONE',  ( 9.156518149657648209, -94.79128788294934793, -23.00520788063733590 ) ) ;
#2650 = CARTESIAN_POINT ( 'NONE',  ( -27.33941636499999817, -92.81180222680001179, 1.030446961340000023 ) ) ;
#2651 = CARTESIAN_POINT ( 'NONE',  ( -18.83007542230000197, -97.83384886670000924, 6.645594748249999739 ) ) ;
#2652 = CARTESIAN_POINT ( 'NONE',  ( -10.84063885470000166, -18.87168159810000034, -21.93863571940000057 ) ) ;
#2653 = CARTESIAN_POINT ( 'NONE',  ( 11.61699134809713918, -98.12113811987541112, -16.78456760152103300 ) ) ;
#2654 = VERTEX_POINT ( 'NONE', #21236 ) ;
#2655 = EDGE_CURVE ( 'NONE', #15179, #8526, #2490, .T. ) ;
#2656 = CARTESIAN_POINT ( 'NONE',  ( 10.26927205930000042, -92.75885938639999040, -25.49696123720000074 ) ) ;
#2657 = DIRECTION ( 'NONE',  ( 1.000000000000000000, 0.000000000000000000, 0.000000000000000000 ) ) ;
#2658 = CARTESIAN_POINT ( 'NONE',  ( 39.90536558136047773, -73.91587151461750693, 7.249694362032179207 ) ) ;
#2659 = ORIENTED_EDGE ( 'NONE', *, *, #23375, .T. ) ;
#2660 = CARTESIAN_POINT ( 'NONE',  ( 19.57843399940000140, -94.59276292389999696, 13.52682119470000011 ) ) ;
#2661 = FACE_OUTER_BOUND ( 'NONE', #16860, .T. ) ;
#2662 = DIRECTION ( 'NONE',  ( 0.8775825618903722036, 0.000000000000000000, -0.4794255386042041156 ) ) ;
#2663 = EDGE_LOOP ( 'NONE', ( #28748, #23889, #24650, #12109, #9724 ) ) ;
#2664 = EDGE_CURVE ( 'NONE', #24292, #20440, #167, .T. ) ;
#2665 = CARTESIAN_POINT ( 'NONE',  ( 36.87753886209557663, -80.23900670806611402, -13.59568402046754976 ) ) ;
#2666 = CARTESIAN_POINT ( 'NONE',  ( -19.81272040990000249, -52.63293862049999916, 12.05498172269999912 ) ) ;
#2667 = DIRECTION ( 'NONE',  ( 1.000000000000000000, 0.000000000000000000, 0.000000000000000000 ) ) ;
#2668 = CARTESIAN_POINT ( 'NONE',  ( 32.04416956680000084, -73.81489368219999392, -20.33277479140000210 ) ) ;
#2669 =( NAMED_UNIT ( * ) PLANE_ANGLE_UNIT ( ) SI_UNIT ( $, .RADIAN. ) );
#2670 = ORIENTED_EDGE ( 'NONE', *, *, #21882, .F. ) ;
#2671 = DIRECTION ( 'NONE',  ( 0.4794255386042041156, 0.000000000000000000, 0.8775825618903720926 ) ) ;
#2672 = CARTESIAN_POINT ( 'NONE',  ( 9.385332722619999402, -98.68450614990000247, 16.47661810339999988 ) ) ;
#2673 = CARTESIAN_POINT ( 'NONE',  ( 10.23740437490000055, -99.60591711109999835, 14.03865835380000071 ) ) ;
#2674 = ORIENTED_EDGE ( 'NONE', *, *, #589, .T. ) ;
#2675 = FACE_OUTER_BOUND ( 'NONE', #1727, .T. ) ;
#2676 = CARTESIAN_POINT ( 'NONE',  ( 20.47205805249999955, -93.24058218799999054, 16.33781131059999936 ) ) ;
#2677 = B_SPLINE_SURFACE_WITH_KNOTS ( 'NONE', 5, 5, ( 
 ( #2173, #2618, #19781, #28802, #28662, #8695 ),
 ( #17611, #24312, #4351, #13224, #27088, #14114 ),
 ( #883, #27677, #442, #23289, #7130, #7577 ),
 ( #13963, #743, #27379, #9588, #15996, #11468 ),
 ( #18194, #18638, #25474, #2908, #11616, #9292 ),
 ( #24902, #25344, #4932, #18488, #16138, #18785 ) ),
 .UNSPECIFIED., .F., .F., .F.,
 ( 6, 6 ),
 ( 6, 6 ),
 ( 0.000000000000000000, 1.940837277319999998 ),
 ( 0.000000000000000000, 0.5000000000000000000 ),
 .UNSPECIFIED. ) ;
#2678 = CARTESIAN_POINT ( 'NONE',  ( 24.39713799250000292, -19.50000027030000282, 1.459766484860000046 ) ) ;
#2679 = CARTESIAN_POINT ( 'NONE',  ( 26.82296289428647285, -72.69303614417458448, -10.31361415116993641 ) ) ;
#2680 = CARTESIAN_POINT ( 'NONE',  ( -12.56720507379640495, -101.6484611540000031, -9.903160520584330939 ) ) ;
#2681 = CARTESIAN_POINT ( 'NONE',  ( 9.320854954070000531, -36.00000000000000000, -20.33059790500000119 ) ) ;
#2682 = CARTESIAN_POINT ( 'NONE',  ( 8.935678578700709807, -19.49096733334448928, -19.40207715605563266 ) ) ;
#2683 = ORIENTED_EDGE ( 'NONE', *, *, #13823, .F. ) ;
#2684 = AXIS2_PLACEMENT_3D ( 'NONE', #10869, #18783, #3330 ) ;
#2685 = EDGE_CURVE ( 'NONE', #23505, #18491, #15682, .T. ) ;
#2686 = VECTOR ( 'NONE', #6161, 1000.000000000000000 ) ;
#2687 = CARTESIAN_POINT ( 'NONE',  ( 7.936175460970000373, -99.23650994359999800, 16.10618517760000046 ) ) ;
#2688 = DIRECTION ( 'NONE',  ( 0.000000000000000000, 1.000000000000000000, 0.000000000000000000 ) ) ;
#2689 = CARTESIAN_POINT ( 'NONE',  ( -7.333307833730000169, -94.59276292389999696, -22.63874420850000035 ) ) ;
#2690 = CARTESIAN_POINT ( 'NONE',  ( -14.65665286289999969, -74.43375220249998847, 36.94583910070000599 ) ) ;
#2691 = CARTESIAN_POINT ( 'NONE',  ( 11.22133265290000104, -100.9938510739999913, -10.73518741380000030 ) ) ;
#2692 = CARTESIAN_POINT ( 'NONE',  ( -1.179190554560000104, -39.36414254499999288, -22.77357817330000245 ) ) ;
#2693 = CARTESIAN_POINT ( 'NONE',  ( 15.49409222530310615, -95.04050137967534795, 17.29256239693905073 ) ) ;
#2694 = ADVANCED_FACE ( 'NONE', ( #28490 ), #28347, .T. ) ;
#2695 = CARTESIAN_POINT ( 'NONE',  ( -38.08919256720000135, -65.74290439030001210, 1.043878858160000034 ) ) ;
#2696 = AXIS2_PLACEMENT_3D ( 'NONE', #17695, #28613, #4289 ) ;
#2697 = CARTESIAN_POINT ( 'NONE',  ( -38.25000000000000000, -65.14977478849999670, 2.684678751729999480 ) ) ;
#2698 = DIRECTION ( 'NONE',  ( 0.000000000000000000, 1.000000000000000000, 0.000000000000000000 ) ) ;
#2699 = DIRECTION ( 'NONE',  ( -0.8775825618903722036, 0.000000000000000000, 0.4794255386042041156 ) ) ;
#2700 = ORIENTED_EDGE ( 'NONE', *, *, #28663, .F. ) ;
#2701 = CARTESIAN_POINT ( 'NONE',  ( 36.24656976640000039, -75.00000018780001199, -15.05817680799999891 ) ) ;
#2702 = CARTESIAN_POINT ( 'NONE',  ( -22.22906643760000023, -79.50000000000000000, -32.83566815539999340 ) ) ;
#2703 = CARTESIAN_POINT ( 'NONE',  ( 7.984254895100000304, -100.9843696920000014, 13.33388511600000115 ) ) ;
#2704 = CIRCLE ( 'NONE', #25495, 3.499999999999999556 ) ;
#2705 = CARTESIAN_POINT ( 'NONE',  ( -13.80673513500000027, -68.20222042139999985, 22.71145972000000057 ) ) ;
#2706 = ADVANCED_FACE ( 'NONE', ( #13029 ), #22227, .T. ) ;
#2707 = CARTESIAN_POINT ( 'NONE',  ( -13.26199019340000085, -58.91587053549999808, 20.59544867430000181 ) ) ;
#2708 = DIRECTION ( 'NONE',  ( 0.000000000000000000, 1.000000000000000000, 0.000000000000000000 ) ) ;
#2709 = CARTESIAN_POINT ( 'NONE',  ( 25.97241523970000188, -92.68283745200000112, 10.25715990590000004 ) ) ;
#2710 = CARTESIAN_POINT ( 'NONE',  ( 20.06309461859999743, -36.00000000000000000, -9.476129726630000860 ) ) ;
#2711 = CARTESIAN_POINT ( 'NONE',  ( -13.42523386781685169, -94.35876167532840952, -21.59623076260758978 ) ) ;
#2712 = CARTESIAN_POINT ( 'NONE',  ( 27.68682485439999752, -24.80000000000000071, 50.68039294919999804 ) ) ;
#2713 = CARTESIAN_POINT ( 'NONE',  ( -11.23228026081345199, -39.24428776201335722, -22.24512021485102053 ) ) ;
#2714 = ORIENTED_EDGE ( 'NONE', *, *, #18312, .T. ) ;
#2715 = CARTESIAN_POINT ( 'NONE',  ( 28.41585885021854097, -74.42752580149716835, -27.07206850168904566 ) ) ;
#2716 = AXIS2_PLACEMENT_3D ( 'NONE', #4651, #13234, #17479 ) ;
#2717 = CARTESIAN_POINT ( 'NONE',  ( -20.15180004589999996, -97.32097376039999403, -7.274423422870000877 ) ) ;
#2718 = EDGE_LOOP ( 'NONE', ( #27894, #16569, #23075, #22728 ) ) ;
#2719 = CARTESIAN_POINT ( 'NONE',  ( 8.546518572781618417, -92.66972459458614253, 29.27809851676327924 ) ) ;
#2720 = ORIENTED_EDGE ( 'NONE', *, *, #8478, .T. ) ;
#2721 = EDGE_CURVE ( 'NONE', #21247, #17262, #18248, .T. ) ;
#2722 = DIRECTION ( 'NONE',  ( -0.3443190008117950063, 0.000000000000000000, 0.9388527177784421474 ) ) ;
#2723 = CARTESIAN_POINT ( 'NONE',  ( 0.000000000000000000, -30.20000000000000284, 0.000000000000000000 ) ) ;
#2724 = CARTESIAN_POINT ( 'NONE',  ( -12.43380386931423232, -65.01950801014830006, -21.83872194420420598 ) ) ;
#2725 = CARTESIAN_POINT ( 'NONE',  ( 40.00000000000000000, -74.00000000000000000, 2.009834509230000106E-15 ) ) ;
#2726 = DIRECTION ( 'NONE',  ( -0.3790931394101558771, -0.6121731929912518355, -0.6939253370752848094 ) ) ;
#2727 = CARTESIAN_POINT ( 'NONE',  ( -21.40239531899999648, -66.04426305559999832, 14.04033265860000057 ) ) ;
#2728 = CARTESIAN_POINT ( 'NONE',  ( -17.53169516290746444, -96.08573336708691670, 13.07164240864208082 ) ) ;
#2729 = VERTEX_POINT ( 'NONE', #11123 ) ;
#2730 = CIRCLE ( 'NONE', #20874, 2.999999999999999556 ) ;
#2731 = CARTESIAN_POINT ( 'NONE',  ( -11.98650081279999924, -70.39409877170000129, -25.90118300180000332 ) ) ;
#2732 = DIRECTION ( 'NONE',  ( 0.000000000000000000, -1.000000000000000000, 0.000000000000000000 ) ) ;
#2733 = CARTESIAN_POINT ( 'NONE',  ( 7.794725237649443805, -101.6024172056560815, 14.01240486772618432 ) ) ;
#2734 = DIRECTION ( 'NONE',  ( -0.8091158474751273255, 0.000000000000000000, -0.5876491686070921538 ) ) ;
#2735 = CARTESIAN_POINT ( 'NONE',  ( -39.03038279190000281, -74.00032110560000831, -7.562806955070000114 ) ) ;
#2736 = EDGE_LOOP ( 'NONE', ( #6226, #10424, #9912, #2192, #22297, #13876 ) ) ;
#2737 = CARTESIAN_POINT ( 'NONE',  ( 26.96539441263278647, -92.54383083955173106, -14.25194291928822565 ) ) ;
#2738 = VERTEX_POINT ( 'NONE', #26174 ) ;
#2739 = ADVANCED_FACE ( 'NONE', ( #13184 ), #21790, .T. ) ;
#2740 = DIRECTION ( 'NONE',  ( 0.8775825618903722036, 0.000000000000000000, -0.4794255386042041156 ) ) ;
#2741 = CARTESIAN_POINT ( 'NONE',  ( -3.966380828739999753, -98.30614355410000371, 19.04978114919999754 ) ) ;
#2742 = CARTESIAN_POINT ( 'NONE',  ( 11.26760366760000132, -92.51839641809998227, 27.23952649899999656 ) ) ;
#2743 = ORIENTED_EDGE ( 'NONE', *, *, #9045, .F. ) ;
#2744 = AXIS2_PLACEMENT_3D ( 'NONE', #18895, #21634, #1408 ) ;
#2745 = TOROIDAL_SURFACE ( 'NONE', #23653, 13.00000000000000000, 2.000000000000000000 ) ;
#2746 = ORIENTED_EDGE ( 'NONE', *, *, #8123, .T. ) ;
#2747 = DIRECTION ( 'NONE',  ( 1.000000000000000000, 0.000000000000000000, 0.000000000000000000 ) ) ;
#2748 = CARTESIAN_POINT ( 'NONE',  ( 27.18988201479999844, -25.69844555429999744, 49.77074518290000071 ) ) ;
#2749 = CARTESIAN_POINT ( 'NONE',  ( 9.988478739970000575, -36.00000000000000000, -20.41376899180000137 ) ) ;
#2750 = ORIENTED_EDGE ( 'NONE', *, *, #10665, .T. ) ;
#2751 = CARTESIAN_POINT ( 'NONE',  ( 7.225850277544148881, -73.65029154561577229, -39.40310785672224370 ) ) ;
#2752 = FACE_OUTER_BOUND ( 'NONE', #15905, .T. ) ;
#2753 = DIRECTION ( 'NONE',  ( 1.000000000000000000, 0.000000000000000000, 0.000000000000000000 ) ) ;
#2754 = CARTESIAN_POINT ( 'NONE',  ( -4.085206522429999154, -70.99734270939998737, -28.45162464230000054 ) ) ;
#2755 = CARTESIAN_POINT ( 'NONE',  ( 22.26662627820000040, -57.47855601759999900, -7.066909182079999852 ) ) ;
#2756 = CARTESIAN_POINT ( 'NONE',  ( -22.11864956829469619, -74.07080536734231657, -32.38124336146950810 ) ) ;
#2757 = ORIENTED_EDGE ( 'NONE', *, *, #18056, .F. ) ;
#2758 = CARTESIAN_POINT ( 'NONE',  ( -14.78710422270000002, -79.49999982573447710, 36.35833235879999847 ) ) ;
#2759 = CARTESIAN_POINT ( 'NONE',  ( -2.694596519430000559, -63.24129318349999807, -26.04567641519999910 ) ) ;
#2760 = CARTESIAN_POINT ( 'NONE',  ( -22.10393671050000108, -74.26505820949999759, -32.64452500950000058 ) ) ;
#2761 = ORIENTED_EDGE ( 'NONE', *, *, #3818, .F. ) ;
#2762 = AXIS2_PLACEMENT_3D ( 'NONE', #3121, #7492, #11972 ) ;
#2763 = DIRECTION ( 'NONE',  ( 0.000000000000000000, -1.000000000000000000, 0.000000000000000000 ) ) ;
#2764 = CARTESIAN_POINT ( 'NONE',  ( -2.619606055569999814, -19.50000000000000000, -24.29997775220000023 ) ) ;
#2765 = FACE_OUTER_BOUND ( 'NONE', #13647, .T. ) ;
#2766 = ORIENTED_EDGE ( 'NONE', *, *, #12031, .T. ) ;
#2767 = AXIS2_PLACEMENT_3D ( 'NONE', #16696, #12175, #1554 ) ;
#2768 = CIRCLE ( 'NONE', #19499, 0.8000000000000003775 ) ;
#2769 = CARTESIAN_POINT ( 'NONE',  ( -10.73934281380000044, -93.50968831570000361, -23.38067028629999555 ) ) ;
#2770 = CIRCLE ( 'NONE', #24148, 20.64285714289999873 ) ;
#2771 = CARTESIAN_POINT ( 'NONE',  ( 21.85294459619999685, -62.89113864609998927, 10.91972205250000094 ) ) ;
#2772 = CARTESIAN_POINT ( 'NONE',  ( 8.988163966810001071, -35.02801756110000042, -19.45347226109999994 ) ) ;
#2773 = CARTESIAN_POINT ( 'NONE',  ( 15.61948084379431201, -101.6484611539999889, 3.469733395131306963 ) ) ;
#2774 = CYLINDRICAL_SURFACE ( 'NONE', #25788, 57.74999999999999289 ) ;
#2775 = EDGE_LOOP ( 'NONE', ( #20148, #24485, #15477, #18761 ) ) ;
#2776 = CARTESIAN_POINT ( 'NONE',  ( 47.25000000000000000, -79.00000000000000000, -7.709388683000000122E-13 ) ) ;
#2777 = CARTESIAN_POINT ( 'NONE',  ( -11.24280342539999822, -58.88258727490000410, -22.09277839770000185 ) ) ;
#2778 = CARTESIAN_POINT ( 'NONE',  ( 36.90870977912933881, -79.74033897581968233, -14.42227066965258686 ) ) ;
#2779 = CARTESIAN_POINT ( 'NONE',  ( 23.93312032140000056, -65.07443051799999978, -7.727578354849999442 ) ) ;
#2780 = DIRECTION ( 'NONE',  ( 0.000000000000000000, 1.000000000000000000, 0.000000000000000000 ) ) ;
#2781 = EDGE_CURVE ( 'NONE', #731, #6736, #12177, .T. ) ;
#2782 = ORIENTED_EDGE ( 'NONE', *, *, #7608, .F. ) ;
#2783 = DIRECTION ( 'NONE',  ( 0.000000000000000000, 1.000000000000000000, 0.000000000000000000 ) ) ;
#2784 = DIRECTION ( 'NONE',  ( -0.4509255599460827435, -0.3396444637780623443, -0.8254137008871517134 ) ) ;
#2786 = VERTEX_POINT ( 'NONE', #28768 ) ;
#2785 = AXIS2_PLACEMENT_3D ( 'NONE', #26617, #12312, #27917 ) ;
#2787 = CARTESIAN_POINT ( 'NONE',  ( -13.53260628059999959, -42.21390124650000075, 20.62898559450000135 ) ) ;
#2788 = CARTESIAN_POINT ( 'NONE',  ( -6.580578580030000957, -101.1889999979999999, 15.40319725099999992 ) ) ;
#2789 = EDGE_CURVE ( 'NONE', #12473, #4490, #11720, .T. ) ;
#2790 = VERTEX_POINT ( 'NONE', #26461 ) ;
#2791 = CARTESIAN_POINT ( 'NONE',  ( -26.69293917519999937, -15.49689110870000164, -48.86109741659999628 ) ) ;
#2792 = ADVANCED_FACE ( 'NONE', ( #8662 ), #22448, .T. ) ;
#2793 = AXIS2_PLACEMENT_3D ( 'NONE', #11897, #20807, #28065 ) ;
#2794 = CARTESIAN_POINT ( 'NONE',  ( 7.229652833200000295, -101.2530993470000027, 13.36368574970000012 ) ) ;
#2795 = CARTESIAN_POINT ( 'NONE',  ( -11.02010494672524388, -19.46474609920444365, -19.15837582207361933 ) ) ;
#2796 = CARTESIAN_POINT ( 'NONE',  ( -17.00713571869999896, -99.92967601899998442, 3.484593143450000152 ) ) ;
#2797 = DIRECTION ( 'NONE',  ( 0.000000000000000000, 1.000000000000000000, 0.000000000000000000 ) ) ;
#2798 = CARTESIAN_POINT ( 'NONE',  ( 21.79230230059999940, -37.95144147500000287, -8.472395268590000583 ) ) ;
#2799 = ORIENTED_EDGE ( 'NONE', *, *, #3072, .T. ) ;
#2800 = CARTESIAN_POINT ( 'NONE',  ( -32.66023292159999869, -79.72849242800000980, -21.85457041760000152 ) ) ;
#2801 = CARTESIAN_POINT ( 'NONE',  ( -38.22259796004242816, -65.70975255743678645, -1.354924268994119885 ) ) ;
#2802 = CARTESIAN_POINT ( 'NONE',  ( 0.000000000000000000, -92.50000000000000000, 0.000000000000000000 ) ) ;
#2803 = CARTESIAN_POINT ( 'NONE',  ( -13.13823760000467367, -92.72722989462275223, 27.52520356741175789 ) ) ;
#2804 = EDGE_LOOP ( 'NONE', ( #1720, #22121, #8458, #4717 ) ) ;
#2805 = CARTESIAN_POINT ( 'NONE',  ( 7.120909764619999412E-15, -69.50000000000000000, 40.00000000000000000 ) ) ;
#2806 = DIRECTION ( 'NONE',  ( 1.000000000000000000, 0.000000000000000000, 0.000000000000000000 ) ) ;
#2807 = DIRECTION ( 'NONE',  ( 0.000000000000000000, -1.000000000000000000, 0.000000000000000000 ) ) ;
#2808 = ORIENTED_EDGE ( 'NONE', *, *, #5850, .F. ) ;
#2809 = CARTESIAN_POINT ( 'NONE',  ( -16.89118076489999964, -98.29694271920000403, 8.926253644079999106 ) ) ;
#2810 = CARTESIAN_POINT ( 'NONE',  ( -19.49041480450000208, -52.62618816490000029, 12.93508487010000074 ) ) ;
#2811 = LINE ( 'NONE', #27586, #27757 ) ;
#2812 = CARTESIAN_POINT ( 'NONE',  ( -20.30440251868529700, -57.41946960321629234, 14.68517168904920567 ) ) ;
#2813 = FACE_OUTER_BOUND ( 'NONE', #11451, .T. ) ;
#2814 = AXIS2_PLACEMENT_3D ( 'NONE', #3591, #18624, #27928 ) ;
#2815 = CARTESIAN_POINT ( 'NONE',  ( 25.27264777759999959, -64.89165752090001149, 0.6762964727910000251 ) ) ;
#2816 = ADVANCED_FACE ( 'NONE', ( #6344 ), #1846, .T. ) ;
#2817 = ORIENTED_EDGE ( 'NONE', *, *, #27726, .F. ) ;
#2818 = CARTESIAN_POINT ( 'NONE',  ( 40.00000000000000000, -69.50000000000000000, 5.786765616290000531E-15 ) ) ;
#2819 = CARTESIAN_POINT ( 'NONE',  ( 12.43176822059999864, -98.26008456249999767, 14.57113454829999988 ) ) ;
#2820 = ORIENTED_EDGE ( 'NONE', *, *, #24466, .T. ) ;
#2821 = CARTESIAN_POINT ( 'NONE',  ( 7.627568735119999666, -74.00000000000000000, 38.62788659690000515 ) ) ;
#2822 = CARTESIAN_POINT ( 'NONE',  ( -39.50000000000000000, -64.47022873560000278, 2.309401076760000393 ) ) ;
#2823 = ADVANCED_FACE ( 'NONE', ( #10686 ), #10972, .T. ) ;
#2824 = CARTESIAN_POINT ( 'NONE',  ( -7.443709283000000454, -101.0405520670000072, 14.44167797660000119 ) ) ;
#2825 = FACE_OUTER_BOUND ( 'NONE', #9695, .T. ) ;
#2826 = CARTESIAN_POINT ( 'NONE',  ( 4.500000000000000000, -11.00000000000000000, 31.00000000000000000 ) ) ;
#2827 = CARTESIAN_POINT ( 'NONE',  ( 9.165577939120000295, -36.05978003129999365, -20.59810505469999953 ) ) ;
#2828 = AXIS2_PLACEMENT_3D ( 'NONE', #17866, #18455, #403 ) ;
#2829 = CARTESIAN_POINT ( 'NONE',  ( 7.500294343269999331, -101.1699703470000031, 13.83260060669999980 ) ) ;
#2830 = ORIENTED_EDGE ( 'NONE', *, *, #21482, .F. ) ;
#2831 = CARTESIAN_POINT ( 'NONE',  ( -40.12703402703129285, -74.06318173156705598, 7.249276399910129953 ) ) ;
#2832 = AXIS2_PLACEMENT_3D ( 'NONE', #21321, #8470, #14880 ) ;
#2833 = DIRECTION ( 'NONE',  ( 0.8775825618903724257, 0.000000000000000000, 0.4794255386042036160 ) ) ;
#2834 = DIRECTION ( 'NONE',  ( -0.8981584475625418174, 0.000000000000000000, -0.4396719266362647538 ) ) ;
#2835 = VERTEX_POINT ( 'NONE', #15208 ) ;
#2836 = CARTESIAN_POINT ( 'NONE',  ( -1.464217970924556633, -19.46608320369988121, -22.20330980833862355 ) ) ;
#2837 = B_SPLINE_CURVE_WITH_KNOTS ( 'NONE', 5,
 ( #18047, #25044, #22427, #22868, #11469, #15698, #24604, #2759, #27236, #22271, #9142, #18195 ),
 .UNSPECIFIED., .F., .F.,
 ( 6, 3, 3, 6 ),
 ( 112.4516934179999907, 115.4092999559999981, 122.7593676420000008, 122.9563471680000077 ),
 .UNSPECIFIED. ) ;
#2838 = CARTESIAN_POINT ( 'NONE',  ( 11.43385261259999908, -100.9763228559999959, -10.73324566510000011 ) ) ;
#2839 = CARTESIAN_POINT ( 'NONE',  ( -1.456904695350000001, -52.62618816490000029, -23.34673678599999747 ) ) ;
#2840 = CARTESIAN_POINT ( 'NONE',  ( 15.77015574596263647, -94.90770262334949336, 17.27435799970811203 ) ) ;
#2841 = FACE_OUTER_BOUND ( 'NONE', #1817, .T. ) ;
#2842 = CARTESIAN_POINT ( 'NONE',  ( 22.12830645909999916, -53.29680639610000270, -7.019998623859999398 ) ) ;
#2843 = CARTESIAN_POINT ( 'NONE',  ( 8.986258419809999509, -35.50000000000000000, -19.49544308430000328 ) ) ;
#2844 = DIRECTION ( 'NONE',  ( 0.6184463001828854889, 0.000000000000000000, 0.7858270635388554526 ) ) ;
#2845 = VERTEX_POINT ( 'NONE', #6494 ) ;
#2846 = CARTESIAN_POINT ( 'NONE',  ( 36.59060393619999729, -74.92841728889999331, -14.75000109939999859 ) ) ;
#2847 = FACE_OUTER_BOUND ( 'NONE', #15652, .T. ) ;
#2848 = CARTESIAN_POINT ( 'NONE',  ( -22.65559868730312942, -80.00000000000000000, -32.64705978834439293 ) ) ;
#2849 = EDGE_CURVE ( 'NONE', #2022, #9163, #13594, .T. ) ;
#2850 = AXIS2_PLACEMENT_3D ( 'NONE', #18388, #25384, #12095 ) ;
#2851 = CIRCLE ( 'NONE', #25193, 7.249999999999999112 ) ;
#2852 = EDGE_CURVE ( 'NONE', #21621, #5717, #12525, .T. ) ;
#2853 = AXIS2_PLACEMENT_3D ( 'NONE', #7526, #6256, #12936 ) ;
#2854 = CARTESIAN_POINT ( 'NONE',  ( 23.70295813380000283, -94.59276292389999696, -2.111851990829999970 ) ) ;
#2855 = CARTESIAN_POINT ( 'NONE',  ( 20.91697839109999890, -35.19239095940000084, -8.427788642599999491 ) ) ;
#2856 = DIRECTION ( 'NONE',  ( 0.000000000000000000, -1.000000000000000000, 0.000000000000000000 ) ) ;
#2857 = FACE_OUTER_BOUND ( 'NONE', #24929, .T. ) ;
#2858 = CARTESIAN_POINT ( 'NONE',  ( 0.000000000000000000, -37.08699221940000257, 0.000000000000000000 ) ) ;
#2859 = CARTESIAN_POINT ( 'NONE',  ( 0.4184155361420000552, -92.92146929989999649, -30.38020812550000116 ) ) ;
#2860 = EDGE_CURVE ( 'NONE', #9320, #26317, #4770, .T. ) ;
#2861 = DIRECTION ( 'NONE',  ( 0.000000000000000000, -1.000000000000000000, 0.000000000000000000 ) ) ;
#2862 = CARTESIAN_POINT ( 'NONE',  ( 16.22917866779999940, -99.91102932019998661, 4.812753184709999132 ) ) ;
#2863 = ORIENTED_EDGE ( 'NONE', *, *, #21763, .T. ) ;
#2864 = DIRECTION ( 'NONE',  ( 1.000000000000000000, 0.000000000000000000, 0.000000000000000000 ) ) ;
#2865 = CARTESIAN_POINT ( 'NONE',  ( -17.52282427860000169, -98.26007807950000483, -7.734195792939999592 ) ) ;
#2866 = ORIENTED_EDGE ( 'NONE', *, *, #14425, .T. ) ;
#2867 = CARTESIAN_POINT ( 'NONE',  ( 8.879714594546598505, -92.75430643264905939, 29.17881595893258506 ) ) ;
#2868 = VERTEX_POINT ( 'NONE', #27195 ) ;
#2869 = LINE ( 'NONE', #6796, #25350 ) ;
#2870 = DIRECTION ( 'NONE',  ( 0.4794255386042042266, 0.000000000000000000, 0.8775825618903720926 ) ) ;
#2871 = LINE ( 'NONE', #16250, #15503 ) ;
#2872 = AXIS2_PLACEMENT_3D ( 'NONE', #1782, #4683, #6875 ) ;
#2873 = B_SPLINE_CURVE_WITH_KNOTS ( 'NONE', 5,
 ( #2166, #8990, #17897, #4190, #17460, #19915 ),
 .UNSPECIFIED., .F., .F.,
 ( 6, 6 ),
 ( 0.000000000000000000, 1.000000000000000000 ),
 .UNSPECIFIED. ) ;
#2874 = CARTESIAN_POINT ( 'NONE',  ( -7.230541818644482532, -73.67850591084784639, -39.46631086812988087 ) ) ;
#2875 = AXIS2_PLACEMENT_3D ( 'NONE', #14983, #8432, #7892 ) ;
#2876 = AXIS2_PLACEMENT_3D ( 'NONE', #24730, #9264, #2732 ) ;
#2877 = CARTESIAN_POINT ( 'NONE',  ( -14.90631076309999870, -74.36723410090000641, 36.29697133340000192 ) ) ;
#2878 = CARTESIAN_POINT ( 'NONE',  ( -21.78892497420000041, -67.75971617740000852, 15.66234658180000139 ) ) ;
#2879 = CARTESIAN_POINT ( 'NONE',  ( -15.50938051129999984, -101.3150705480000084, 4.855933523060000034 ) ) ;
#2880 = VERTEX_POINT ( 'NONE', #25156 ) ;
#2881 = CARTESIAN_POINT ( 'NONE',  ( -12.01481558839999941, -71.12613788880000243, -25.81978417510000057 ) ) ;
#2882 = DIRECTION ( 'NONE',  ( 1.000000000000000000, 0.000000000000000000, 0.000000000000000000 ) ) ;
#2883 = DIRECTION ( 'NONE',  ( -0.6710129359900831592, 0.000000000000000000, 0.7414456417930908039 ) ) ;
#2884 = DIRECTION ( 'NONE',  ( 0.000000000000000000, 1.000000000000000000, 0.000000000000000000 ) ) ;
#2885 = CARTESIAN_POINT ( 'NONE',  ( 15.89267423569999949, -101.2490009469999990, 2.460413036130000286 ) ) ;
#2886 = ORIENTED_EDGE ( 'NONE', *, *, #16918, .F. ) ;
#2887 = ORIENTED_EDGE ( 'NONE', *, *, #24848, .F. ) ;
#2888 = EDGE_CURVE ( 'NONE', #8967, #13063, #20564, .T. ) ;
#2889 = CARTESIAN_POINT ( 'NONE',  ( -2.584575094209999868, -57.80430419099999995, -25.24242492149999961 ) ) ;
#2890 = B_SPLINE_CURVE_WITH_KNOTS ( 'NONE', 3,
 ( #16132, #7709, #16576, #25470, #437, #16431, #12048, #13956, #18629, #9285, #20814, #5067, #733, #9582, #2902, #586, #25033, #11760, #15989, #5223, #18483, #9431, #11608, #7414, #18186, #23283, #5501, #11908, #16277 ),
 .UNSPECIFIED., .F., .F.,
 ( 4, 2, 2, 2, 1, 1, 1, 1, 2, 2, 2, 2, 1, 1, 1, 2, 2, 4 ),
 ( 0.000000000000000000, 0.2500000000000724976, 0.3750000000001087463, 0.4375000000001268985, 0.4687500000001376677, 0.4843750000001449396, 0.4921875000001469935, 0.4960937500001482703, 0.4980468750001488254, 0.5000000000001494360, 0.6250000000001784128, 0.6875000000001919576, 0.7187500000001986189, 0.7343750000002017275, 0.7421875000002008393, 0.7460937500002003953, 0.7500000000001999512, 1.000000000000000000 ),
 .UNSPECIFIED. ) ;
#2891 = CARTESIAN_POINT ( 'NONE',  ( -2.620111886150000124, -97.23151481229999149, 21.21167663179999963 ) ) ;
#2892 = EDGE_CURVE ( 'NONE', #24483, #24085, #19173, .T. ) ;
#2893 = CONICAL_SURFACE ( 'NONE', #7090, 5.499999999999999112, 0.3217505543970000104 ) ;
#2894 = CARTESIAN_POINT ( 'NONE',  ( 5.617108918220000469, -93.05272100550000403, 26.49227707150000199 ) ) ;
#2895 = CIRCLE ( 'NONE', #14053, 7.249999999999999112 ) ;
#2896 = ORIENTED_EDGE ( 'NONE', *, *, #18686, .T. ) ;
#2897 = EDGE_LOOP ( 'NONE', ( #1127, #12201, #26392, #17100 ) ) ;
#2898 = CARTESIAN_POINT ( 'NONE',  ( 20.87140401170000104, -36.00000000000000000, -10.07774184699999864 ) ) ;
#2899 = CARTESIAN_POINT ( 'NONE',  ( 47.18156435510000080, -74.63486761890000309, -1.134764142530000131 ) ) ;
#2900 = ORIENTED_EDGE ( 'NONE', *, *, #1713, .F. ) ;
#2901 = CARTESIAN_POINT ( 'NONE',  ( 7.213678002751584550, -73.60295742109886419, -39.27497438193323376 ) ) ;
#2902 = CARTESIAN_POINT ( 'NONE',  ( -11.45632417142031301, -61.34567075806889846, 20.94901889759627522 ) ) ;
#2903 = ORIENTED_EDGE ( 'NONE', *, *, #24675, .T. ) ;
#2904 = CARTESIAN_POINT ( 'NONE',  ( -8.907626117019999512, -96.37889029669999275, -20.95313078519999905 ) ) ;
#2905 = CARTESIAN_POINT ( 'NONE',  ( -3.852920966090000121, -71.18862645909999287, -28.24098550969999977 ) ) ;
#2906 = LINE ( 'NONE', #12193, #6854 ) ;
#2907 = EDGE_LOOP ( 'NONE', ( #13611, #23142, #26239, #26486 ) ) ;
#2908 = CARTESIAN_POINT ( 'NONE',  ( 36.47365836190000010, -74.39700102820000893, -14.67944147449999903 ) ) ;
#2909 = CARTESIAN_POINT ( 'NONE',  ( -16.13888085079999613, -100.3684813130000038, 2.534467327679999826 ) ) ;
#2910 = CARTESIAN_POINT ( 'NONE',  ( 25.80868167070000396, -64.58097566740001128, 1.225860731590000086 ) ) ;
#2911 = CARTESIAN_POINT ( 'NONE',  ( -22.03141727930000116, -74.00000000000000000, -32.02573219850000186 ) ) ;
#2912 = ADVANCED_FACE ( 'NONE', ( #5337 ), #22924, .F. ) ;
#2913 = ORIENTED_EDGE ( 'NONE', *, *, #11565, .F. ) ;
#2914 = DIRECTION ( 'NONE',  ( 1.000000000000000000, 0.000000000000000000, 0.000000000000000000 ) ) ;
#2915 = CARTESIAN_POINT ( 'NONE',  ( -7.366413754511537348, -73.99967301548019805, 39.30374743330985154 ) ) ;
#2916 = CARTESIAN_POINT ( 'NONE',  ( 36.75354318842512669, -74.46086523469682561, -14.59276404010832628 ) ) ;
#2917 = ORIENTED_EDGE ( 'NONE', *, *, #11507, .T. ) ;
#2918 = CYLINDRICAL_SURFACE ( 'NONE', #12769, 32.39999999999999858 ) ;
#2919 = DIRECTION ( 'NONE',  ( 0.9408310772095872521, 0.000000000000000000, 0.3388759126238510833 ) ) ;
#2920 = CARTESIAN_POINT ( 'NONE',  ( 8.988706506799999829, -34.85239680849999644, -19.44233762329999848 ) ) ;
#2921 = CARTESIAN_POINT ( 'NONE',  ( 16.58398298995137665, -100.1994045927079924, 4.339543189922326683 ) ) ;
#2922 = CARTESIAN_POINT ( 'NONE',  ( 19.72731200591455192, -94.57749869813547150, 14.01461210758740705 ) ) ;
#2923 = VERTEX_POINT ( 'NONE', #22975 ) ;
#2924 = CARTESIAN_POINT ( 'NONE',  ( 20.69873715099999956, -52.63055504180000099, 10.61298605969999898 ) ) ;
#2925 = B_SPLINE_SURFACE_WITH_KNOTS ( 'NONE', 5, 5, ( 
 ( #12330, #21238, #12191, #21107, #879, #12459 ),
 ( #10131, #21372, #10275, #8109, #28074, #9720 ),
 ( #14253, #18630, #27528, #18778, #5504, #16434 ),
 ( #23144, #12049, #20965, #1024, #26176, #6050 ),
 ( #4017, #23836, #28631, #22094, #4158, #12603 ),
 ( #1847, #23697, #3739, #14796, #17571, #13031 ) ),
 .UNSPECIFIED., .F., .F., .F.,
 ( 6, 6 ),
 ( 6, 6 ),
 ( 2.618707526800000185, 4.366203223410000334 ),
 ( 0.000000000000000000, 0.5000000000000000000 ),
 .UNSPECIFIED. ) ;
#2926 = APPLICATION_PROTOCOL_DEFINITION ( 'draft international standard', 'automotive_design', 1998, #15339 ) ;
#2927 = CARTESIAN_POINT ( 'NONE',  ( -11.52017008789999863, -59.01533270489999694, -20.60511547919999842 ) ) ;
#2928 = CARTESIAN_POINT ( 'NONE',  ( 37.14627454077874802, -79.96476207452478491, -14.01644017333399006 ) ) ;
#2929 = FACE_OUTER_BOUND ( 'NONE', #6715, .T. ) ;
#2930 = CARTESIAN_POINT ( 'NONE',  ( -3.595691539529999758, -0.5000000000000000000, -6.581869214180000149 ) ) ;
#2931 = ORIENTED_EDGE ( 'NONE', *, *, #6076, .F. ) ;
#2932 = AXIS2_PLACEMENT_3D ( 'NONE', #23977, #8805, #22225 ) ;
#2933 = CARTESIAN_POINT ( 'NONE',  ( 47.01173857123500710, -74.16368351650025659, -1.843492029084275785 ) ) ;
#2934 = ORIENTED_EDGE ( 'NONE', *, *, #25396, .T. ) ;
#2935 = CARTESIAN_POINT ( 'NONE',  ( -13.01278816429999985, -34.63361166290000170, 19.94379924919999780 ) ) ;
#2936 = CARTESIAN_POINT ( 'NONE',  ( 9.024081099289999131, -19.49999992740000110, -18.94592230980000380 ) ) ;
#2937 = ORIENTED_EDGE ( 'NONE', *, *, #4873, .T. ) ;
#2938 = CIRCLE ( 'NONE', #21524, 0.4999999999999995559 ) ;
#2939 = CARTESIAN_POINT ( 'NONE',  ( 14.62247892739999955, -92.50000000000000000, 26.76626813769999913 ) ) ;
#2940 = EDGE_LOOP ( 'NONE', ( #3507, #27405, #10044, #887 ) ) ;
#2941 = CARTESIAN_POINT ( 'NONE',  ( -0.5413028987460000163, -57.47855601759999900, -23.35488904649999853 ) ) ;
#2942 = CARTESIAN_POINT ( 'NONE',  ( -10.48084080227152626, -19.47282323712138208, -20.22219529147017880 ) ) ;
#2943 = DIRECTION ( 'NONE',  ( 0.000000000000000000, -1.000000000000000000, 0.000000000000000000 ) ) ;
#2944 = CARTESIAN_POINT ( 'NONE',  ( -9.684721259419999839, -18.50000000000000000, -20.79699324019999906 ) ) ;
#2945 = CARTESIAN_POINT ( 'NONE',  ( 9.743056916871200457, -61.47481733543323656, -24.01218373186148369 ) ) ;
#2946 = ORIENTED_EDGE ( 'NONE', *, *, #22702, .F. ) ;
#2947 = CARTESIAN_POINT ( 'NONE',  ( -32.77174707999999725, -79.81706294759999309, -21.60034937969999902 ) ) ;
#2948 = DIRECTION ( 'NONE',  ( 1.000000000000000000, 0.000000000000000000, 0.000000000000000000 ) ) ;
#2949 = EDGE_CURVE ( 'NONE', #2641, #5527, #4546, .T. ) ;
#2950 = DIRECTION ( 'NONE',  ( 0.000000000000000000, 1.000000000000000000, 0.000000000000000000 ) ) ;
#2951 = VERTEX_POINT ( 'NONE', #2429 ) ;
#2952 = CARTESIAN_POINT ( 'NONE',  ( -14.42556421679999978, -101.1889999979999999, -2.978755036369999942 ) ) ;
#2953 = CARTESIAN_POINT ( 'NONE',  ( -12.61948338259999858, -101.5369810359999860, -9.836088610590000059 ) ) ;
#2954 = DIRECTION ( 'NONE',  ( 0.2414462220490750377, 0.000000000000000000, 0.9704142011833034598 ) ) ;
#2955 = VERTEX_POINT ( 'NONE', #9102 ) ;
#2956 = EDGE_CURVE ( 'NONE', #4122, #24455, #3876, .T. ) ;
#2957 = CARTESIAN_POINT ( 'NONE',  ( -16.12708711420000185, -99.55613392470000633, 6.748578067059999519 ) ) ;
#2958 = CIRCLE ( 'NONE', #12223, 0.4999999999999985567 ) ;
#2959 = CARTESIAN_POINT ( 'NONE',  ( 0.4290680484630000069, -99.83167681540000160, -17.32407653439999962 ) ) ;
#2960 = CYLINDRICAL_SURFACE ( 'NONE', #316, 53.34999999999998721 ) ;
#2961 = B_SPLINE_CURVE_WITH_KNOTS ( 'NONE', 5,
 ( #3420, #9956, #3143, #18728, #14479, #11999 ),
 .UNSPECIFIED., .F., .F.,
 ( 6, 6 ),
 ( 0.000000000000000000, 1.000000000000000000 ),
 .UNSPECIFIED. ) ;
#2962 = CARTESIAN_POINT ( 'NONE',  ( 23.53302756460000111, -92.50000000000000000, -18.47479450719999861 ) ) ;
#2963 = EDGE_CURVE ( 'NONE', #7997, #2790, #14065, .T. ) ;
#2964 = CARTESIAN_POINT ( 'NONE',  ( 22.17287391929999885, -57.47832537019999677, -7.362282751269999537 ) ) ;
#2965 = AXIS2_PLACEMENT_3D ( 'NONE', #21975, #15239, #6531 ) ;
#2966 = B_SPLINE_CURVE_WITH_KNOTS ( 'NONE', 3,
 ( #8331, #12416, #28446, #17524, #6153, #28589, #5872, #14888, #21331, #8481, #1389, #12984, #21894, #21471, #21748, #10231, #16962, #15023, #10788, #26412, #6442, #19146, #28033, #8073, #14752, #17382, #3698, #17234, #1799, #1525 ),
 .UNSPECIFIED., .F., .F.,
 ( 4, 1, 1, 1, 1, 2, 2, 1, 1, 1, 1, 2, 2, 2, 1, 1, 1, 1, 2, 2, 4 ),
 ( 0.000000000000000000, 0.1249999999999382994, 0.1874999999999068523, 0.2187499999998906153, 0.2343749999998821498, 0.2421874999998781253, 0.2499999999998741007, 0.3749999999998134825, 0.4374999999997830069, 0.4687499999997698508, 0.4843749999997616351, 0.4921874999997594147, 0.4999999999997573052, 0.6249999999997394307, 0.6874999999997285505, 0.7187499999997207789, 0.7343749999997143396, 0.7421874999997097877, 0.7460937499997096767, 0.7499999999997094546, 1.000000000000000000 ),
 .UNSPECIFIED. ) ;
#2967 = CARTESIAN_POINT ( 'NONE',  ( 26.91262686989999864, -67.03347986180000362, 1.647007874590000087 ) ) ;
#2968 = CARTESIAN_POINT ( 'NONE',  ( -10.54576762539999990, -18.85523517670000260, 19.18725863699999934 ) ) ;
#2969 = EDGE_LOOP ( 'NONE', ( #4500, #10238 ) ) ;
#2970 = FACE_OUTER_BOUND ( 'NONE', #7600, .T. ) ;
#2971 = CARTESIAN_POINT ( 'NONE',  ( 21.70215820849999844, -37.32353051909999664, -8.471236736359999853 ) ) ;
#2972 = CARTESIAN_POINT ( 'NONE',  ( 14.99988783689999927, -97.32097506000000919, 15.29756773239999923 ) ) ;
#2973 = ORIENTED_EDGE ( 'NONE', *, *, #20675, .T. ) ;
#2974 = DIRECTION ( 'NONE',  ( 1.000000000000000000, 0.000000000000000000, 0.000000000000000000 ) ) ;
#2975 = DIRECTION ( 'NONE',  ( 0.8775825618903722036, 0.000000000000000000, -0.4794255386042041156 ) ) ;
#2976 = DIRECTION ( 'NONE',  ( 0.000000000000000000, 1.000000000000000000, 0.000000000000000000 ) ) ;
#2977 = CARTESIAN_POINT ( 'NONE',  ( -8.226221597980000411, -100.1275643909999928, 14.47297520289999895 ) ) ;
#2978 = CARTESIAN_POINT ( 'NONE',  ( 26.90812271843742565, -72.79933240784657755, -9.897999932954709479 ) ) ;
#2979 = CARTESIAN_POINT ( 'NONE',  ( -10.36222220525591631, -93.92272615323433627, -23.21778344804266325 ) ) ;
#2980 = CARTESIAN_POINT ( 'NONE',  ( -40.87758256189999884, -66.42264973080000345, -0.4794255386039999456 ) ) ;
#2981 = AXIS2_PLACEMENT_3D ( 'NONE', #18313, #6951, #26770 ) ;
#2982 = CARTESIAN_POINT ( 'NONE',  ( 7.593106369170000036, -101.5369811139999996, 14.08349511319999969 ) ) ;
#2983 = CARTESIAN_POINT ( 'NONE',  ( -40.61475266853483390, -74.42768721757238382, 7.224488193796126723 ) ) ;
#2984 = CARTESIAN_POINT ( 'NONE',  ( 38.08875739639999836, -84.00000000000000000, -9.476764215410000247 ) ) ;
#2985 = CARTESIAN_POINT ( 'NONE',  ( -36.79999999999999716, -65.14977478849999670, 0.1732050807570000017 ) ) ;
#2986 = VERTEX_POINT ( 'NONE', #23391 ) ;
#2987 = CARTESIAN_POINT ( 'NONE',  ( -2.579071154395890630, -19.48685756504436384, -23.54263317592151594 ) ) ;
#2988 = EDGE_CURVE ( 'NONE', #20659, #23734, #8921, .T. ) ;
#2989 = CARTESIAN_POINT ( 'NONE',  ( 11.85750691279999991, -101.2995922080000071, -10.62593904340000073 ) ) ;
#2990 = CARTESIAN_POINT ( 'NONE',  ( -0.5335602090290000321, -52.63293862049999916, -23.18581005440000098 ) ) ;
#2991 = CARTESIAN_POINT ( 'NONE',  ( 12.71397128391526721, -96.41053128091054703, 17.27455293077128573 ) ) ;
#2992 = ADVANCED_FACE ( 'NONE', ( #16679 ), #1131, .T. ) ;
#2993 = CIRCLE ( 'NONE', #11392, 3.500000000000003109 ) ;
#2994 = CARTESIAN_POINT ( 'NONE',  ( -38.48840878260216414, -63.06523941402249278, -2.884620168990968292 ) ) ;
#2995 = CIRCLE ( 'NONE', #8084, 55.67692378859999991 ) ;
#2996 = LINE ( 'NONE', #972, #19416 ) ;
#2997 = CARTESIAN_POINT ( 'NONE',  ( 21.98941332889999956, -49.11505549560000361, -6.974892859150000568 ) ) ;
#2998 = EDGE_CURVE ( 'NONE', #24745, #10596, #5470, .T. ) ;
#2999 = DIRECTION ( 'NONE',  ( 0.000000000000000000, -1.000000000000000000, 0.000000000000000000 ) ) ;
#3000 = DIRECTION ( 'NONE',  ( 1.000000000000000000, 0.000000000000000000, 0.000000000000000000 ) ) ;
#3001 = ORIENTED_EDGE ( 'NONE', *, *, #15191, .T. ) ;
#3002 = EDGE_CURVE ( 'NONE', #4093, #8967, #20188, .T. ) ;
#3003 = CARTESIAN_POINT ( 'NONE',  ( 6.553154880760000189, -101.1030539030000028, 13.97735961090000067 ) ) ;
#3004 = CARTESIAN_POINT ( 'NONE',  ( -13.46646228700000059, -111.0000000000000000, -9.098096927170001180 ) ) ;
#3005 = AXIS2_PLACEMENT_3D ( 'NONE', #25732, #25170, #16694 ) ;
#3006 = CARTESIAN_POINT ( 'NONE',  ( -14.08127054510000065, -65.97310055630001102, 21.99106896830000224 ) ) ;
#3007 = CARTESIAN_POINT ( 'NONE',  ( 8.961089119540002201, -35.57149483869999784, -20.08449242119999667 ) ) ;
#3008 = LINE ( 'NONE', #833, #21963 ) ;
#3009 = FACE_OUTER_BOUND ( 'NONE', #25888, .T. ) ;
#3010 = CARTESIAN_POINT ( 'NONE',  ( 20.73064457619999956, -36.00000000000000000, -9.377114307539999416 ) ) ;
#3011 = CYLINDRICAL_SURFACE ( 'NONE', #16532, 5.000000000000000000 ) ;
#3012 = CIRCLE ( 'NONE', #6709, 0.5000000000000004441 ) ;
#3013 = CARTESIAN_POINT ( 'NONE',  ( 0.000000000000000000, -101.2530993010000060, 0.000000000000000000 ) ) ;
#3014 = DIRECTION ( 'NONE',  ( 0.9212380119587632032, 0.000000000000000000, -0.3889993898738990930 ) ) ;
#3015 = ORIENTED_EDGE ( 'NONE', *, *, #26696, .T. ) ;
#3016 = CONICAL_SURFACE ( 'NONE', #18352, 55.67692378859999280, 1.047197551199999799 ) ;
#3017 = CARTESIAN_POINT ( 'NONE',  ( -32.70203577369999692, -80.13412001289999864, -21.70611439569999845 ) ) ;
#3018 = DIRECTION ( 'NONE',  ( 0.000000000000000000, 1.000000000000000000, 0.000000000000000000 ) ) ;
#3019 = B_SPLINE_CURVE_WITH_KNOTS ( 'NONE', 3,
 ( #6918, #24836, #6473, #10954, #11553, #17696, #26582, #6626, #22359, #15487, #4434, #2255, #11101, #20014, #26739, #6775, #15636, #25555 ),
 .UNSPECIFIED., .F., .F.,
 ( 4, 2, 2, 2, 2, 2, 2, 2, 4 ),
 ( 0.000000000000000000, 0.1249999999999961142, 0.1874999999999941713, 0.2499999999999922284, 0.4999999999999658606, 0.6249999999999715783, 0.6874999999999747979, 0.7499999999999779066, 1.000000000000000000 ),
 .UNSPECIFIED. ) ;
#3020 = ORIENTED_EDGE ( 'NONE', *, *, #21743, .F. ) ;
#3021 = CARTESIAN_POINT ( 'NONE',  ( -30.44841632907958129, -92.65976904079269616, 1.773215843239575928 ) ) ;
#3022 = ORIENTED_EDGE ( 'NONE', *, *, #4676, .F. ) ;
#3023 = CARTESIAN_POINT ( 'NONE',  ( 0.1128683156097121110, -101.5740747342138803, -16.05694931027083783 ) ) ;
#3024 = B_SPLINE_CURVE_WITH_KNOTS ( 'NONE', 3,
 ( #8503, #17110, #14905, #4285, #12719, #22205, #26298, #2250, #13007, #28609, #11093, #8353, #13157, #79, #25998, #23814, #21631, #1681, #10521, #17254, #23959, #11853, #6772, #22652, #2840, #27022, #9524, #4720, #7354, #2693, #672, #26874, #11699, #17836, #15633, #24687, #16217, #25131, #5164, #8930, #24976, #26734, #5007, #22953, #11550, #14045, #11256, #20305, #24531, #13897, #13601, #2991, #18278, #18126, #7207, #4570, #233, #2553 ),
 .UNSPECIFIED., .F., .F.,
 ( 4, 2, 1, 1, 2, 2, 2, 1, 1, 2, 2, 1, 1, 2, 2, 1, 1, 1, 1, 1, 2, 2, 2, 2, 1, 1, 1, 2, 2, 2, 2, 1, 1, 1, 1, 2, 2, 4 ),
 ( 0.000000000000000000, 0.007812500000005218048, 0.01171875000000782707, 0.01367187500000852096, 0.01464843750001047946, 0.01562500000001243797, 0.02343750000001134856, 0.02734375000001080386, 0.02929687500001182041, 0.03027343750001156020, 0.03125000000001129652, 0.04687500000001742356, 0.05468750000002103873, 0.05859375000002389755, 0.06250000000002675637, 0.09375000000004667100, 0.1093750000000555112, 0.1171875000000596329, 0.1210937500000619227, 0.1230468750000631023, 0.1240234375000626582, 0.1250000000000622002, 0.1875000000001452727, 0.2187500000001867950, 0.2343750000002075562, 0.2421875000002177147, 0.2460937500002227940, 0.2480468750002245704, 0.2500000000002263190, 0.3750000000002354783, 0.4375000000002389200, 0.4687500000002393086, 0.4843750000002381428, 0.4921875000002358669, 0.4960937500002358669, 0.4980468750002362555, 0.5000000000002366995, 1.000000000000000000 ),
 .UNSPECIFIED. ) ;
#3025 = DIRECTION ( 'NONE',  ( 0.000000000000000000, 1.000000000000000000, 0.000000000000000000 ) ) ;
#3026 = CARTESIAN_POINT ( 'NONE',  ( -12.83089869019999973, -99.70407914540000149, -11.44895565849999919 ) ) ;
#3027 = ADVANCED_FACE ( 'NONE', ( #16547 ), #3570, .T. ) ;
#3028 = VECTOR ( 'NONE', #9528, 999.9999999999998863 ) ;
#3029 = CARTESIAN_POINT ( 'NONE',  ( 23.70206688740000089, -94.36515553530000489, -7.408338407089999578 ) ) ;
#3030 = EDGE_CURVE ( 'NONE', #7301, #26062, #17089, .T. ) ;
#3031 = DIRECTION ( 'NONE',  ( 0.8086044598489942059, 0.000000000000000000, -0.5883526387399961033 ) ) ;
#3032 = CARTESIAN_POINT ( 'NONE',  ( 13.94245834920000071, -96.73974214399999028, -16.03213923699999910 ) ) ;
#3033 = EDGE_LOOP ( 'NONE', ( #27867, #12027, #6228, #27507 ) ) ;
#3034 = AXIS2_PLACEMENT_3D ( 'NONE', #12319, #16700, #27659 ) ;
#3035 = CARTESIAN_POINT ( 'NONE',  ( 0.000000000000000000, -2.000000000000000000, 0.000000000000000000 ) ) ;
#3036 = CARTESIAN_POINT ( 'NONE',  ( 8.508195433830001875, -34.61672952569999495, -20.76917450910000085 ) ) ;
#3037 = DIRECTION ( 'NONE',  ( 0.000000000000000000, 1.000000000000000000, 0.000000000000000000 ) ) ;
#3038 = LINE ( 'NONE', #3447, #27692 ) ;
#3039 = CARTESIAN_POINT ( 'NONE',  ( 15.77847589470000145, -100.9405348700000076, 2.296806114620000283 ) ) ;
#3040 = ORIENTED_EDGE ( 'NONE', *, *, #9105, .T. ) ;
#3041 = EDGE_CURVE ( 'NONE', #22316, #26221, #12952, .T. ) ;
#3042 = AXIS2_PLACEMENT_3D ( 'NONE', #9106, #15957, #402 ) ;
#3043 = ORIENTED_EDGE ( 'NONE', *, *, #7541, .T. ) ;
#3044 = FACE_OUTER_BOUND ( 'NONE', #17610, .T. ) ;
#3045 = CARTESIAN_POINT ( 'NONE',  ( -39.50000000000000000, -63.30468293320000583, -2.309401076760000393 ) ) ;
#3046 = CARTESIAN_POINT ( 'NONE',  ( -11.35954001540000036, -74.50000000000000000, 45.25000000000000000 ) ) ;
#3047 = CARTESIAN_POINT ( 'NONE',  ( 1.312670351570000005, -94.71480777040000021, 24.32357384970000069 ) ) ;
#3048 = VERTEX_POINT ( 'NONE', #3297 ) ;
#3049 = CIRCLE ( 'NONE', #15089, 3.500000000000003109 ) ;
#3050 = CARTESIAN_POINT ( 'NONE',  ( -28.44467018057688534, -93.18010901174839944, 2.040524032743244565 ) ) ;
#3051 = LINE ( 'NONE', #16128, #16794 ) ;
#3052 = CARTESIAN_POINT ( 'NONE',  ( -1.869165715791609950, -94.36683344921111427, 24.51523021183322726 ) ) ;
#3053 = ORIENTED_EDGE ( 'NONE', *, *, #27993, .T. ) ;
#3054 = CARTESIAN_POINT ( 'NONE',  ( 7.233314584209180609, -74.35734738468387661, -40.52471375186235036 ) ) ;
#3055 = DIRECTION ( 'NONE',  ( 0.4794255386042037270, 0.000000000000000000, 0.8775825618903724257 ) ) ;
#3056 = VERTEX_POINT ( 'NONE', #12158 ) ;
#3057 = CARTESIAN_POINT ( 'NONE',  ( 0.000000000000000000, -90.50000000000000000, 0.000000000000000000 ) ) ;
#3058 = CONICAL_SURFACE ( 'NONE', #9988, 8.099999999999997868, 0.7853981633970000820 ) ;
#3059 = CARTESIAN_POINT ( 'NONE',  ( -2.790529132629999687, -64.24504218810000111, -26.36014162090000212 ) ) ;
#3060 = CARTESIAN_POINT ( 'NONE',  ( -16.10242507159999903, -71.49765472880000061, 23.35251611179999998 ) ) ;
#3061 = ORIENTED_EDGE ( 'NONE', *, *, #3383, .T. ) ;
#3062 = DIRECTION ( 'NONE',  ( 1.000000000000000000, 0.000000000000000000, 0.000000000000000000 ) ) ;
#3063 = ADVANCED_FACE ( 'NONE', ( #7681 ), #1980, .T. ) ;
#3064 = CARTESIAN_POINT ( 'NONE',  ( -15.23833467649999918, -101.0223712829999982, 2.799529863349999648 ) ) ;
#3065 = CARTESIAN_POINT ( 'NONE',  ( 23.60463849679999626, -59.01533270489999694, 0.3257977875450000504 ) ) ;
#3066 = CARTESIAN_POINT ( 'NONE',  ( -21.01599529309999781, -64.93834962409999889, 13.98666844150000088 ) ) ;
#3067 = EDGE_LOOP ( 'NONE', ( #22611, #6190, #7662, #12901 ) ) ;
#3068 = CARTESIAN_POINT ( 'NONE',  ( -18.99800347089999875, -26.09861276229999660, 11.61132478269999879 ) ) ;
#3069 = CARTESIAN_POINT ( 'NONE',  ( -0.9991794988550000145, -19.46390881170000142, -22.01488094909999660 ) ) ;
#3070 = CARTESIAN_POINT ( 'NONE',  ( -7.921025165613940544, -100.1994045928917956, 15.20254870833589145 ) ) ;
#3071 = ORIENTED_EDGE ( 'NONE', *, *, #21876, .F. ) ;
#3072 = EDGE_CURVE ( 'NONE', #15581, #4465, #5696, .T. ) ;
#3073 = CARTESIAN_POINT ( 'NONE',  ( -11.74977568899999980, -18.50000000000000000, 18.05674360140000445 ) ) ;
#3074 = TOROIDAL_SURFACE ( 'NONE', #19326, 30.50381168839999901, 2.000000000000000000 ) ;
#3075 = CARTESIAN_POINT ( 'NONE',  ( 23.41692821889999720, -63.52052399810000338, 10.59810502480000061 ) ) ;
#3076 = CARTESIAN_POINT ( 'NONE',  ( -38.62700573890000300, -65.19264941160000149, -2.813424548380000001 ) ) ;
#3077 = CARTESIAN_POINT ( 'NONE',  ( 15.76345192703606024, -101.3038909014199760, 4.015656894647334774 ) ) ;
#3078 = DIRECTION ( 'NONE',  ( 0.000000000000000000, 1.000000000000000000, 0.000000000000000000 ) ) ;
#3079 = VERTEX_POINT ( 'NONE', #990 ) ;
#3080 = DIRECTION ( 'NONE',  ( 1.000000000000000000, 0.000000000000000000, 0.000000000000000000 ) ) ;
#3081 = CARTESIAN_POINT ( 'NONE',  ( -11.18016241690000001, -57.44036991850000362, -21.74842387279999656 ) ) ;
#3082 = CARTESIAN_POINT ( 'NONE',  ( -29.76178938840000043, -91.50000000000000000, 6.669774538800000485 ) ) ;
#3083 = DIRECTION ( 'NONE',  ( 0.4794255386042040601, 0.000000000000000000, 0.8775825618903720926 ) ) ;
#3084 = ORIENTED_EDGE ( 'NONE', *, *, #4007, .F. ) ;
#3085 = EDGE_CURVE ( 'NONE', #21366, #10298, #9835, .T. ) ;
#3086 = DIRECTION ( 'NONE',  ( 0.000000000000000000, -1.000000000000000000, 0.000000000000000000 ) ) ;
#3087 = ORIENTED_EDGE ( 'NONE', *, *, #16278, .T. ) ;
#3088 = CARTESIAN_POINT ( 'NONE',  ( -11.42167949289999918, -34.66886610320000273, 19.55066939339999976 ) ) ;
#3089 = CARTESIAN_POINT ( 'NONE',  ( -5.487411647150000071, -100.8733988930000010, 14.73625039430000072 ) ) ;
#3090 = ORIENTED_EDGE ( 'NONE', *, *, #19002, .T. ) ;
#3091 = CARTESIAN_POINT ( 'NONE',  ( 39.04162410880000067, -73.95638562439998509, 7.432628554209999905 ) ) ;
#3092 = CARTESIAN_POINT ( 'NONE',  ( -10.71547162644561624, -19.46656777169255292, -19.55512608735946500 ) ) ;
#3093 = CARTESIAN_POINT ( 'NONE',  ( 7.120909764619999412E-15, -74.50000000000000000, 40.00000000000000000 ) ) ;
#3094 = CARTESIAN_POINT ( 'NONE',  ( -9.797255285709999484, -18.50000000000000000, -21.36865465820000054 ) ) ;
#3095 = CARTESIAN_POINT ( 'NONE',  ( -10.20110288159999890, -84.50000000000000000, -41.00000000000000000 ) ) ;
#3096 = ORIENTED_EDGE ( 'NONE', *, *, #19405, .F. ) ;
#3097 = CARTESIAN_POINT ( 'NONE',  ( 0.000000000000000000, -92.50000000000000000, 29.91857981989999971 ) ) ;
#3098 = ADVANCED_FACE ( 'NONE', ( #27640 ), #5878, .T. ) ;
#3099 = CARTESIAN_POINT ( 'NONE',  ( 18.39061537769999788, -98.53908914310000000, 3.638009050179999981 ) ) ;
#3100 = CARTESIAN_POINT ( 'NONE',  ( -20.48363899790000175, -93.24064650399999721, 16.32317473610000036 ) ) ;
#3101 = DIRECTION ( 'NONE',  ( -0.9999381462442837876, 0.000000000000000000, 0.01112221585590941926 ) ) ;
#3102 = EDGE_LOOP ( 'NONE', ( #16143, #17346, #14193, #8940 ) ) ;
#3103 = AXIS2_PLACEMENT_3D ( 'NONE', #23067, #23199, #2667 ) ;
#3104 = CARTESIAN_POINT ( 'NONE',  ( -38.23742073339541037, -63.33368279749979024, -1.408367766111304098 ) ) ;
#3105 = CARTESIAN_POINT ( 'NONE',  ( 7.708049625630000179, -24.50935433020000076, -20.82960214859999937 ) ) ;
#3106 = CARTESIAN_POINT ( 'NONE',  ( 0.000000000000000000, -26.59999999999999787, 0.000000000000000000 ) ) ;
#3107 = EDGE_LOOP ( 'NONE', ( #19832, #5934, #15126, #22723, #28574 ) ) ;
#3108 = CARTESIAN_POINT ( 'NONE',  ( -17.84952382330000020, -94.52419442680000827, 16.07137070119999933 ) ) ;
#3109 = CARTESIAN_POINT ( 'NONE',  ( -19.45061163789999981, -45.99930305819999887, 12.20452280910000020 ) ) ;
#3110 = CARTESIAN_POINT ( 'NONE',  ( 30.63102016379999881, -73.01580299129999219, -23.62320562749999908 ) ) ;
#3111 = CARTESIAN_POINT ( 'NONE',  ( 22.38434844160000026, -60.58720252940000250, -7.752233810359999922 ) ) ;
#3112 = CARTESIAN_POINT ( 'NONE',  ( 25.57917931149999902, -64.69849622489999774, 1.120748734570000016 ) ) ;
#3113 = CARTESIAN_POINT ( 'NONE',  ( -10.60770804610000084, -19.15810967940000253, 19.29995473580000009 ) ) ;
#3114 = EDGE_LOOP ( 'NONE', ( #25608, #26871, #2766, #14276 ) ) ;
#3115 = ADVANCED_FACE ( 'NONE', ( #2426 ), #10970, .F. ) ;
#3116 = CARTESIAN_POINT ( 'NONE',  ( -39.48689401896172768, -73.68677077079325954, -7.232334316218844705 ) ) ;
#3117 = EDGE_CURVE ( 'NONE', #22747, #17308, #17717, .T. ) ;
#3118 = CARTESIAN_POINT ( 'NONE',  ( 21.72885701919999946, -37.62355108940000292, -8.376330313129999539 ) ) ;
#3119 = DIRECTION ( 'NONE',  ( 0.4794255386042036715, 0.000000000000000000, 0.8775825618903724257 ) ) ;
#3120 = VERTEX_POINT ( 'NONE', #21940 ) ;
#3121 = CARTESIAN_POINT ( 'NONE',  ( 25.26718046270000073, -45.73899999920000425, 6.129403842640000377 ) ) ;
#3122 = CARTESIAN_POINT ( 'NONE',  ( -10.89815191770000169, -18.50000000000000000, -17.99090140869999743 ) ) ;
#3123 = CARTESIAN_POINT ( 'NONE',  ( -17.07013490150000123, -92.69457892460000892, -23.53491425640000045 ) ) ;
#3124 = CARTESIAN_POINT ( 'NONE',  ( 46.25000000000000000, -79.00000000000000000, -14.75000000000000000 ) ) ;
#3125 = ADVANCED_FACE ( 'NONE', ( #2273 ), #11745, .F. ) ;
#3126 = CARTESIAN_POINT ( 'NONE',  ( 7.584268293420000084, -101.6484612600000048, 14.08825297070000104 ) ) ;
#3127 = VERTEX_POINT ( 'NONE', #8374 ) ;
#3128 = CARTESIAN_POINT ( 'NONE',  ( 0.000000000000000000, -102.5000000000000000, 0.000000000000000000 ) ) ;
#3129 = B_SPLINE_CURVE_WITH_KNOTS ( 'NONE', 5,
 ( #7096, #3026, #995, #9838, #16404, #27494, #9691, #11880, #22678, #27050, #4898, #7383 ),
 .UNSPECIFIED., .F., .F.,
 ( 6, 3, 3, 6 ),
 ( 0.000000000000000000, 0.4964111757615384257, 0.7833083924331027958, 1.000000000000000000 ),
 .UNSPECIFIED. ) ;
#3130 = DIRECTION ( 'NONE',  ( -0.000000000000000000, 1.000000000000000000, 0.000000000000000000 ) ) ;
#3131 = CARTESIAN_POINT ( 'NONE',  ( 11.52544325100000044, -97.14975610999999844, -17.91795520970000055 ) ) ;
#3132 = VERTEX_POINT ( 'NONE', #17279 ) ;
#3133 = DIRECTION ( 'NONE',  ( 0.000000000000000000, -1.000000000000000000, 0.000000000000000000 ) ) ;
#3134 = CARTESIAN_POINT ( 'NONE',  ( 11.48112218699999865, -101.1411470150000014, -10.24881966589999926 ) ) ;
#3135 = CARTESIAN_POINT ( 'NONE',  ( -0.5372044051000000042, -32.73130089789999886, -22.49056468509999718 ) ) ;
#3136 = CARTESIAN_POINT ( 'NONE',  ( -17.71736434265992699, -92.62800705135339285, 24.82640349161211901 ) ) ;
#3137 = CARTESIAN_POINT ( 'NONE',  ( -27.18988201479999844, -29.29844555429999886, -49.77074518290000071 ) ) ;
#3138 = CARTESIAN_POINT ( 'NONE',  ( 12.01314480165432563, -101.6484611540000031, -10.56820974955409298 ) ) ;
#3139 = FACE_OUTER_BOUND ( 'NONE', #7188, .T. ) ;
#3140 = DIRECTION ( 'NONE',  ( 1.000000000000000000, 0.000000000000000000, 0.000000000000000000 ) ) ;
#3141 = VERTEX_POINT ( 'NONE', #22090 ) ;
#3142 = CARTESIAN_POINT ( 'NONE',  ( 6.902456655579999989, -101.3852859389999992, 14.42727485510000029 ) ) ;
#3143 = CARTESIAN_POINT ( 'NONE',  ( -21.85457041760000152, -74.50000000000000000, -32.66023292159999869 ) ) ;
#3144 = CARTESIAN_POINT ( 'NONE',  ( -11.20160157070000118, -94.96737615119999987, -21.25938373800000036 ) ) ;
#3145 = CARTESIAN_POINT ( 'NONE',  ( 8.744948820599999451, -35.57625659020000342, -20.62426134429999891 ) ) ;
#3146 = DIRECTION ( 'NONE',  ( 1.000000000000000000, 0.000000000000000000, 0.000000000000000000 ) ) ;
#3147 = B_SPLINE_CURVE_WITH_KNOTS ( 'NONE', 5,
 ( #240, #6919, #6627, #9085, #15785, #4726 ),
 .UNSPECIFIED., .F., .F.,
 ( 6, 6 ),
 ( 0.000000000000000000, 1.000000000000000000 ),
 .UNSPECIFIED. ) ;
#3148 = CARTESIAN_POINT ( 'NONE',  ( 46.25000000000000000, -77.00000000000000000, -13.75000000000000000 ) ) ;
#3149 = ADVANCED_FACE ( 'NONE', ( #8660 ), #2132, .T. ) ;
#3150 = CARTESIAN_POINT ( 'NONE',  ( -41.45000000000000284, -65.00000000000000000, -2.857883832489999776 ) ) ;
#3151 = EDGE_CURVE ( 'NONE', #3865, #27292, #6633, .T. ) ;
#3152 = DIRECTION ( 'NONE',  ( 0.000000000000000000, 1.000000000000000000, 0.000000000000000000 ) ) ;
#3153 = ORIENTED_EDGE ( 'NONE', *, *, #15812, .T. ) ;
#3154 = CARTESIAN_POINT ( 'NONE',  ( 32.73121282881579219, -74.00000011846343284, -20.86988175080205465 ) ) ;
#3155 = CARTESIAN_POINT ( 'NONE',  ( 0.000000000000000000, -10.00000000000000000, 0.000000000000000000 ) ) ;
#3156 = ORIENTED_EDGE ( 'NONE', *, *, #5885, .F. ) ;
#3157 = ADVANCED_FACE ( 'NONE', ( #19601 ), #17289, .F. ) ;
#3158 = AXIS2_PLACEMENT_3D ( 'NONE', #10884, #19794, #26509 ) ;
#3159 = CARTESIAN_POINT ( 'NONE',  ( -10.20110288159999890, -74.00000000000000000, 41.00000000000000000 ) ) ;
#3160 = EDGE_CURVE ( 'NONE', #22409, #927, #19190, .T. ) ;
#3161 = ORIENTED_EDGE ( 'NONE', *, *, #15006, .F. ) ;
#3162 = CARTESIAN_POINT ( 'NONE',  ( 0.5651181260435291787, -100.9609609850402308, -16.52593752888986245 ) ) ;
#3163 = CYLINDRICAL_SURFACE ( 'NONE', #19103, 5.000000000000001776 ) ;
#3164 = PLANE ( 'NONE',  #18309 ) ;
#3165 = CARTESIAN_POINT ( 'NONE',  ( 21.89559254579999958, -72.72322124080000094, -31.02685804430000260 ) ) ;
#3166 = FACE_OUTER_BOUND ( 'NONE', #20183, .T. ) ;
#3167 = CARTESIAN_POINT ( 'NONE',  ( 23.92053897610000135, -93.00000000000000000, -18.92241567810000191 ) ) ;
#3168 = B_SPLINE_SURFACE_WITH_KNOTS ( 'NONE', 5, 5, ( 
 ( #4001, #21779, #1832, #10673, #8513, #20312 ),
 ( #5017, #24840, #26744, #13904, #383, #8937 ),
 ( #89, #18286, #27032, #9227, #13460, #534 ),
 ( #4879, #681, #9384, #7075, #18135, #4582 ),
 ( #6923, #2846, #11709, #22661, #15935, #20623 ),
 ( #22808, #17847, #16083, #6779, #15640, #2701 ) ),
 .UNSPECIFIED., .F., .F., .F.,
 ( 6, 6 ),
 ( 6, 6 ),
 ( 6.713731535029999975, 7.329014384030000606 ),
 ( 0.000000000000000000, 0.5000000000000000000 ),
 .UNSPECIFIED. ) ;
#3169 = CARTESIAN_POINT ( 'NONE',  ( -12.09704001540000107, -80.00000000000000000, 47.10905722069999513 ) ) ;
#3170 = CARTESIAN_POINT ( 'NONE',  ( 8.509522500270000123, -31.58327295760000197, -20.65664638119999807 ) ) ;
#3171 = CARTESIAN_POINT ( 'NONE',  ( 23.14416696340000001, -57.40875702419999982, 10.37855830930000067 ) ) ;
#3172 = FILL_AREA_STYLE ('',( #1003 ) ) ;
#3173 = EDGE_LOOP ( 'NONE', ( #4142, #13134, #23756, #10527 ) ) ;
#3174 = AXIS2_PLACEMENT_3D ( 'NONE', #20082, #26799, #13669 ) ;
#3175 = CARTESIAN_POINT ( 'NONE',  ( -41.33431406180000067, -65.21397798589998729, 2.791092524920000262 ) ) ;
#3176 = EDGE_LOOP ( 'NONE', ( #12884, #5708, #1307, #23802 ) ) ;
#3177 = CARTESIAN_POINT ( 'NONE',  ( -2.488381974000000163, -57.43018231299999599, -24.62424122550000050 ) ) ;
#3178 = CARTESIAN_POINT ( 'NONE',  ( -2.575778565979999879, -97.41042627209999694, 21.30187829299999791 ) ) ;
#3179 = CARTESIAN_POINT ( 'NONE',  ( 2.583222064299999676, -94.01600108440000270, 25.18845981800000189 ) ) ;
#3180 = EDGE_LOOP ( 'NONE', ( #12404, #27489, #3986, #18825 ) ) ;
#3181 = EDGE_CURVE ( 'NONE', #2510, #25473, #17769, .T. ) ;
#3182 = CARTESIAN_POINT ( 'NONE',  ( -7.627568735119999666, -74.00000000000000000, 38.62788659690000515 ) ) ;
#3183 = LINE ( 'NONE', #14103, #27526 ) ;
#3184 = DIRECTION ( 'NONE',  ( 0.000000000000000000, 1.000000000000000000, 0.000000000000000000 ) ) ;
#3185 = ORIENTED_EDGE ( 'NONE', *, *, #14572, .F. ) ;
#3186 = FACE_OUTER_BOUND ( 'NONE', #2506, .T. ) ;
#3187 = CARTESIAN_POINT ( 'NONE',  ( -1.598721155459999804E-14, -15.00000000000000000, 50.00000000000000000 ) ) ;
#3188 = EDGE_CURVE ( 'NONE', #7412, #13154, #5090, .T. ) ;
#3189 = VERTEX_POINT ( 'NONE', #25154 ) ;
#3190 = CIRCLE ( 'NONE', #12020, 16.00000000000000000 ) ;
#3191 = CARTESIAN_POINT ( 'NONE',  ( 26.73327916010000038, -93.00000450890000536, -12.41348522350000039 ) ) ;
#3192 = CIRCLE ( 'NONE', #19444, 0.5000000000000013323 ) ;
#3193 = CARTESIAN_POINT ( 'NONE',  ( -3.058911596290000201, -72.82938648530000592, -28.52031795890000154 ) ) ;
#3194 = CARTESIAN_POINT ( 'NONE',  ( -16.01432518160000029, -72.70510571239999820, 23.73092384619999962 ) ) ;
#3195 = ORIENTED_EDGE ( 'NONE', *, *, #5913, .T. ) ;
#3196 = LINE ( 'NONE', #16441, #12518 ) ;
#3197 = CARTESIAN_POINT ( 'NONE',  ( -15.84587239670000258, -101.4177331369999990, 3.264600553649999792 ) ) ;
#3198 = CARTESIAN_POINT ( 'NONE',  ( -20.15147649909999927, -62.06884231739999791, 13.30139272559999952 ) ) ;
#3199 = EDGE_LOOP ( 'NONE', ( #20621, #26057, #23347, #1933 ) ) ;
#3200 = VECTOR ( 'NONE', #1123, 1000.000000000000000 ) ;
#3201 = CARTESIAN_POINT ( 'NONE',  ( -0.5567007213574344249, -26.09861274200153147, -22.25841601198301944 ) ) ;
#3202 = CARTESIAN_POINT ( 'NONE',  ( -2.650567523169999884, -19.17792668139999890, -23.73795088580000012 ) ) ;
#3203 = CARTESIAN_POINT ( 'NONE',  ( -7.919901001398579332, -100.1517898586247952, 15.24641937776444323 ) ) ;
#3204 = ORIENTED_EDGE ( 'NONE', *, *, #6439, .F. ) ;
#3205 = CYLINDRICAL_SURFACE ( 'NONE', #16537, 10.00000000000000000 ) ;
#3206 = B_SPLINE_CURVE_WITH_KNOTS ( 'NONE', 3,
 ( #15249, #11473, #22725, #11775 ),
 .UNSPECIFIED., .F., .F.,
 ( 4, 4 ),
 ( 0.000000000000000000, 1.000000000000000000 ),
 .UNSPECIFIED. ) ;
#3207 = FACE_OUTER_BOUND ( 'NONE', #25041, .T. ) ;
#3208 = CARTESIAN_POINT ( 'NONE',  ( 16.76861568428709504, -99.99762666420065216, 4.276776115527929356 ) ) ;
#3209 = CARTESIAN_POINT ( 'NONE',  ( -4.234949299205656992, -72.18744871743631109, -28.56489076017935957 ) ) ;
#3210 = VERTEX_POINT ( 'NONE', #14069 ) ;
#3211 = AXIS2_PLACEMENT_3D ( 'NONE', #20237, #24170, #6838 ) ;
#3212 = EDGE_CURVE ( 'NONE', #28629, #16297, #6669, .T. ) ;
#3213 = CARTESIAN_POINT ( 'NONE',  ( 26.16632615330000178, -71.08692331999999681, -10.19695628250000041 ) ) ;
#3214 = FACE_OUTER_BOUND ( 'NONE', #27610, .T. ) ;
#3215 = ORIENTED_EDGE ( 'NONE', *, *, #2210, .T. ) ;
#3216 = EDGE_CURVE ( 'NONE', #26221, #16034, #5553, .T. ) ;
#3217 = CARTESIAN_POINT ( 'NONE',  ( -6.665307709260000379, -93.00000000000000000, -13.13558364449999871 ) ) ;
#3218 = CARTESIAN_POINT ( 'NONE',  ( 47.16974535660000356, -74.50000000000000000, -1.075756255579999987 ) ) ;
#3219 = ORIENTED_EDGE ( 'NONE', *, *, #6343, .T. ) ;
#3220 = FACE_OUTER_BOUND ( 'NONE', #17799, .T. ) ;
#3221 = CARTESIAN_POINT ( 'NONE',  ( -5.452248121450000262, -100.9938510739999913, 14.54082342019999885 ) ) ;
#3222 = ORIENTED_EDGE ( 'NONE', *, *, #5155, .F. ) ;
#3223 = EDGE_CURVE ( 'NONE', #4878, #139, #17155, .T. ) ;
#3224 = CARTESIAN_POINT ( 'NONE',  ( 46.12332288628675769, -80.00000000113583098, -4.489694476353789376 ) ) ;
#3225 = LINE ( 'NONE', #9472, #4301 ) ;
#3226 = EDGE_CURVE ( 'NONE', #16528, #18883, #11881, .T. ) ;
#3227 = EDGE_LOOP ( 'NONE', ( #7343, #12352, #7592, #21982 ) ) ;
#3228 = DIRECTION ( 'NONE',  ( 0.000000000000000000, 1.000000000000000000, 0.000000000000000000 ) ) ;
#3229 = CARTESIAN_POINT ( 'NONE',  ( -10.51533464487888736, -19.47102514969543208, -20.05824860045767721 ) ) ;
#3230 = DIRECTION ( 'NONE',  ( 1.000000000000000000, 0.000000000000000000, 0.000000000000000000 ) ) ;
#3231 = CARTESIAN_POINT ( 'NONE',  ( 9.476764215410000247, -82.25000000000000000, 38.08875739639999836 ) ) ;
#3232 = LINE ( 'NONE', #12091, #14814 ) ;
#3233 = VERTEX_POINT ( 'NONE', #7804 ) ;
#3234 = TOROIDAL_SURFACE ( 'NONE', #7434, 18.14285714289999873, 0.5000000000000000000 ) ;
#3235 = AXIS2_PLACEMENT_3D ( 'NONE', #3169, #9697, #15967 ) ;
#3236 = CARTESIAN_POINT ( 'NONE',  ( -32.66023292159999869, -79.50000000000000000, -21.85457041760000152 ) ) ;
#3237 = CARTESIAN_POINT ( 'NONE',  ( 21.23910705489999984, -96.83679385140000306, 0.8485770364149999301 ) ) ;
#3238 = FACE_OUTER_BOUND ( 'NONE', #3114, .T. ) ;
#3239 = ORIENTED_EDGE ( 'NONE', *, *, #14018, .F. ) ;
#3240 = CARTESIAN_POINT ( 'NONE',  ( 29.74110577495378749, -92.77521214521595994, 6.761509561029908078 ) ) ;
#3241 = CARTESIAN_POINT ( 'NONE',  ( -14.87113501819999861, -65.53648121479999133, 22.45123099050000093 ) ) ;
#3242 = ORIENTED_EDGE ( 'NONE', *, *, #10014, .T. ) ;
#3243 = DIRECTION ( 'NONE',  ( 0.4794255386042040601, 0.000000000000000000, 0.8775825618903720926 ) ) ;
#3244 = EDGE_CURVE ( 'NONE', #25772, #28370, #6469, .T. ) ;
#3245 = CARTESIAN_POINT ( 'NONE',  ( -19.89280855559999850, -39.30675845289999870, 14.46928939670000069 ) ) ;
#3246 = CARTESIAN_POINT ( 'NONE',  ( -8.124727395691921927, -99.57060688036840190, 15.34961553150924374 ) ) ;
#3247 = CARTESIAN_POINT ( 'NONE',  ( 28.93927510940000047, -73.97465399030001265, -26.57194658529999742 ) ) ;
#3248 = DIRECTION ( 'NONE',  ( 0.000000000000000000, -1.000000000000000000, 0.000000000000000000 ) ) ;
#3249 = CARTESIAN_POINT ( 'NONE',  ( 25.82503148889999878, -66.16381828919999464, 0.7716244649270000977 ) ) ;
#3250 = CIRCLE ( 'NONE', #26494, 0.7500000000000006661 ) ;
#3251 = VECTOR ( 'NONE', #19320, 1000.000000000000000 ) ;
#3252 = AXIS2_PLACEMENT_3D ( 'NONE', #11099, #28743, #8782 ) ;
#3254 = VERTEX_POINT ( 'NONE', #18882 ) ;
#3253 = ADVANCED_FACE ( 'NONE', ( #5468 ), #6947, .T. ) ;
#3255 = EDGE_CURVE ( 'NONE', #14724, #23155, #12041, .T. ) ;
#3256 = DIRECTION ( 'NONE',  ( 1.000000000000000000, 0.000000000000000000, 0.000000000000000000 ) ) ;
#3257 = B_SPLINE_CURVE_WITH_KNOTS ( 'NONE', 5,
 ( #24158, #22264, #8838, #17755, #26637, #4486, #13359, #27370, #20517 ),
 .UNSPECIFIED., .F., .F.,
 ( 6, 3, 6 ),
 ( 0.000000000000000000, 0.5000000000000000000, 1.000000000000000000 ),
 .UNSPECIFIED. ) ;
#3258 = CARTESIAN_POINT ( 'NONE',  ( 21.61390653610000001, -37.84383064499999705, -8.096276181549999507 ) ) ;
#3259 = CARTESIAN_POINT ( 'NONE',  ( 7.601090357100000361, -101.6484612010000035, 14.07919707850000002 ) ) ;
#3260 = ORIENTED_EDGE ( 'NONE', *, *, #25866, .F. ) ;
#3261 = CARTESIAN_POINT ( 'NONE',  ( 7.973708284010000646, -18.50000000000000000, -19.11504000820000115 ) ) ;
#3262 = CARTESIAN_POINT ( 'NONE',  ( 25.34421590619999876, -10.95575221240000019, 46.39227603280000523 ) ) ;
#3263 = FILL_AREA_STYLE_COLOUR ( '', #21287 ) ;
#3264 = B_SPLINE_CURVE_WITH_KNOTS ( 'NONE', 3,
 ( #13402, #32, #631, #18384, #17793, #4387, #13256, #22307, #22163, #26683, #2353, #5408, #11808, #14560, #23466, #14291, #21144, #27574, #25650, #27833, #14001, #9763, #23187, #1200, #7613, #16755, #10035, #16477, #1066, #18949, #18525, #7873, #25238, #25084, #20720, #5680, #779, #7467 ),
 .UNSPECIFIED., .F., .F.,
 ( 4, 2, 2, 1, 1, 1, 1, 2, 2, 2, 2, 1, 1, 1, 2, 2, 2, 2, 1, 1, 1, 2, 2, 4 ),
 ( 0.000000000000000000, 0.1250000000001522948, 0.1875000000002285672, 0.2187500000002666756, 0.2343750000002870482, 0.2421875000002955969, 0.2460937500003001766, 0.2480468750003007039, 0.2500000000003012590, 0.3750000000002757794, 0.4375000000002619571, 0.4687500000002539080, 0.4843750000002494671, 0.4921875000002482459, 0.4960937500002480793, 0.5000000000002479128, 0.6250000000002012834, 0.6875000000001786349, 0.7187500000001665335, 0.7343750000001604272, 0.7421875000001573186, 0.7460937500001556533, 0.7500000000001538769, 1.000000000000000000 ),
 .UNSPECIFIED. ) ;
#3265 = CARTESIAN_POINT ( 'NONE',  ( 7.517162733169999278, -40.74985578699999422, -21.57753409760000096 ) ) ;
#3266 = CARTESIAN_POINT ( 'NONE',  ( 7.458107840580000314, -101.1716783650000053, 13.85390195080000098 ) ) ;
#3267 = VERTEX_POINT ( 'NONE', #27767 ) ;
#3268 = CARTESIAN_POINT ( 'NONE',  ( -43.24908333233128133, -65.12255024416487004, -0.1339731005256810936 ) ) ;
#3269 = DIRECTION ( 'NONE',  ( -0.000000000000000000, 1.000000000000000000, 0.000000000000000000 ) ) ;
#3270 = CARTESIAN_POINT ( 'NONE',  ( 11.00987699500000083, -96.97547176729999308, -17.68222522410000153 ) ) ;
#3271 = EDGE_LOOP ( 'NONE', ( #871, #11955, #12087, #3204 ) ) ;
#3272 = CARTESIAN_POINT ( 'NONE',  ( -14.43678919070000077, -74.15747494800001505, 36.75078895099999698 ) ) ;
#3273 = CARTESIAN_POINT ( 'NONE',  ( 11.95646652419999967, -101.4254868690000109, -10.58588781379999944 ) ) ;
#3274 = CARTESIAN_POINT ( 'NONE',  ( -2.483423092989999859, -26.06274386000000121, -23.44595030099999988 ) ) ;
#3275 = DIRECTION ( 'NONE',  ( 1.000000000000000000, 0.000000000000000000, 0.000000000000000000 ) ) ;
#3276 = AXIS2_PLACEMENT_3D ( 'NONE', #6822, #4781, #24889 ) ;
#3277 = DIRECTION ( 'NONE',  ( 1.000000000000000000, 0.000000000000000000, 0.000000000000000000 ) ) ;
#3278 = EDGE_CURVE ( 'NONE', #26635, #12535, #12296, .T. ) ;
#3279 = LINE ( 'NONE', #11994, #9665 ) ;
#3280 = CARTESIAN_POINT ( 'NONE',  ( 23.40924512820000203, -53.22700740269999642, -9.524618309619999224 ) ) ;
#3281 = CARTESIAN_POINT ( 'NONE',  ( -13.55269044519999966, -111.0000000000000000, -9.843123574170000722 ) ) ;
#3282 = FACE_OUTER_BOUND ( 'NONE', #8463, .T. ) ;
#3283 = EDGE_LOOP ( 'NONE', ( #4893, #18597, #24736, #8867, #10571, #12621 ) ) ;
#3284 = CARTESIAN_POINT ( 'NONE',  ( 6.961737886719999935, -101.4121386959999995, 14.38077149549999945 ) ) ;
#3285 = CARTESIAN_POINT ( 'NONE',  ( -8.359362780541310656, -94.05619596941960481, -23.03490016510948735 ) ) ;
#3286 = CARTESIAN_POINT ( 'NONE',  ( 7.579179873580000226, -101.3235621230000021, 13.98627925510000125 ) ) ;
#3287 = LINE ( 'NONE', #3422, #12145 ) ;
#3288 = CARTESIAN_POINT ( 'NONE',  ( 7.310010114310000695, -36.32767552400000710, -21.47202530089999684 ) ) ;
#3289 = LINE ( 'NONE', #9959, #1519 ) ;
#3290 = CARTESIAN_POINT ( 'NONE',  ( -32.39999999999999858, -86.00000000000000000, 0.000000000000000000 ) ) ;
#3291 = TOROIDAL_SURFACE ( 'NONE', #1004, 29.91857981989999971, 10.00000000000000000 ) ;
#3292 = LINE ( 'NONE', #837, #26301 ) ;
#3293 = EDGE_LOOP ( 'NONE', ( #2683, #25707, #25641, #5766 ) ) ;
#3294 = CARTESIAN_POINT ( 'NONE',  ( -2.555686511607881517, -71.82672801145491803, -28.11473483637883675 ) ) ;
#3295 = DIRECTION ( 'NONE',  ( -0.7071067811865470176, 0.000000000000000000, -0.7071067811865480168 ) ) ;
#3296 = ORIENTED_EDGE ( 'NONE', *, *, #23338, .F. ) ;
#3297 = CARTESIAN_POINT ( 'NONE',  ( -32.83566817450000030, -79.50000000000000000, -22.22906645670000003 ) ) ;
#3298 = EDGE_LOOP ( 'NONE', ( #21641, #21966, #19805, #15161, #11151 ) ) ;
#3299 = DIRECTION ( 'NONE',  ( 0.000000000000000000, 1.000000000000000000, 0.000000000000000000 ) ) ;
#3300 = FACE_OUTER_BOUND ( 'NONE', #22997, .T. ) ;
#3301 = CARTESIAN_POINT ( 'NONE',  ( 13.18316069947562141, -92.84927079009474937, 27.50371515764524943 ) ) ;
#3302 = CARTESIAN_POINT ( 'NONE',  ( -11.73626289319999927, -94.71481161159999829, -21.34523302109999676 ) ) ;
#3303 = CARTESIAN_POINT ( 'NONE',  ( 22.05228288849999885, -72.00360875399999827, -30.91980140109999553 ) ) ;
#3304 = DIRECTION ( 'NONE',  ( 0.000000000000000000, 1.000000000000000000, 0.000000000000000000 ) ) ;
#3305 = CARTESIAN_POINT ( 'NONE',  ( -5.273680924649999824, -107.1975888269999899, -9.653408180790000515 ) ) ;
#3306 = CARTESIAN_POINT ( 'NONE',  ( 8.804564246469999134, -31.59895619559999957, -20.26062780839999888 ) ) ;
#3307 = CARTESIAN_POINT ( 'NONE',  ( -26.69328098980000163, -74.00000000000000000, -37.29988270759999835 ) ) ;
#3308 = CARTESIAN_POINT ( 'NONE',  ( 4.882943008269999509E-15, -69.50000000000000000, -40.00000000000000000 ) ) ;
#3309 = CIRCLE ( 'NONE', #25615, 0.4999999999999990008 ) ;
#3310 = ORIENTED_EDGE ( 'NONE', *, *, #22963, .T. ) ;
#3312 = EDGE_CURVE ( 'NONE', #13063, #4330, #11124, .T. ) ;
#3311 = AXIS2_PLACEMENT_3D ( 'NONE', #22567, #17751, #6823 ) ;
#3313 = PLANE ( 'NONE',  #22299 ) ;
#3314 = AXIS2_PLACEMENT_3D ( 'NONE', #893, #16880, #19198 ) ;
#3315 = ORIENTED_EDGE ( 'NONE', *, *, #11420, .F. ) ;
#3316 = ADVANCED_FACE ( 'NONE', ( #1261 ), #10097, .T. ) ;
#3317 = ADVANCED_FACE ( 'NONE', ( #28179 ), #8212, .T. ) ;
#3318 = CARTESIAN_POINT ( 'NONE',  ( -41.75000000000000000, -63.30468293320000583, -1.587713240270000048 ) ) ;
#3319 = CARTESIAN_POINT ( 'NONE',  ( -28.34275910430000067, -92.98926436760000058, 1.604598016960000040 ) ) ;
#3320 = CARTESIAN_POINT ( 'NONE',  ( -31.00000000000000000, -11.00000000000000000, -2.486899575159999765E-14 ) ) ;
#3321 = EDGE_LOOP ( 'NONE', ( #21756, #13298, #26410, #6339 ) ) ;
#3322 = CARTESIAN_POINT ( 'NONE',  ( -29.52408826051700075, -93.00000237470420927, 5.228628232560329714 ) ) ;
#3323 = CARTESIAN_POINT ( 'NONE',  ( -7.561758309997661520, -74.02518802157268851, -38.96765197712468165 ) ) ;
#3324 = ORIENTED_EDGE ( 'NONE', *, *, #7736, .T. ) ;
#3325 = DIRECTION ( 'NONE',  ( -0.2414462220490755373, 0.000000000000000000, -0.9704142011833032377 ) ) ;
#3326 = CARTESIAN_POINT ( 'NONE',  ( -17.94180966909999597, -19.50000000000000000, 18.81731824139999887 ) ) ;
#3327 = TOROIDAL_SURFACE ( 'NONE', #28419, 55.85192378860000417, 0.3499999999999999778 ) ;
#3328 = AXIS2_PLACEMENT_3D ( 'NONE', #12396, #3130, #14598 ) ;
#3329 = CARTESIAN_POINT ( 'NONE',  ( -16.73195129730000374, -84.25000000000000000, -30.62763141000000289 ) ) ;
#3330 = DIRECTION ( 'NONE',  ( 0.9601004944592514967, 0.000000000000000000, -0.2796552172570731520 ) ) ;
#3331 = VERTEX_POINT ( 'NONE', #25991 ) ;
#3332 = CYLINDRICAL_SURFACE ( 'NONE', #10191, 0.1999999999999997891 ) ;
#3333 = CARTESIAN_POINT ( 'NONE',  ( -16.25371433440000146, -100.5776968050000022, 3.032057373910000297 ) ) ;
#3334 = CARTESIAN_POINT ( 'NONE',  ( 24.49010419710000264, -63.63799337820000090, -0.5178770050080000464 ) ) ;
#3335 = CARTESIAN_POINT ( 'NONE',  ( 19.44161842069999935, -34.82993252660000394, -8.988741827920000205 ) ) ;
#3336 = EDGE_LOOP ( 'NONE', ( #25336, #17133, #10156, #5233 ) ) ;
#3337 = CARTESIAN_POINT ( 'NONE',  ( 0.000000000000000000, -19.70310889130000120, 0.000000000000000000 ) ) ;
#3338 = CARTESIAN_POINT ( 'NONE',  ( -2.326474588770000018, -19.16559685929999901, -22.80254021129999842 ) ) ;
#3339 = DIRECTION ( 'NONE',  ( -0.000000000000000000, 1.000000000000000000, 0.000000000000000000 ) ) ;
#3340 = ORIENTED_EDGE ( 'NONE', *, *, #25811, .T. ) ;
#3341 = EDGE_CURVE ( 'NONE', #7636, #8453, #2770, .T. ) ;
#3342 = CARTESIAN_POINT ( 'NONE',  ( -41.61565191535785146, -65.09473604208761799, -2.877732256211138928 ) ) ;
#3343 = CARTESIAN_POINT ( 'NONE',  ( -31.89935321680000158, -74.00000000000000000, -21.99985828019999801 ) ) ;
#3344 = CARTESIAN_POINT ( 'NONE',  ( -11.35954001540000036, -79.50000000000000000, 45.25000000000000000 ) ) ;
#3345 = CARTESIAN_POINT ( 'NONE',  ( -1.776356839399999804E-15, -89.00000000000000000, 0.000000000000000000 ) ) ;
#3346 = ORIENTED_EDGE ( 'NONE', *, *, #6428, .T. ) ;
#3347 = EDGE_CURVE ( 'NONE', #5424, #7860, #11069, .T. ) ;
#3348 = AXIS2_PLACEMENT_3D ( 'NONE', #28430, #5992, #14872 ) ;
#3349 = AXIS2_PLACEMENT_3D ( 'NONE', #18069, #15420, #4956 ) ;
#3350 = EDGE_CURVE ( 'NONE', #25460, #7740, #21944, .T. ) ;
#3351 = UNCERTAINTY_MEASURE_WITH_UNIT (LENGTH_MEASURE( 1.000000000000000082E-05 ), #10188, 'distance_accuracy_value', 'NONE');
#3352 = CARTESIAN_POINT ( 'NONE',  ( 6.688784535489389782, -101.3038909011303161, 14.82808411082569222 ) ) ;
#3353 = CARTESIAN_POINT ( 'NONE',  ( -1.767871301636886550, -80.14255480913817564, 47.03116330652069621 ) ) ;
#3354 = ORIENTED_EDGE ( 'NONE', *, *, #25773, .F. ) ;
#3355 = LINE ( 'NONE', #10297, #24912 ) ;
#3356 = EDGE_LOOP ( 'NONE', ( #12342, #23781 ) ) ;
#3357 = DIRECTION ( 'NONE',  ( -0.5301416321220548955, 0.000000000000000000, -0.8479091047340887588 ) ) ;
#3358 = CARTESIAN_POINT ( 'NONE',  ( -6.181676134210000839, -101.5369810359999860, 14.75803956719999910 ) ) ;
#3359 = ORIENTED_EDGE ( 'NONE', *, *, #8938, .F. ) ;
#3360 = CARTESIAN_POINT ( 'NONE',  ( -21.35786096709999882, -65.07443093669999712, 13.27975207949999970 ) ) ;
#3361 = TOROIDAL_SURFACE ( 'NONE', #8514, 5.500000000000000000, 0.5000000000000000000 ) ;
#3362 = AXIS2_PLACEMENT_3D ( 'NONE', #18592, #21476, #14759 ) ;
#3363 = PLANE ( 'NONE',  #9255 ) ;
#3364 = CARTESIAN_POINT ( 'NONE',  ( 25.61850624154103073, -69.24211324756858232, -8.680134436598166303 ) ) ;
#3365 = DIRECTION ( 'NONE',  ( 1.000000000000000000, 0.000000000000000000, 0.000000000000000000 ) ) ;
#3366 = AXIS2_PLACEMENT_3D ( 'NONE', #11334, #20533, #26505 ) ;
#3367 = CARTESIAN_POINT ( 'NONE',  ( 9.755293273557064992, -61.61770146517354618, -24.04309117867698475 ) ) ;
#3368 = VERTEX_POINT ( 'NONE', #1809 ) ;
#3369 = CARTESIAN_POINT ( 'NONE',  ( -32.80949674840000085, -79.81706281630000888, -22.29175087539999822 ) ) ;
#3370 = CARTESIAN_POINT ( 'NONE',  ( 15.74335372269999844, -101.6484611540000031, 2.854262350110000401 ) ) ;
#3371 = CARTESIAN_POINT ( 'NONE',  ( -20.56696564920000014, -93.13213601760000415, 16.30486652549999960 ) ) ;
#3372 = CARTESIAN_POINT ( 'NONE',  ( 9.334872109610000362E-16, -74.00000000000000000, -2.419703924680000090E-15 ) ) ;
#3373 = ORIENTED_EDGE ( 'NONE', *, *, #1537, .T. ) ;
#3374 = EDGE_CURVE ( 'NONE', #16418, #26990, #27885, .T. ) ;
#3375 = CARTESIAN_POINT ( 'NONE',  ( 29.72764218755513710, -92.82709422631323548, 6.820359001708948377 ) ) ;
#3376 = LINE ( 'NONE', #789, #7991 ) ;
#3377 = ORIENTED_EDGE ( 'NONE', *, *, #20265, .T. ) ;
#3378 = EDGE_CURVE ( 'NONE', #27814, #4274, #28455, .T. ) ;
#3379 = CARTESIAN_POINT ( 'NONE',  ( 0.000000000000000000, -56.78056608349999834, 0.000000000000000000 ) ) ;
#3380 = CARTESIAN_POINT ( 'NONE',  ( 47.25000000000000000, -74.00000000000000000, 8.881784196999999612E-15 ) ) ;
#3381 = CARTESIAN_POINT ( 'NONE',  ( 21.04158602090314645, -97.05288880075438840, 0.8598937435395828111 ) ) ;
#3382 = CARTESIAN_POINT ( 'NONE',  ( 30.75969929770000277, -73.34323049660000038, -23.57645225990000171 ) ) ;
#3383 = EDGE_CURVE ( 'NONE', #5488, #8306, #10177, .T. ) ;
#3384 = CARTESIAN_POINT ( 'NONE',  ( -14.46557528003321025, -70.49261988755607433, 23.52773505033430723 ) ) ;
#3385 = EDGE_CURVE ( 'NONE', #20072, #23472, #22779, .T. ) ;
#3386 = CARTESIAN_POINT ( 'NONE',  ( -26.77683864449999973, -23.00000000000000000, -49.01467436490000296 ) ) ;
#3387 = AXIS2_PLACEMENT_3D ( 'NONE', #4443, #4737, #4885 ) ;
#3388 = ORIENTED_EDGE ( 'NONE', *, *, #13986, .T. ) ;
#3389 = CARTESIAN_POINT ( 'NONE',  ( 21.19011208810000113, -36.03998686679999963, -8.396978594420000164 ) ) ;
#3390 = CARTESIAN_POINT ( 'NONE',  ( 20.49735013020000096, -36.03245755269999506, -9.139729082780000624 ) ) ;
#3391 = DIRECTION ( 'NONE',  ( 0.4794255386042036715, 0.000000000000000000, 0.8775825618903724257 ) ) ;
#3392 = ORIENTED_EDGE ( 'NONE', *, *, #11965, .F. ) ;
#3393 = CARTESIAN_POINT ( 'NONE',  ( -13.30460049849999926, -101.3399913430000083, -9.124713982900001241 ) ) ;
#3394 = B_SPLINE_SURFACE_WITH_KNOTS ( 'NONE', 5, 5, ( 
 ( #23536, #16403, #12163, #21076, #5888, #28046 ),
 ( #16974, #12016, #14767, #23668, #11879, #20793 ),
 ( #845, #9690, #9974, #27642, #16682, #16549 ),
 ( #18605, #12303, #25445, #27771, #27493, #25311 ),
 ( #7808, #5339, #994, #21213, #9837, #18747 ),
 ( #8215, #28604, #17541, #17399, #3713, #19717 ) ),
 .UNSPECIFIED., .F., .F., .F.,
 ( 6, 6 ),
 ( 6, 6 ),
 ( 1.309430326270000000, 3.318582255669999981 ),
 ( 0.000000000000000000, 0.5000000000000000000 ),
 .UNSPECIFIED. ) ;
#3395 = FACE_OUTER_BOUND ( 'NONE', #1279, .T. ) ;
#3396 = DIRECTION ( 'NONE',  ( 0.000000000000000000, -1.000000000000000000, 0.000000000000000000 ) ) ;
#3397 = CARTESIAN_POINT ( 'NONE',  ( 8.465915579399998947, -40.73328259390000028, -21.79505839740000184 ) ) ;
#3398 = CARTESIAN_POINT ( 'NONE',  ( 7.571226706500000070, -101.3243788949999953, 13.99005347329999793 ) ) ;
#3399 = EDGE_LOOP ( 'NONE', ( #11630, #2471, #11380, #9755 ) ) ;
#3400 = CARTESIAN_POINT ( 'NONE',  ( -43.21399166432318850, -65.14196057591203726, -0.1651269895930678189 ) ) ;
#3401 = DIRECTION ( 'NONE',  ( 0.9952295494196657932, 0.000000000000000000, -0.09756097560976527416 ) ) ;
#3402 = CARTESIAN_POINT ( 'NONE',  ( 12.01538071500000093, -98.51736893780000059, -15.58690078470000095 ) ) ;
#3403 = ORIENTED_EDGE ( 'NONE', *, *, #11049, .T. ) ;
#3404 = AXIS2_PLACEMENT_3D ( 'NONE', #16967, #27485, #21337 ) ;
#3405 = CARTESIAN_POINT ( 'NONE',  ( 20.10370293170000267, -18.85979313690000225, -8.426925535960000602 ) ) ;
#3406 = VECTOR ( 'NONE', #4224, 1000.000000000000000 ) ;
#3407 = DIRECTION ( 'NONE',  ( -0.04503285875970657742, 0.000000000000000000, -0.9989855062171465461 ) ) ;
#3408 = AXIS2_PLACEMENT_3D ( 'NONE', #216, #512, #6753 ) ;
#3409 = CARTESIAN_POINT ( 'NONE',  ( -14.66608903329999869, -74.50000000000000000, 36.47374631129999756 ) ) ;
#3410 = DIRECTION ( 'NONE',  ( 0.000000000000000000, -1.000000000000000000, 0.000000000000000000 ) ) ;
#3411 = CARTESIAN_POINT ( 'NONE',  ( -17.99251962983047548, -92.56492639278971524, 24.62779902097171103 ) ) ;
#3412 = EDGE_CURVE ( 'NONE', #2130, #13695, #27423, .T. ) ;
#3413 = CARTESIAN_POINT ( 'NONE',  ( 0.000000000000000000, -16.50000000000000000, 0.000000000000000000 ) ) ;
#3414 = EDGE_CURVE ( 'NONE', #19902, #726, #16380, .T. ) ;
#3415 = DIRECTION ( 'NONE',  ( 0.000000000000000000, 1.000000000000000000, 0.000000000000000000 ) ) ;
#3416 = CARTESIAN_POINT ( 'NONE',  ( -32.83566817730000054, -74.50000000000000000, -22.22906645950000026 ) ) ;
#3417 = FACE_OUTER_BOUND ( 'NONE', #17356, .T. ) ;
#3418 = ORIENTED_EDGE ( 'NONE', *, *, #26655, .T. ) ;
#3419 = CARTESIAN_POINT ( 'NONE',  ( -32.77174709959999888, -74.43710720380001078, -21.60034937849999892 ) ) ;
#3420 = CARTESIAN_POINT ( 'NONE',  ( -21.60034937969999902, -74.50000000000000000, -32.77174707999999725 ) ) ;
#3421 = AXIS2_PLACEMENT_3D ( 'NONE', #20098, #24470, #12932 ) ;
#3422 = CARTESIAN_POINT ( 'NONE',  ( 7.564829567879999012E-15, -73.00000000000000000, 32.75000000000000000 ) ) ;
#3423 = CARTESIAN_POINT ( 'NONE',  ( 19.90557433739999738, -34.65022632540000558, -8.965966767359999423 ) ) ;
#3424 = CARTESIAN_POINT ( 'NONE',  ( 7.250038883935697065, -73.95086734785802207, 39.95935625373193290 ) ) ;
#3425 = CARTESIAN_POINT ( 'NONE',  ( -13.96596450430000047, -64.58097845250000546, 21.73803617189999926 ) ) ;
#3426 = VECTOR ( 'NONE', #24344, 1000.000000000000000 ) ;
#3427 = CARTESIAN_POINT ( 'NONE',  ( -38.79568063749716345, -74.00014642295835188, 7.600472224630967055 ) ) ;
#3428 = EDGE_CURVE ( 'NONE', #5725, #6342, #7682, .T. ) ;
#3429 = CARTESIAN_POINT ( 'NONE',  ( 26.69293917519999937, -19.09689110869999951, 48.86109741659999628 ) ) ;
#3430 = VERTEX_POINT ( 'NONE', #7197 ) ;
#3431 = CARTESIAN_POINT ( 'NONE',  ( 31.68381302702793434, -74.06963932891925140, -22.77788534991574210 ) ) ;
#3432 = DIRECTION ( 'NONE',  ( 0.000000000000000000, 1.000000000000000000, 0.000000000000000000 ) ) ;
#3433 = ORIENTED_EDGE ( 'NONE', *, *, #20242, .F. ) ;
#3434 = CARTESIAN_POINT ( 'NONE',  ( -30.40640577132692357, -92.81370807101379228, 2.387642233200668151 ) ) ;
#3435 = ORIENTED_EDGE ( 'NONE', *, *, #26209, .T. ) ;
#3436 = CARTESIAN_POINT ( 'NONE',  ( 0.3872056760440000245, -99.92967571559999840, -17.35614698070000017 ) ) ;
#3437 = PLANE ( 'NONE',  #1876 ) ;
#3438 = AXIS2_PLACEMENT_3D ( 'NONE', #5161, #668, #24973 ) ;
#3439 = CARTESIAN_POINT ( 'NONE',  ( 13.68012917844785292, -92.58608763744132375, 27.25993674634458230 ) ) ;
#3440 = CARTESIAN_POINT ( 'NONE',  ( 20.33277134760000138, -73.81489374239998824, -32.04417015119999945 ) ) ;
#3441 = ADVANCED_FACE ( 'NONE', ( #15767 ), #24673, .T. ) ;
#3442 = CARTESIAN_POINT ( 'NONE',  ( -40.50000000000000000, -15.00000000000000000, 4.500000000000000000 ) ) ;
#3443 = DIRECTION ( 'NONE',  ( 0.000000000000000000, 1.000000000000000000, 0.000000000000000000 ) ) ;
#3444 = DIRECTION ( 'NONE',  ( 0.000000000000000000, -1.000000000000000000, 0.000000000000000000 ) ) ;
#3445 = DIRECTION ( 'NONE',  ( 1.000000000000000000, 0.000000000000000000, 0.000000000000000000 ) ) ;
#3446 = CIRCLE ( 'NONE', #15027, 6.000000000000000000 ) ;
#3447 = CARTESIAN_POINT ( 'NONE',  ( -31.64302845809999809, -74.00000000000000000, -31.64302845809999809 ) ) ;
#3448 = VERTEX_POINT ( 'NONE', #2826 ) ;
#3449 = ORIENTED_EDGE ( 'NONE', *, *, #18469, .T. ) ;
#3450 = AXIS2_PLACEMENT_3D ( 'NONE', #3517, #23197, #3243 ) ;
#3451 = CARTESIAN_POINT ( 'NONE',  ( -14.01337423622812928, -80.36910030610464162, 36.66316738247557083 ) ) ;
#3452 = VECTOR ( 'NONE', #13602, 1000.000000000000000 ) ;
#3453 = CARTESIAN_POINT ( 'NONE',  ( 9.828880478180000324, -36.53914149509999731, -22.51363315740000104 ) ) ;
#3454 = DIRECTION ( 'NONE',  ( 0.000000000000000000, 1.000000000000000000, 0.000000000000000000 ) ) ;
#3455 = FACE_OUTER_BOUND ( 'NONE', #3067, .T. ) ;
#3456 = EDGE_CURVE ( 'NONE', #27709, #2458, #10609, .T. ) ;
#3457 = CARTESIAN_POINT ( 'NONE',  ( 19.83285472758843682, -19.48229551556754657, -8.720275436146035730 ) ) ;
#3458 = ORIENTED_EDGE ( 'NONE', *, *, #12233, .F. ) ;
#3459 = CARTESIAN_POINT ( 'NONE',  ( -27.64435950660053010, -93.39299082529144869, 0.4115795295578285606 ) ) ;
#3460 = ORIENTED_EDGE ( 'NONE', *, *, #26996, .F. ) ;
#3461 = CIRCLE ( 'NONE', #28561, 7.250000000000000000 ) ;
#3462 = CARTESIAN_POINT ( 'NONE',  ( 23.03829042120000281, -52.56313962710000709, 10.32398954119999956 ) ) ;
#3463 = CARTESIAN_POINT ( 'NONE',  ( 9.032270281389999766, -35.86447823839999671, -20.16936839779999957 ) ) ;
#3464 = FACE_OUTER_BOUND ( 'NONE', #19566, .T. ) ;
#3465 = CARTESIAN_POINT ( 'NONE',  ( 26.45655024610000083, -92.68419354089999729, -7.824660114159999402 ) ) ;
#3466 = EDGE_CURVE ( 'NONE', #3592, #87, #8756, .T. ) ;
#3467 = CARTESIAN_POINT ( 'NONE',  ( -17.65314336990000399, -18.50000000000000000, 13.58065803889999934 ) ) ;
#3468 = ORIENTED_EDGE ( 'NONE', *, *, #5913, .F. ) ;
#3469 = CARTESIAN_POINT ( 'NONE',  ( -14.91147105619999991, -101.0534797690000062, 4.558379831599999044 ) ) ;
#3470 = CARTESIAN_POINT ( 'NONE',  ( -16.52509094760000252, -100.0517779130000093, 2.709010215110000175 ) ) ;
#3471 = CARTESIAN_POINT ( 'NONE',  ( -32.77954208402166358, -74.32766453548276786, -22.21551416184748717 ) ) ;
#3472 = B_SPLINE_CURVE_WITH_KNOTS ( 'NONE', 5,
 ( #4311, #110, #6346, #28772, #10837, #19746, #4602, #15210, #24125, #8959, #4160, #13033, #13186, #17867, #22095, #10974, #18606, #20935 ),
 .UNSPECIFIED., .F., .F.,
 ( 6, 3, 3, 3, 3, 6 ),
 ( 0.000000000000000000, 1.123597682139999998, 2.251105814059999766, 3.378920982569999953, 4.507089344490000649, 5.576980695549999645 ),
 .UNSPECIFIED. ) ;
#3473 = CARTESIAN_POINT ( 'NONE',  ( -19.85441137420000146, -60.55428303689999581, 13.13179032179999872 ) ) ;
#3474 = ORIENTED_EDGE ( 'NONE', *, *, #20906, .F. ) ;
#3475 = CIRCLE ( 'NONE', #23926, 0.7500000000000000000 ) ;
#3476 = CARTESIAN_POINT ( 'NONE',  ( 46.25000000000000000, -79.00000000000000000, -7.375000000000000000 ) ) ;
#3477 = CARTESIAN_POINT ( 'NONE',  ( -3.299060175100000158, -18.50000000000000000, -24.39335979490000028 ) ) ;
#3478 = CARTESIAN_POINT ( 'NONE',  ( 36.49396608176380852, -74.06970218573687248, -14.11767483867770601 ) ) ;
#3480 = EDGE_LOOP ( 'NONE', ( #26192, #10796, #25597, #19751 ) ) ;
#3479 = B_SPLINE_CURVE_WITH_KNOTS ( 'NONE', 5,
 ( #15078, #3884, #3746, #23987, #12749, #4021 ),
 .UNSPECIFIED., .F., .F.,
 ( 6, 6 ),
 ( 0.000000000000000000, 1.000000000000000000 ),
 .UNSPECIFIED. ) ;
#3481 = DIRECTION ( 'NONE',  ( 1.000000000000000000, 0.000000000000000000, 0.000000000000000000 ) ) ;
#3482 = DIRECTION ( 'NONE',  ( 0.000000000000000000, -1.000000000000000000, 0.000000000000000000 ) ) ;
#3483 = DIRECTION ( 'NONE',  ( 1.000000000000000000, 0.000000000000000000, 0.000000000000000000 ) ) ;
#3484 = ORIENTED_EDGE ( 'NONE', *, *, #9550, .T. ) ;
#3485 = CIRCLE ( 'NONE', #21167, 30.50000000000000000 ) ;
#3486 = AXIS2_PLACEMENT_3D ( 'NONE', #282, #4476, #4624 ) ;
#3487 = CARTESIAN_POINT ( 'NONE',  ( 36.77570183985819341, -79.45385781081505172, -14.64121397519159196 ) ) ;
#3488 = CARTESIAN_POINT ( 'NONE',  ( 7.181689689069999716, -99.92967571559999840, 15.80535034289999885 ) ) ;
#3489 = CARTESIAN_POINT ( 'NONE',  ( -2.450393045606315656, -80.33972342794427846, 46.82405269585417074 ) ) ;
#3490 = ORIENTED_EDGE ( 'NONE', *, *, #12125, .F. ) ;
#3491 = CARTESIAN_POINT ( 'NONE',  ( -14.60877014137605379, -74.50000000000000000, 36.82513846446037320 ) ) ;
#3492 = CARTESIAN_POINT ( 'NONE',  ( 47.25000000000000000, -75.00000000000000000, -1.242228542250000064E-12 ) ) ;
#3493 = VERTEX_POINT ( 'NONE', #11688 ) ;
#3494 = CONICAL_SURFACE ( 'NONE', #8137, 55.67692378859999280, 1.047197551199999799 ) ;
#3495 = CARTESIAN_POINT ( 'NONE',  ( 28.15407045200000269, -92.49999926799999628, 8.194203099389998357 ) ) ;
#3496 = CARTESIAN_POINT ( 'NONE',  ( -5.935178058420000013, -101.2490009469999990, 14.94671830490000097 ) ) ;
#3497 = ORIENTED_EDGE ( 'NONE', *, *, #10431, .F. ) ;
#3498 = CARTESIAN_POINT ( 'NONE',  ( 0.000000000000000000, -83.75000000000000000, 0.000000000000000000 ) ) ;
#3499 = CARTESIAN_POINT ( 'NONE',  ( 22.51853742079654808, -36.00000000000000000, -11.01541626719902922 ) ) ;
#3500 = EDGE_CURVE ( 'NONE', #11909, #7960, #8656, .T. ) ;
#3501 = ORIENTED_EDGE ( 'NONE', *, *, #23788, .T. ) ;
#3502 = CARTESIAN_POINT ( 'NONE',  ( 39.59129699470000219, -73.90055525949999549, 7.279149876810000031 ) ) ;
#3503 = CARTESIAN_POINT ( 'NONE',  ( -13.46646228700000059, -101.3150700380000018, -9.098096927170001180 ) ) ;
#3504 = EDGE_CURVE ( 'NONE', #13461, #15756, #28771, .T. ) ;
#3505 = LINE ( 'NONE', #3231, #27438 ) ;
#3506 = CARTESIAN_POINT ( 'NONE',  ( 0.000000000000000000, -19.40000000000000213, 0.000000000000000000 ) ) ;
#3507 = ORIENTED_EDGE ( 'NONE', *, *, #8637, .F. ) ;
#3508 = EDGE_CURVE ( 'NONE', #16242, #19815, #14388, .T. ) ;
#3509 = CARTESIAN_POINT ( 'NONE',  ( -13.18672279729999985, -99.64579499010000063, -11.23091032149999968 ) ) ;
#3510 = CARTESIAN_POINT ( 'NONE',  ( 15.91799941834440268, -101.5019029711150012, 2.484100747937272757 ) ) ;
#3511 = CARTESIAN_POINT ( 'NONE',  ( -20.67841902900000051, -93.05545087649998948, 16.29593949070000036 ) ) ;
#3512 = CARTESIAN_POINT ( 'NONE',  ( 40.00000000000000000, -77.00000000000000000, 0.000000000000000000 ) ) ;
#3513 = ORIENTED_EDGE ( 'NONE', *, *, #26160, .T. ) ;
#3514 = CARTESIAN_POINT ( 'NONE',  ( -2.238370485110000363, -80.04479719919999070, 47.01479521750000146 ) ) ;
#3515 = CARTESIAN_POINT ( 'NONE',  ( 24.22382764319999993, -64.24504439390000243, 10.76339940740000145 ) ) ;
#3516 = ORIENTED_EDGE ( 'NONE', *, *, #24133, .T. ) ;
#3517 = CARTESIAN_POINT ( 'NONE',  ( 0.000000000000000000, -108.5000000000000000, 0.000000000000000000 ) ) ;
#3518 = CARTESIAN_POINT ( 'NONE',  ( 4.037078284719999375E-15, -74.00000000000000000, -40.00000000000000000 ) ) ;
#3519 = CARTESIAN_POINT ( 'NONE',  ( -14.40572000550000098, -18.50000000000000000, 20.06574520719999910 ) ) ;
#3520 = CARTESIAN_POINT ( 'NONE',  ( 27.75394116159999669, -74.50000000000000000, -27.75394116159999669 ) ) ;
#3521 = CARTESIAN_POINT ( 'NONE',  ( -21.30003612899999865, -111.0000000000000000, -21.83021898440000186 ) ) ;
#3522 = DIRECTION ( 'NONE',  ( 1.000000000000000000, 0.000000000000000000, 0.000000000000000000 ) ) ;
#3523 = ORIENTED_EDGE ( 'NONE', *, *, #24757, .F. ) ;
#3524 = CARTESIAN_POINT ( 'NONE',  ( 9.332951828819998852, -36.18018306619999436, -21.06416784469999826 ) ) ;
#3525 = CARTESIAN_POINT ( 'NONE',  ( 20.66368818489999981, -35.66750349659999841, -8.753531078070000859 ) ) ;
#3526 = AXIS2_PLACEMENT_3D ( 'NONE', #13675, #28533, #8568 ) ;
#3527 = CARTESIAN_POINT ( 'NONE',  ( 20.03541958720000338, -35.94892542979999916, -9.230207021330000927 ) ) ;
#3528 = DIRECTION ( 'NONE',  ( 0.5000000000001900702, 0.000000000000000000, -0.8660254037843290176 ) ) ;
#3529 = ORIENTED_EDGE ( 'NONE', *, *, #6069, .T. ) ;
#3530 = CARTESIAN_POINT ( 'NONE',  ( -12.29363612039999865, -101.2530993000000024, -8.928690578759999497 ) ) ;
#3531 = EDGE_CURVE ( 'NONE', #20422, #7443, #4179, .T. ) ;
#3532 = FACE_OUTER_BOUND ( 'NONE', #8224, .T. ) ;
#3533 = ORIENTED_EDGE ( 'NONE', *, *, #25266, .T. ) ;
#3534 = CARTESIAN_POINT ( 'NONE',  ( -1.228306939259999897, -101.1461863720000025, -16.11255642589999937 ) ) ;
#3535 = CARTESIAN_POINT ( 'NONE',  ( 13.01745538959999848, -111.0000000000000000, -10.62006851110000127 ) ) ;
#3536 = VECTOR ( 'NONE', #24102, 999.9999999999998863 ) ;
#3537 = CARTESIAN_POINT ( 'NONE',  ( 7.202169754829999881, -101.2530994060000040, 13.37848089620000103 ) ) ;
#3538 = ORIENTED_EDGE ( 'NONE', *, *, #5536, .F. ) ;
#3539 = ADVANCED_FACE ( 'NONE', ( #24789 ), #480, .F. ) ;
#3540 = CARTESIAN_POINT ( 'NONE',  ( 12.85307023921196468, -101.4085864806519481, -9.837083722716631229 ) ) ;
#3541 = DIRECTION ( 'NONE',  ( -2.220446049250000002E-16, 0.000000000000000000, 1.000000000000000000 ) ) ;
#3542 = CARTESIAN_POINT ( 'NONE',  ( 11.15108638419999920, -100.9197081840000010, -10.94438793620000183 ) ) ;
#3543 = VERTEX_POINT ( 'NONE', #4520 ) ;
#3544 = CARTESIAN_POINT ( 'NONE',  ( -14.60455326470000159, -74.31496036839999419, 36.89972645289999775 ) ) ;
#3545 = CARTESIAN_POINT ( 'NONE',  ( 12.04737265750000041, -101.5369810359999860, -10.52904611309999972 ) ) ;
#3546 = CARTESIAN_POINT ( 'NONE',  ( -14.51929513910000047, -74.27627443250000283, 36.71621193889999546 ) ) ;
#3547 = CARTESIAN_POINT ( 'NONE',  ( -17.98395509190000041, -94.09782194550001577, 17.16060177909999851 ) ) ;
#3548 = CARTESIAN_POINT ( 'NONE',  ( -18.59081129359999807, -92.50000000000000000, 24.17915911369999904 ) ) ;
#3549 = ORIENTED_EDGE ( 'NONE', *, *, #13069, .T. ) ;
#3550 = DIRECTION ( 'NONE',  ( 0.000000000000000000, 1.000000000000000000, 0.000000000000000000 ) ) ;
#3551 = DIRECTION ( 'NONE',  ( -0.09756097560976655092, 0.000000000000000000, -0.9952295494196655712 ) ) ;
#3552 = CARTESIAN_POINT ( 'NONE',  ( 23.52622212079999997, -57.40875702419999982, -9.564509902250000195 ) ) ;
#3553 = DIRECTION ( 'NONE',  ( 0.000000000000000000, 1.000000000000000000, 0.000000000000000000 ) ) ;
#3554 = CARTESIAN_POINT ( 'NONE',  ( 22.62017292919999889, -58.65571127909999660, 10.18887697589999952 ) ) ;
#3555 = ORIENTED_EDGE ( 'NONE', *, *, #17303, .F. ) ;
#3556 = CARTESIAN_POINT ( 'NONE',  ( 6.812757346439999750, -99.85455315880000171, 15.72436791289999825 ) ) ;
#3557 = CARTESIAN_POINT ( 'NONE',  ( 15.61171978429999996, -101.6311724339999927, 3.565474465639999924 ) ) ;
#3558 = CARTESIAN_POINT ( 'NONE',  ( 7.723274522320000557, -101.5232170330000088, 14.02298824230000029 ) ) ;
#3559 = CARTESIAN_POINT ( 'NONE',  ( -11.60187077849999859, -94.77767847329999995, -21.32567029700000205 ) ) ;
#3560 = CARTESIAN_POINT ( 'NONE',  ( 7.299999026299999194, -35.81311514570000298, -21.43074813960000213 ) ) ;
#3561 = CARTESIAN_POINT ( 'NONE',  ( 23.73650098047212254, -62.45651223016474773, 10.62604559626449685 ) ) ;
#3562 = CARTESIAN_POINT ( 'NONE',  ( -7.941640844080000150, -99.73367660430000115, 15.38008034509999966 ) ) ;
#3563 = CARTESIAN_POINT ( 'NONE',  ( 8.577089147620000631, -94.15497152599999708, -23.87126057090000231 ) ) ;
#3564 = EDGE_CURVE ( 'NONE', #5746, #20422, #22628, .T. ) ;
#3565 = CARTESIAN_POINT ( 'NONE',  ( 0.000000000000000000, -101.6484611540000031, 0.000000000000000000 ) ) ;
#3566 = ORIENTED_EDGE ( 'NONE', *, *, #22511, .F. ) ;
#3567 = CARTESIAN_POINT ( 'NONE',  ( 7.508026895748405316, -35.02998825093359869, -21.30133317590891906 ) ) ;
#3568 = CARTESIAN_POINT ( 'NONE',  ( -5.487411647150000071, -100.8733988930000010, 14.73625039430000072 ) ) ;
#3569 = ORIENTED_EDGE ( 'NONE', *, *, #18939, .F. ) ;
#3570 = CYLINDRICAL_SURFACE ( 'NONE', #28479, 61.34999999999998721 ) ;
#3571 = ORIENTED_EDGE ( 'NONE', *, *, #1592, .T. ) ;
#3572 = EDGE_CURVE ( 'NONE', #24310, #11938, #14618, .T. ) ;
#3573 = CARTESIAN_POINT ( 'NONE',  ( 0.1687264450993073983, -101.5409490181601058, -16.08202886997192493 ) ) ;
#3574 = DIRECTION ( 'NONE',  ( 0.000000000000000000, 1.000000000000000000, 0.000000000000000000 ) ) ;
#3575 = CARTESIAN_POINT ( 'NONE',  ( 14.01961443358530701, -92.52249206702738604, 27.08691047983507261 ) ) ;
#3576 = CARTESIAN_POINT ( 'NONE',  ( 25.19069697129999952, -73.33154443940000533, -29.87473424289999713 ) ) ;
#3577 = CARTESIAN_POINT ( 'NONE',  ( -22.44049059359999987, -70.63300521989999936, 17.23241241100000209 ) ) ;
#3578 = DIRECTION ( 'NONE',  ( 0.3799696139668871098, 0.000000000000000000, -0.9249989688977251490 ) ) ;
#3579 = CARTESIAN_POINT ( 'NONE',  ( -19.04077152199090150, -19.48549492421237517, 13.94607375679098205 ) ) ;
#3580 = CARTESIAN_POINT ( 'NONE',  ( 7.135467526410000261, -73.50000000000000000, 38.71641004229999794 ) ) ;
#3581 = EDGE_LOOP ( 'NONE', ( #16468, #10485, #26309, #23412, #24380 ) ) ;
#3582 = EDGE_CURVE ( 'NONE', #2628, #14989, #25053, .T. ) ;
#3583 = ORIENTED_EDGE ( 'NONE', *, *, #11371, .F. ) ;
#3584 = FACE_OUTER_BOUND ( 'NONE', #21830, .T. ) ;
#3585 = CARTESIAN_POINT ( 'NONE',  ( -1.158751914399999805, -60.33243244399999128, -23.66032903080000338 ) ) ;
#3586 = CARTESIAN_POINT ( 'NONE',  ( -29.71161915649999941, -93.00000902169999506, 6.352307318500000299 ) ) ;
#3587 = CARTESIAN_POINT ( 'NONE',  ( 47.25000000000000000, -79.00000000000000000, -7.709388683000000122E-13 ) ) ;
#3588 = EDGE_CURVE ( 'NONE', #17507, #22416, #2451, .T. ) ;
#3589 = EDGE_CURVE ( 'NONE', #15352, #22592, #5238, .T. ) ;
#3590 = EDGE_LOOP ( 'NONE', ( #7556, #20449, #10072, #24931 ) ) ;
#3591 = CARTESIAN_POINT ( 'NONE',  ( -41.75000000000000000, -63.00000000000000000, 1.587713240270000048 ) ) ;
#3592 = VERTEX_POINT ( 'NONE', #9474 ) ;
#3593 = DIRECTION ( 'NONE',  ( 1.000000000000000000, 0.000000000000000000, 0.000000000000000000 ) ) ;
#3594 = CARTESIAN_POINT ( 'NONE',  ( 7.619628858569999608, -36.43422328860000192, -21.46039065680000135 ) ) ;
#3595 = EDGE_LOOP ( 'NONE', ( #8104, #18530, #6935, #8680 ) ) ;
#3596 = CARTESIAN_POINT ( 'NONE',  ( 22.12830645909999916, -53.29680639610000270, -7.019998623859999398 ) ) ;
#3597 = CARTESIAN_POINT ( 'NONE',  ( -16.95867319479999935, -74.00000000000000000, 44.10460184009999551 ) ) ;
#3598 = ORIENTED_EDGE ( 'NONE', *, *, #16847, .T. ) ;
#3599 = AXIS2_PLACEMENT_3D ( 'NONE', #17758, #26643, #22423 ) ;
#3600 = DIRECTION ( 'NONE',  ( 0.000000000000000000, -1.000000000000000000, 0.000000000000000000 ) ) ;
#3601 = CIRCLE ( 'NONE', #27799, 0.5000000000000004441 ) ;
#3602 = CARTESIAN_POINT ( 'NONE',  ( -15.55828293370000104, -101.5369810359999860, 3.733608462370000325 ) ) ;
#3603 = DIRECTION ( 'NONE',  ( 0.4794255386042040601, 0.000000000000000000, 0.8775825618903720926 ) ) ;
#3604 = CARTESIAN_POINT ( 'NONE',  ( -20.08490270809999956, -60.38591348639999268, 14.30072212849999858 ) ) ;
#3605 = EDGE_LOOP ( 'NONE', ( #9713, #18793, #7551, #14176 ) ) ;
#3606 = DIRECTION ( 'NONE',  ( 1.000000000000000000, 0.000000000000000000, 0.000000000000000000 ) ) ;
#3607 = DIRECTION ( 'NONE',  ( 1.000000000000000000, 0.000000000000000000, 0.000000000000000000 ) ) ;
#3608 = AXIS2_PLACEMENT_3D ( 'NONE', #21845, #28673, #19649 ) ;
#3609 = CARTESIAN_POINT ( 'NONE',  ( -3.610293792020000225, -18.50000000000000000, -24.43613468120000221 ) ) ;
#3610 = CARTESIAN_POINT ( 'NONE',  ( -12.61948338259999858, -111.0000000000000000, -9.836088610590000059 ) ) ;
#3611 = VERTEX_POINT ( 'NONE', #23318 ) ;
#3612 = EDGE_CURVE ( 'NONE', #13005, #1944, #18520, .T. ) ;
#3613 = ADVANCED_FACE ( 'NONE', ( #14148 ), #3363, .F. ) ;
#3614 = DIRECTION ( 'NONE',  ( 0.000000000000000000, 1.000000000000000000, 0.000000000000000000 ) ) ;
#3615 = AXIS2_PLACEMENT_3D ( 'NONE', #8320, #28433, #6140 ) ;
#3616 = CARTESIAN_POINT ( 'NONE',  ( -31.89935321680000158, -74.00000000000000000, -21.99985828019999801 ) ) ;
#3617 = CARTESIAN_POINT ( 'NONE',  ( 36.47640386220000153, -80.06330722010001466, -14.49564800679999976 ) ) ;
#3618 = ORIENTED_EDGE ( 'NONE', *, *, #1656, .F. ) ;
#3619 = PRODUCT_DEFINITION_CONTEXT ( 'detailed design', #11839, 'design' ) ;
#3620 = PRODUCT ( 'MAS-679', 'MAS-679', '', ( #26368 ) ) ;
#3621 = CARTESIAN_POINT ( 'NONE',  ( 36.70830968600000688, -79.13352040803519571, -14.75000000000000000 ) ) ;
#3622 = CARTESIAN_POINT ( 'NONE',  ( 6.822492494782297356, -100.4103893717170450, 15.54132353519026566 ) ) ;
#3623 = DIRECTION ( 'NONE',  ( 1.000000000000000000, 0.000000000000000000, 0.000000000000000000 ) ) ;
#3624 = ORIENTED_EDGE ( 'NONE', *, *, #700, .T. ) ;
#3625 = AXIS2_PLACEMENT_3D ( 'NONE', #20030, #22084, #2129 ) ;
#3626 = CARTESIAN_POINT ( 'NONE',  ( 47.25000000000000000, -75.00000000000000000, -1.242228542250000064E-12 ) ) ;
#3627 = EDGE_LOOP ( 'NONE', ( #1914, #15490, #4031, #22362 ) ) ;
#3628 = CARTESIAN_POINT ( 'NONE',  ( 27.23434004499999972, -92.57423549739999658, 9.563854126349999873 ) ) ;
#3629 = CARTESIAN_POINT ( 'NONE',  ( 21.92880676370000259, -37.95796630400000282, -8.677144394200000832 ) ) ;
#3630 = CARTESIAN_POINT ( 'NONE',  ( -5.549654215229999465, -100.9728541479999961, 14.57947289470000030 ) ) ;
#3631 = ORIENTED_EDGE ( 'NONE', *, *, #3508, .T. ) ;
#3632 = DIRECTION ( 'NONE',  ( 0.000000000000000000, 1.000000000000000000, 0.000000000000000000 ) ) ;
#3633 = CARTESIAN_POINT ( 'NONE',  ( -27.21207320324499079, -93.20709273738651746, -3.793618906176141170 ) ) ;
#3634 = AXIS2_PLACEMENT_3D ( 'NONE', #754, #18498, #312 ) ;
#3635 = CARTESIAN_POINT ( 'NONE',  ( 9.307965732619999599, -36.00000000019999646, -20.68428864319999860 ) ) ;
#3636 = CARTESIAN_POINT ( 'NONE',  ( 16.77426419571010996, -99.76647888980478740, 4.307225748008878696 ) ) ;
#3637 = CARTESIAN_POINT ( 'NONE',  ( -3.463923112789999870, -18.50000000000000000, -22.98618337390000121 ) ) ;
#3638 = ORIENTED_EDGE ( 'NONE', *, *, #10717, .T. ) ;
#3639 = CARTESIAN_POINT ( 'NONE',  ( -22.27192559399999894, -94.59276292389999696, -8.381615205879999309 ) ) ;
#3640 = CARTESIAN_POINT ( 'NONE',  ( 16.75373607410000076, -99.64579499020000242, 4.397195963869999780 ) ) ;
#3641 = CARTESIAN_POINT ( 'NONE',  ( -20.16249632440000283, -93.14733754460000625, 18.54048584069999706 ) ) ;
#3642 = CARTESIAN_POINT ( 'NONE',  ( 24.33711400909999867, -92.62399497440000573, -16.98201569060000082 ) ) ;
#3643 = DIRECTION ( 'NONE',  ( 0.000000000000000000, 1.000000000000000000, 0.000000000000000000 ) ) ;
#3644 = CARTESIAN_POINT ( 'NONE',  ( -3.592524694620000236, -80.18584070859999713, 46.36824188119999945 ) ) ;
#3645 = CARTESIAN_POINT ( 'NONE',  ( -12.17277550232225991, -67.87585717449533718, -23.96830675610268102 ) ) ;
#3646 = ORIENTED_EDGE ( 'NONE', *, *, #6640, .F. ) ;
#3647 = AXIS2_PLACEMENT_3D ( 'NONE', #16446, #2763, #2914 ) ;
#3648 = DIRECTION ( 'NONE',  ( 0.000000000000000000, -1.000000000000000000, 0.000000000000000000 ) ) ;
#3649 = CARTESIAN_POINT ( 'NONE',  ( 0.000000000000000000, -102.8486084350000027, 0.000000000000000000 ) ) ;
#3650 = CARTESIAN_POINT ( 'NONE',  ( 30.97095772320000151, -72.00000182920000213, -20.30102774879999927 ) ) ;
#3651 = CARTESIAN_POINT ( 'NONE',  ( -27.68682485439999752, -24.80000000000000071, -50.68039294919999804 ) ) ;
#3652 = ADVANCED_FACE ( 'NONE', ( #23182 ), #1824, .T. ) ;
#3653 = PRODUCT_DEFINITION_FORMATION_WITH_SPECIFIED_SOURCE ( 'ANY', '', #1309, .NOT_KNOWN. ) ;
#3654 = ADVANCED_FACE ( 'NONE', ( #5404 ), #27568, .F. ) ;
#3655 = ADVANCED_FACE ( 'NONE', ( #775 ), #1257, .T. ) ;
#3656 = ORIENTED_EDGE ( 'NONE', *, *, #20069, .F. ) ;
#3657 = B_SPLINE_CURVE_WITH_KNOTS ( 'NONE', 5,
 ( #25517, #7622, #23475, #14162, #12371, #23062 ),
 .UNSPECIFIED., .F., .F.,
 ( 6, 6 ),
 ( 0.000000000000000000, 1.000000000000000000 ),
 .UNSPECIFIED. ) ;
#3658 = FACE_OUTER_BOUND ( 'NONE', #2496, .T. ) ;
#3659 = CARTESIAN_POINT ( 'NONE',  ( 20.44148170879999782, -35.89950312469999716, -8.903712398839999764 ) ) ;
#3660 = LINE ( 'NONE', #10332, #26999 ) ;
#3661 = ORIENTED_EDGE ( 'NONE', *, *, #20576, .F. ) ;
#3662 = CARTESIAN_POINT ( 'NONE',  ( -12.97902083080000146, -100.9728541479999961, -8.654750722490000214 ) ) ;
#3663 = AXIS2_PLACEMENT_3D ( 'NONE', #7845, #19060, #5654 ) ;
#3664 = CARTESIAN_POINT ( 'NONE',  ( -15.07981158940000022, -92.68449574909999455, -23.80217061829999992 ) ) ;
#3665 = CARTESIAN_POINT ( 'NONE',  ( -7.959924907470000477, -99.99711545080000974, 15.21642579620000113 ) ) ;
#3666 = AXIS2_PLACEMENT_3D ( 'NONE', #957, #1227, #16789 ) ;
#3667 = CARTESIAN_POINT ( 'NONE',  ( -1.561394334049999832, -94.07620464540001137, 24.87225459399999750 ) ) ;
#3668 = CARTESIAN_POINT ( 'NONE',  ( -1.776356839399999804E-15, -80.00000000000000000, 3.552713678799999214E-14 ) ) ;
#3669 = CARTESIAN_POINT ( 'NONE',  ( -40.37009550159991988, -65.68577269143263209, 2.246086790230779062 ) ) ;
#3670 = ORIENTED_EDGE ( 'NONE', *, *, #26322, .F. ) ;
#3671 = CARTESIAN_POINT ( 'NONE',  ( 12.96791850173126193, -101.3038909013318118, -9.820641867354686028 ) ) ;
#3672 = CARTESIAN_POINT ( 'NONE',  ( -25.57103825560000132, -93.13207089489999646, -5.913928942570000125 ) ) ;
#3673 = CARTESIAN_POINT ( 'NONE',  ( -25.81706525379999917, -37.08699221940000257, -47.25782095779999992 ) ) ;
#3674 = ORIENTED_EDGE ( 'NONE', *, *, #10874, .T. ) ;
#3675 = FACE_OUTER_BOUND ( 'NONE', #4516, .T. ) ;
#3676 = CARTESIAN_POINT ( 'NONE',  ( -14.39310877959999857, -74.06193868690000670, 36.25276817999999679 ) ) ;
#3677 = CARTESIAN_POINT ( 'NONE',  ( -41.58198193041125279, -63.05619511567597613, -2.885163282589263911 ) ) ;
#3678 = FACE_OUTER_BOUND ( 'NONE', #18113, .T. ) ;
#3679 = ORIENTED_EDGE ( 'NONE', *, *, #22819, .T. ) ;
#3680 = CARTESIAN_POINT ( 'NONE',  ( 0.000000000000000000, -30.50310889129999836, 0.000000000000000000 ) ) ;
#3681 = AXIS2_PLACEMENT_3D ( 'NONE', #12739, #5638, #1702 ) ;
#3682 = CARTESIAN_POINT ( 'NONE',  ( -0.1749952543550000184, -101.1716782170000073, -15.73287486140000091 ) ) ;
#3683 = CARTESIAN_POINT ( 'NONE',  ( 7.752235230210000161, -60.58770331659999897, -22.38439241200000396 ) ) ;
#3684 = DIRECTION ( 'NONE',  ( 0.000000000000000000, 1.000000000000000000, 0.000000000000000000 ) ) ;
#3685 = CARTESIAN_POINT ( 'NONE',  ( 0.000000000000000000, -40.00000000000000000, 0.000000000000000000 ) ) ;
#3686 = CARTESIAN_POINT ( 'NONE',  ( -37.59243475499999931, -65.56519245710001087, 0.6307174998529999632 ) ) ;
#3687 = EDGE_LOOP ( 'NONE', ( #16165, #441, #27094, #27383 ) ) ;
#3689 = EDGE_CURVE ( 'NONE', #258, #2880, #22282, .T. ) ;
#3688 = VECTOR ( 'NONE', #27782, 1000.000000000000000 ) ;
#3690 = AXIS2_PLACEMENT_3D ( 'NONE', #24349, #4675, #24203 ) ;
#3691 = CIRCLE ( 'NONE', #23690, 5.499999999999998224 ) ;
#3692 = CARTESIAN_POINT ( 'NONE',  ( 6.678130984960001015, -101.3090757639999993, 14.82851652149999921 ) ) ;
#3693 = CARTESIAN_POINT ( 'NONE',  ( -14.75037098800590130, -92.63657771148726283, -24.06201644404302797 ) ) ;
#3694 = AXIS2_PLACEMENT_3D ( 'NONE', #15595, #24494, #6870 ) ;
#3695 = CARTESIAN_POINT ( 'NONE',  ( -5.344456951210212914, -96.89152197296419899, 20.58333059934093612 ) ) ;
#3696 = ADVANCED_FACE ( 'NONE', ( #17169 ), #10866, .T. ) ;
#3697 = LINE ( 'NONE', #6152, #1184 ) ;
#3698 = CARTESIAN_POINT ( 'NONE',  ( 4.391227679578132204, -92.82668962669040980, -30.18223191820092310 ) ) ;
#3699 = CARTESIAN_POINT ( 'NONE',  ( -8.022711211519999219E-16, -84.50000000000000000, 40.00000000000000000 ) ) ;
#3700 = CARTESIAN_POINT ( 'NONE',  ( -26.77683864449999973, -33.79999999999999716, -49.01467436490000296 ) ) ;
#3701 = CARTESIAN_POINT ( 'NONE',  ( 8.738006338790000882, -94.16701134370001114, -22.89272684270000013 ) ) ;
#3702 = CARTESIAN_POINT ( 'NONE',  ( 20.36793921130000129, -34.63244748730000566, -8.805019764629998136 ) ) ;
#3703 = CARTESIAN_POINT ( 'NONE',  ( -20.48493760250000051, -92.56290624670000966, -20.07155161329999871 ) ) ;
#3704 = CARTESIAN_POINT ( 'NONE',  ( 3.778423607708916165, -92.49999918154601630, 28.62985903013981215 ) ) ;
#3705 = ORIENTED_EDGE ( 'NONE', *, *, #865, .F. ) ;
#3706 = DIRECTION ( 'NONE',  ( 0.000000000000000000, 1.000000000000000000, 0.000000000000000000 ) ) ;
#3707 = DIRECTION ( 'NONE',  ( 0.3390050494208429743, 0.7071067811866730279, 0.6205445805637129775 ) ) ;
#3708 = EDGE_LOOP ( 'NONE', ( #20867, #9417, #11317, #1461 ) ) ;
#3709 = ORIENTED_EDGE ( 'NONE', *, *, #9383, .F. ) ;
#3710 = CIRCLE ( 'NONE', #8800, 2.000000000000000000 ) ;
#3711 = AXIS2_PLACEMENT_3D ( 'NONE', #20008, #20159, #20303 ) ;
#3712 = CARTESIAN_POINT ( 'NONE',  ( -0.8216454186400000692, -101.4254868690000109, -15.94813504319999709 ) ) ;
#3713 = CARTESIAN_POINT ( 'NONE',  ( -7.472969336320000266, -74.00000023179998720, 38.65569830309999588 ) ) ;
#3714 = CARTESIAN_POINT ( 'NONE',  ( 7.457144889719999448, -111.0000000000000000, 15.05426816870000017 ) ) ;
#3715 = CARTESIAN_POINT ( 'NONE',  ( 23.57312445299999837, -73.96004965659999186, -31.14713777060000055 ) ) ;
#3716 = DIRECTION ( 'NONE',  ( 0.000000000000000000, 1.000000000000000000, 0.000000000000000000 ) ) ;
#3717 = B_SPLINE_CURVE_WITH_KNOTS ( 'NONE', 5,
 ( #12270, #11985, #7913, #9941, #16798, #18855 ),
 .UNSPECIFIED., .F., .F.,
 ( 6, 6 ),
 ( -66.18347591719999912, -38.72099907209999969 ),
 .UNSPECIFIED. ) ;
#3718 = LINE ( 'NONE', #19306, #12948 ) ;
#3719 = CARTESIAN_POINT ( 'NONE',  ( -12.00784032640000021, -65.53745956570000430, -24.10472249089999863 ) ) ;
#3720 = CARTESIAN_POINT ( 'NONE',  ( 7.023816214479999154, -35.71220903070000219, -21.48235969790000155 ) ) ;
#3721 = LINE ( 'NONE', #19168, #3956 ) ;
#3722 = ORIENTED_EDGE ( 'NONE', *, *, #9583, .T. ) ;
#3723 = EDGE_CURVE ( 'NONE', #8492, #10101, #21815, .T. ) ;
#3724 = ORIENTED_EDGE ( 'NONE', *, *, #27470, .F. ) ;
#3725 = CIRCLE ( 'NONE', #8819, 0.5000000000000027756 ) ;
#3726 = CIRCLE ( 'NONE', #10656, 2.000000035460000269 ) ;
#3727 = EDGE_CURVE ( 'NONE', #24375, #11422, #26058, .T. ) ;
#3728 = CIRCLE ( 'NONE', #26518, 25.14975229270000057 ) ;
#3729 = VERTEX_POINT ( 'NONE', #17462 ) ;
#3730 = CARTESIAN_POINT ( 'NONE',  ( -2.567392390289999771, -60.04642514249999863, -25.10623713540000068 ) ) ;
#3731 = CARTESIAN_POINT ( 'NONE',  ( 16.73195129730000374, -84.75000000000000000, 30.62763141000000289 ) ) ;
#3732 = CARTESIAN_POINT ( 'NONE',  ( -0.7041684613104601809, -101.1586404113103583, -15.62090672338606190 ) ) ;
#3733 = LINE ( 'NONE', #10534, #18762 ) ;
#3734 = DIRECTION ( 'NONE',  ( 0.000000000000000000, 1.000000000000000000, 0.000000000000000000 ) ) ;
#3735 = ORIENTED_EDGE ( 'NONE', *, *, #19657, .F. ) ;
#3736 = CARTESIAN_POINT ( 'NONE',  ( -19.45768768673364590, -96.57210918401234778, -9.555941133991472825 ) ) ;
#3737 = ORIENTED_EDGE ( 'NONE', *, *, #17415, .T. ) ;
#3738 = DIRECTION ( 'NONE',  ( 0.000000000000000000, 1.000000000000000000, 0.000000000000000000 ) ) ;
#3739 = CARTESIAN_POINT ( 'NONE',  ( -14.03539743980000054, -80.18584161550000999, 36.72078694980000080 ) ) ;
#3740 = CIRCLE ( 'NONE', #20020, 2.000000000000001776 ) ;
#3741 = CARTESIAN_POINT ( 'NONE',  ( -18.79730758629999698, -18.50000000000000000, 15.05721160110000056 ) ) ;
#3742 = AXIS2_PLACEMENT_3D ( 'NONE', #25820, #21716, #26380 ) ;
#3743 = AXIS2_PLACEMENT_3D ( 'NONE', #4029, #6514, #4472 ) ;
#3744 = DIRECTION ( 'NONE',  ( 1.000000000000000000, 0.000000000000000000, 0.000000000000000000 ) ) ;
#3745 = DIRECTION ( 'NONE',  ( -1.000000000000000000, 0.000000000000000000, -6.123031769109999188E-17 ) ) ;
#3746 = CARTESIAN_POINT ( 'NONE',  ( 11.19714103559999963, -101.2141467319999890, -10.34781371220000068 ) ) ;
#3747 = ORIENTED_EDGE ( 'NONE', *, *, #13616, .T. ) ;
#3748 = CARTESIAN_POINT ( 'NONE',  ( 19.17604567300720575, -99.07183862241784311, -0.09086224700556182199 ) ) ;
#3749 = CARTESIAN_POINT ( 'NONE',  ( -12.56407913139999977, -101.6484611540000031, -9.907171035319999319 ) ) ;
#3750 = CARTESIAN_POINT ( 'NONE',  ( 36.70830968599999977, -79.00000000000000000, -14.75000000000000000 ) ) ;
#3751 = CARTESIAN_POINT ( 'NONE',  ( 0.000000000000000000, -110.0000000000000000, 0.000000000000000000 ) ) ;
#3752 = VERTEX_POINT ( 'NONE', #20485 ) ;
#3753 = EDGE_CURVE ( 'NONE', #26201, #5317, #553, .T. ) ;
#3754 = CARTESIAN_POINT ( 'NONE',  ( -41.70213186180765774, -65.10053925467518354, -2.815436737016979496 ) ) ;
#3755 = DIRECTION ( 'NONE',  ( -0.7071067811865475727, 0.000000000000000000, -0.7071067811865475727 ) ) ;
#3756 = CARTESIAN_POINT ( 'NONE',  ( 37.22080120100000045, -79.99999987929999179, -13.88618458220000029 ) ) ;
#3757 = ORIENTED_EDGE ( 'NONE', *, *, #7877, .F. ) ;
#3758 = EDGE_CURVE ( 'NONE', #23734, #25273, #21229, .T. ) ;
#3759 = DIRECTION ( 'NONE',  ( -0.9295286103719511139, 0.000000000000000000, -0.3687499999999862554 ) ) ;
#3760 = AXIS2_PLACEMENT_3D ( 'NONE', #3372, #25090, #21150 ) ;
#3761 = CARTESIAN_POINT ( 'NONE',  ( 11.70237128448379416, -101.1416252791438950, -10.22752515391487371 ) ) ;
#3762 = VECTOR ( 'NONE', #4180, 1000.000000000000000 ) ;
#3763 = ORIENTED_EDGE ( 'NONE', *, *, #18503, .F. ) ;
#3764 = CIRCLE ( 'NONE', #24724, 57.75000000000000000 ) ;
#3765 = CARTESIAN_POINT ( 'NONE',  ( 46.66508878058498766, -73.77886964734264552, -2.857274044103978561 ) ) ;
#3766 = ORIENTED_EDGE ( 'NONE', *, *, #16561, .T. ) ;
#3767 = CARTESIAN_POINT ( 'NONE',  ( 22.19837534649999711, -55.01779585689999408, 10.09345264070000070 ) ) ;
#3768 = CARTESIAN_POINT ( 'NONE',  ( -38.29314300141285088, -63.05597747387252383, 2.814055026004789184 ) ) ;
#3769 = CARTESIAN_POINT ( 'NONE',  ( -7.440556932039999793, -74.12472287219999600, -39.45553247920000217 ) ) ;
#3770 = ORIENTED_EDGE ( 'NONE', *, *, #2617, .T. ) ;
#3771 = CARTESIAN_POINT ( 'NONE',  ( -7.593125501599999438, -94.98812477769999418, -22.45811160230000070 ) ) ;
#3772 = DIRECTION ( 'NONE',  ( 1.000000000000000000, 0.000000000000000000, 0.000000000000000000 ) ) ;
#3773 = ADVANCED_FACE ( 'NONE', ( #23221 ), #10980, .T. ) ;
#3774 = VERTEX_POINT ( 'NONE', #6419 ) ;
#3775 = CARTESIAN_POINT ( 'NONE',  ( 21.92880676370000259, -37.95796630400000282, -8.677144394200000832 ) ) ;
#3776 = DIRECTION ( 'NONE',  ( 0.8775825618903718706, 0.000000000000000000, 0.4794255386042046152 ) ) ;
#3777 = CARTESIAN_POINT ( 'NONE',  ( -3.188346920221404535, -79.97866323289575519, 46.91088456186137989 ) ) ;
#3778 = ORIENTED_EDGE ( 'NONE', *, *, #4617, .F. ) ;
#3779 = CARTESIAN_POINT ( 'NONE',  ( -16.86871002079999826, -97.64874574800001028, -10.69232097959999983 ) ) ;
#3780 = CARTESIAN_POINT ( 'NONE',  ( 12.72815622549999937, -100.9364576079999978, -9.613728106940000018 ) ) ;
#3781 = CARTESIAN_POINT ( 'NONE',  ( -19.16019836899999618, -92.50000000000000000, 22.97842938279999814 ) ) ;
#3782 = CARTESIAN_POINT ( 'NONE',  ( 24.67022271940000167, -93.21603264559999502, -11.26210241870000139 ) ) ;
#3783 = EDGE_LOOP ( 'NONE', ( #20641, #8551, #19137, #10968 ) ) ;
#3784 = B_SPLINE_CURVE_WITH_KNOTS ( 'NONE', 5,
 ( #20373, #5784, #21374, #19186, #1433, #7840 ),
 .UNSPECIFIED., .F., .F.,
 ( 6, 6 ),
 ( 0.000000000000000000, 1.000000000000000000 ),
 .UNSPECIFIED. ) ;
#3785 = TOROIDAL_SURFACE ( 'NONE', #4728, 21.14285714289999873, 0.5000000000000000000 ) ;
#3786 = CARTESIAN_POINT ( 'NONE',  ( 0.000000000000000000, -15.50000000000000000, 0.000000000000000000 ) ) ;
#3787 = CARTESIAN_POINT ( 'NONE',  ( -38.25000000000000000, -65.31510159580000163, -2.337827133090000231 ) ) ;
#3788 = ORIENTED_EDGE ( 'NONE', *, *, #25987, .T. ) ;
#3789 = TOROIDAL_SURFACE ( 'NONE', #27550, 10.00000000000000000, 1.000000000000000000 ) ;
#3790 = EDGE_CURVE ( 'NONE', #6364, #12325, #4137, .T. ) ;
#3792 = EDGE_CURVE ( 'NONE', #24445, #9130, #13260, .T. ) ;
#3791 = CYLINDRICAL_SURFACE ( 'NONE', #20250, 9.500000000000001776 ) ;
#3793 = CIRCLE ( 'NONE', #13558, 0.9999999999999980016 ) ;
#3794 = CARTESIAN_POINT ( 'NONE',  ( -27.68682485439999752, -24.80000000000000071, -50.68039294919999804 ) ) ;
#3795 = CARTESIAN_POINT ( 'NONE',  ( 20.78253645173401409, -97.24405583786555951, 1.124206967171268001 ) ) ;
#3796 = FACE_OUTER_BOUND ( 'NONE', #7766, .T. ) ;
#3797 = CARTESIAN_POINT ( 'NONE',  ( -14.16469261447947403, -74.02381607010246967, 36.23209851156404682 ) ) ;
#3798 = ORIENTED_EDGE ( 'NONE', *, *, #25582, .T. ) ;
#3799 = CARTESIAN_POINT ( 'NONE',  ( -40.52471375025919542, -74.35734738351742124, -7.233314584366330457 ) ) ;
#3800 = EDGE_LOOP ( 'NONE', ( #12796, #28418, #1778, #10380 ) ) ;
#3801 = DIRECTION ( 'NONE',  ( 0.000000000000000000, -1.000000000000000000, 0.000000000000000000 ) ) ;
#3802 = CARTESIAN_POINT ( 'NONE',  ( 0.000000000000000000, -18.50000000000000000, 0.000000000000000000 ) ) ;
#3803 = ORIENTED_EDGE ( 'NONE', *, *, #20019, .F. ) ;
#3804 = VECTOR ( 'NONE', #8702, 999.9999999999998863 ) ;
#3805 = CARTESIAN_POINT ( 'NONE',  ( -12.54665039110000002, -101.1411470150000014, -8.912689559260000394 ) ) ;
#3806 = EDGE_CURVE ( 'NONE', #21689, #11679, #7438, .T. ) ;
#3807 = CARTESIAN_POINT ( 'NONE',  ( -16.07857726140000310, -92.61154353310000431, -23.75764880570000059 ) ) ;
#3808 = FACE_OUTER_BOUND ( 'NONE', #27249, .T. ) ;
#3809 = CARTESIAN_POINT ( 'NONE',  ( 7.592835430060000057, -49.11291935200000580, -21.85814127600000134 ) ) ;
#3810 = CARTESIAN_POINT ( 'NONE',  ( -39.64767024207763768, -65.69391135774336021, 2.235876747186491098 ) ) ;
#3811 = EDGE_LOOP ( 'NONE', ( #5199, #10682, #12686, #15097 ) ) ;
#3812 = EDGE_CURVE ( 'NONE', #28156, #18665, #11446, .T. ) ;
#3813 = DIRECTION ( 'NONE',  ( 0.4794255386042041156, 0.000000000000000000, 0.8775825618903720926 ) ) ;
#3814 = CARTESIAN_POINT ( 'NONE',  ( 22.56612536419999770, -34.67035637040000040, -0.2125348757979999836 ) ) ;
#3815 = CARTESIAN_POINT ( 'NONE',  ( 6.888451955769999913, -99.53431386179998697, 15.99365555089999802 ) ) ;
#3816 = ORIENTED_EDGE ( 'NONE', *, *, #2561, .F. ) ;
#3817 = CARTESIAN_POINT ( 'NONE',  ( 19.39105705749999942, -19.17889725919999933, -8.979483757040000569 ) ) ;
#3818 = EDGE_CURVE ( 'NONE', #26140, #7412, #16249, .T. ) ;
#3819 = CARTESIAN_POINT ( 'NONE',  ( -14.59815767989999991, -74.46648494389999939, 36.63377406709999917 ) ) ;
#3820 = DIRECTION ( 'NONE',  ( 0.000000000000000000, 1.000000000000000000, 0.000000000000000000 ) ) ;
#3821 = CARTESIAN_POINT ( 'NONE',  ( 25.81289538086879531, -93.01584921695616970, -5.657399889028498663 ) ) ;
#3822 = VERTEX_POINT ( 'NONE', #27131 ) ;
#3823 = DIRECTION ( 'NONE',  ( 0.7071067811865475727, 0.000000000000000000, -0.7071067811865475727 ) ) ;
#3824 = CARTESIAN_POINT ( 'NONE',  ( 0.05326513945900000074, -101.1417990620000040, -15.75792088070000041 ) ) ;
#3825 = CARTESIAN_POINT ( 'NONE',  ( 8.166636963089999313, -62.08211516050000256, -22.74134383390000025 ) ) ;
#3826 = CARTESIAN_POINT ( 'NONE',  ( 15.07154978059999983, -101.2141467319999890, 2.302521054160000080 ) ) ;
#3827 = CARTESIAN_POINT ( 'NONE',  ( 23.19089252530000422, -58.59418302210000462, 10.40173300340000040 ) ) ;
#3828 = CARTESIAN_POINT ( 'NONE',  ( -10.84908614390000103, -27.06313850649999964, -19.75281354290000024 ) ) ;
#3829 = CIRCLE ( 'NONE', #27591, 23.36116116979999902 ) ;
#3830 = VERTEX_POINT ( 'NONE', #27420 ) ;
#3831 = CARTESIAN_POINT ( 'NONE',  ( 6.101612763509999482, -100.4731125450000064, 15.00927834069999989 ) ) ;
#3832 = CARTESIAN_POINT ( 'NONE',  ( 14.89941269380000044, -101.1700440390000040, 3.486984464110000292 ) ) ;
#3833 = CARTESIAN_POINT ( 'NONE',  ( -2.903039748510000351, -94.98812477769999418, 23.52859306979999943 ) ) ;
#3834 = CARTESIAN_POINT ( 'NONE',  ( -32.68025371723170025, -74.50000000070002670, -21.81265875462274195 ) ) ;
#3835 = CARTESIAN_POINT ( 'NONE',  ( 21.21591776440000388, -18.50000000000000000, 0.5881982815080000204 ) ) ;
#3836 = LINE ( 'NONE', #21616, #12085 ) ;
#3837 = VERTEX_POINT ( 'NONE', #783 ) ;
#3838 = CARTESIAN_POINT ( 'NONE',  ( 1.951203915629999841, -92.83702889919999279, -29.73265166020000194 ) ) ;
#3839 = CARTESIAN_POINT ( 'NONE',  ( 7.025840212360933812, -101.6484611540000174, 14.37514525054935532 ) ) ;
#3840 = CARTESIAN_POINT ( 'NONE',  ( -5.969238273050000210, -101.2530993000000024, 13.97222956270000083 ) ) ;
#3841 = VERTEX_POINT ( 'NONE', #16331 ) ;
#3842 = AXIS2_PLACEMENT_3D ( 'NONE', #10703, #2152, #4030 ) ;
#3843 = DIRECTION ( 'NONE',  ( 0.000000000000000000, 1.000000000000000000, 0.000000000000000000 ) ) ;
#3844 = AXIS2_PLACEMENT_3D ( 'NONE', #17313, #8267, #14423 ) ;
#3845 = CARTESIAN_POINT ( 'NONE',  ( -12.89684236643334536, -100.4010812938312114, -11.04552942129398474 ) ) ;
#3846 = ORIENTED_EDGE ( 'NONE', *, *, #3030, .F. ) ;
#3847 = EDGE_CURVE ( 'NONE', #21458, #17507, #28791, .T. ) ;
#3848 = AXIS2_PLACEMENT_3D ( 'NONE', #11497, #7742, #16608 ) ;
#3849 = EDGE_CURVE ( 'NONE', #11391, #17271, #11098, .T. ) ;
#3850 = B_SPLINE_CURVE_WITH_KNOTS ( 'NONE', 5,
 ( #26775, #26469, #24571, #6806, #6504, #4320 ),
 .UNSPECIFIED., .F., .F.,
 ( 6, 6 ),
 ( 0.000000000000000000, 1.000000000000000000 ),
 .UNSPECIFIED. ) ;
#3851 = CARTESIAN_POINT ( 'NONE',  ( -1.062521193220000049, -101.1516803200000112, -15.28978926900000168 ) ) ;
#3852 = DIRECTION ( 'NONE',  ( 0.000000000000000000, 1.000000000000000000, 0.000000000000000000 ) ) ;
#3853 = DIRECTION ( 'NONE',  ( 0.000000000000000000, 1.000000000000000000, 0.000000000000000000 ) ) ;
#3854 = ADVANCED_FACE ( 'NONE', ( #21005 ), #14838, .T. ) ;
#3855 = CARTESIAN_POINT ( 'NONE',  ( 19.62372718079999956, -18.50000000000000000, -7.547414732120000913 ) ) ;
#3856 = EDGE_CURVE ( 'NONE', #26695, #16270, #19897, .T. ) ;
#3857 = DIRECTION ( 'NONE',  ( 0.8775825618903722036, 0.000000000000000000, -0.4794255386042041156 ) ) ;
#3858 = PRODUCT_DEFINITION_SHAPE ( 'NONE', 'NONE',  #4003 ) ;
#3859 = AXIS2_PLACEMENT_3D ( 'NONE', #555, #7685, #14076 ) ;
#3860 = CARTESIAN_POINT ( 'NONE',  ( 38.57396449699999863, -80.00000000000000000, -9.597487326430000465 ) ) ;
#3861 = CARTESIAN_POINT ( 'NONE',  ( -18.53437987951083343, -19.46453794990133446, 12.04470810626642496 ) ) ;
#3862 = CARTESIAN_POINT ( 'NONE',  ( -37.25000000000000000, -65.00000000000000000, 1.587713240270000048 ) ) ;
#3863 = VERTEX_POINT ( 'NONE', #11953 ) ;
#3864 = CARTESIAN_POINT ( 'NONE',  ( 8.616470839319999797, -18.62200669790000163, -19.27348050239999822 ) ) ;
#3865 = VERTEX_POINT ( 'NONE', #14564 ) ;
#3866 = DIRECTION ( 'NONE',  ( 0.2414462220490750377, 0.000000000000000000, 0.9704142011833034598 ) ) ;
#3867 = AXIS2_PLACEMENT_3D ( 'NONE', #25612, #24378, #6452 ) ;
#3868 = CARTESIAN_POINT ( 'NONE',  ( 7.049162187834887128, -36.56981903923507815, -21.51316594787862968 ) ) ;
#3869 = CARTESIAN_POINT ( 'NONE',  ( -29.42137572429999892, -92.83702889919999279, 4.713854256609999460 ) ) ;
#3870 = DIRECTION ( 'NONE',  ( 0.000000000000000000, -1.000000000000000000, 0.000000000000000000 ) ) ;
#3871 = ORIENTED_EDGE ( 'NONE', *, *, #27031, .F. ) ;
#3872 = CIRCLE ( 'NONE', #8523, 0.5000000000000027756 ) ;
#3873 = CARTESIAN_POINT ( 'NONE',  ( 21.48176983620000158, -36.17740064299999858, -7.146355372150000385 ) ) ;
#3874 = ORIENTED_EDGE ( 'NONE', *, *, #25383, .T. ) ;
#3875 = LINE ( 'NONE', #12189, #14945 ) ;
#3876 = B_SPLINE_CURVE_WITH_KNOTS ( 'NONE', 3,
 ( #13923, #22825, #7091, #698, #20328, #11427, #11283, #9551, #24859, #263, #18452, #27336, #7379, #3021, #2578, #11876, #27047, #401, #843, #18598, #9686, #27490, #3434, #28559, #21865, #23113, #4083, #10759, #17352, #8449 ),
 .UNSPECIFIED., .F., .F.,
 ( 4, 1, 1, 1, 1, 2, 2, 1, 1, 1, 1, 2, 2, 2, 1, 1, 1, 1, 2, 2, 4 ),
 ( 0.000000000000000000, 0.1250000000000514866, 0.1875000000000766054, 0.2187500000000884848, 0.2343750000000944245, 0.2421875000000983380, 0.2500000000001022515, 0.3750000000001702527, 0.4375000000002042810, 0.4687500000002198797, 0.4843750000002277067, 0.4921875000002299827, 0.5000000000002322587, 0.6250000000002787770, 0.6875000000003004264, 0.7187500000003108624, 0.7343750000003180789, 0.7421875000003219647, 0.7460937500003220757, 0.7500000000003222977, 1.000000000000000000 ),
 .UNSPECIFIED. ) ;
#3877 = ORIENTED_EDGE ( 'NONE', *, *, #7823, .F. ) ;
#3878 = ADVANCED_FACE ( 'NONE', ( #27712 ), #8262, .T. ) ;
#3879 = AXIS2_PLACEMENT_3D ( 'NONE', #18190, #19921, #24599 ) ;
#3880 = CARTESIAN_POINT ( 'NONE',  ( 38.62788938250000115, -74.00000000000000000, 7.627566167509999495 ) ) ;
#3881 = ADVANCED_FACE ( 'NONE', ( #28114 ), #6603, .F. ) ;
#3882 = CARTESIAN_POINT ( 'NONE',  ( -15.10594828610000029, -101.1292389759999963, 3.502950928120000196 ) ) ;
#3883 = CARTESIAN_POINT ( 'NONE',  ( -32.19064304186151304, -74.02457476353460208, -22.07217569486996211 ) ) ;
#3884 = CARTESIAN_POINT ( 'NONE',  ( 11.30123137200000016, -101.2530993039999885, -10.15784976960000030 ) ) ;
#3885 = EDGE_LOOP ( 'NONE', ( #20754, #16012, #24364, #7146, #24038 ) ) ;
#3886 = CARTESIAN_POINT ( 'NONE',  ( 0.000000000000000000, -34.10310889129999623, 0.000000000000000000 ) ) ;
#3887 = CARTESIAN_POINT ( 'NONE',  ( -12.42321381640000055, -101.0405520670000072, -10.47065562140000061 ) ) ;
#3888 = CARTESIAN_POINT ( 'NONE',  ( 16.58537890990000108, -94.98812477769999418, 16.93952572510000110 ) ) ;
#3889 = DIRECTION ( 'NONE',  ( 1.000000000000000000, 0.000000000000000000, 0.000000000000000000 ) ) ;
#3890 = ORIENTED_EDGE ( 'NONE', *, *, #7784, .T. ) ;
#3891 = CIRCLE ( 'NONE', #17855, 0.4999999999999986677 ) ;
#3892 = CIRCLE ( 'NONE', #27660, 9.500000000000001776 ) ;
#3893 = CARTESIAN_POINT ( 'NONE',  ( 8.611776762660001694, -37.95567967650000440, -21.87916666729999804 ) ) ;
#3894 = CARTESIAN_POINT ( 'NONE',  ( -32.08437107960000390, -74.00884812510000188, -21.94309233420000282 ) ) ;
#3895 = CARTESIAN_POINT ( 'NONE',  ( 36.73391533630000083, -79.36276986969998859, -14.70890631340000176 ) ) ;
#3896 = VERTEX_POINT ( 'NONE', #21836 ) ;
#3897 = B_SPLINE_CURVE_WITH_KNOTS ( 'NONE', 5,
 ( #24150, #22407, #8828, #24291, #13498, #11150, #26787, #17745, #26337 ),
 .UNSPECIFIED., .F., .F.,
 ( 6, 3, 6 ),
 ( 0.000000000000000000, 0.5000000000000000000, 1.000000000000000000 ),
 .UNSPECIFIED. ) ;
#3898 = B_SPLINE_CURVE_WITH_KNOTS ( 'NONE', 3,
 ( #1164, #7838, #16720, #25616, #5646, #2756, #21795, #1574, #7975, #10691, #19609, #10414, #8378, #23698, #1852, #23984, #10134, #8530, #1431, #17433, #5914, #12879, #17285, #12605 ),
 .UNSPECIFIED., .F., .F.,
 ( 4, 2, 2, 1, 1, 1, 2, 2, 2, 1, 1, 1, 2, 2, 4 ),
 ( 0.000000000000000000, 0.2500000000000677236, 0.3750000000000931477, 0.4375000000000944800, 0.4687500000000965339, 0.4843750000000887068, 0.4921875000000847655, 0.5000000000000808242, 0.6249999999998875344, 0.6874999999997915001, 0.7187499999997323252, 0.7343749999997239986, 0.7421874999997207789, 0.7499999999997175593, 1.000000000000000000 ),
 .UNSPECIFIED. ) ;
#3899 = CARTESIAN_POINT ( 'NONE',  ( 6.920191221405996629, -100.2392017795743158, 15.64847181329894887 ) ) ;
#3900 = CARTESIAN_POINT ( 'NONE',  ( -0.7685659013399879225, -79.79239604273577413, 47.20921231312638611 ) ) ;
#3901 = ORIENTED_EDGE ( 'NONE', *, *, #18873, .T. ) ;
#3902 = CARTESIAN_POINT ( 'NONE',  ( 47.25008975959999447, -74.83017303949999643, -0.5756401097749999085 ) ) ;
#3903 = ORIENTED_EDGE ( 'NONE', *, *, #8336, .T. ) ;
#3904 = CARTESIAN_POINT ( 'NONE',  ( 29.18096563980000013, -92.50000947299999154, 6.925280479609999595 ) ) ;
#3905 = FACE_OUTER_BOUND ( 'NONE', #16674, .T. ) ;
#3906 = CARTESIAN_POINT ( 'NONE',  ( -7.562763921490000207, -74.00035141509999903, -39.03055149349999908 ) ) ;
#3907 = ORIENTED_EDGE ( 'NONE', *, *, #6058, .T. ) ;
#3908 = CARTESIAN_POINT ( 'NONE',  ( -4.660534226913422451, -96.57210917874438394, -21.17066465899685213 ) ) ;
#3909 = CARTESIAN_POINT ( 'NONE',  ( 22.68565687649710227, -36.18510625669999570, -10.42651188819920094 ) ) ;
#3910 = EDGE_CURVE ( 'NONE', #23740, #14954, #7369, .T. ) ;
#3911 = EDGE_CURVE ( 'NONE', #640, #13903, #412, .T. ) ;
#3912 = CIRCLE ( 'NONE', #28129, 0.5000000000000012212 ) ;
#3913 = CARTESIAN_POINT ( 'NONE',  ( -36.23922253580000330, -74.50000000000000000, -26.33972759919999973 ) ) ;
#3914 = CARTESIAN_POINT ( 'NONE',  ( -21.91154649879999994, -92.53610956480000027, -19.81987556260000005 ) ) ;
#3915 = LINE ( 'NONE', #19088, #26957 ) ;
#3916 = VERTEX_POINT ( 'NONE', #1890 ) ;
#3917 = DIRECTION ( 'NONE',  ( 0.8775825618903724257, 0.000000000000000000, 0.4794255386042036160 ) ) ;
#3918 = CARTESIAN_POINT ( 'NONE',  ( 12.86423915559999998, -101.1412505549999992, -9.792936688159999292 ) ) ;
#3919 = CARTESIAN_POINT ( 'NONE',  ( 7.418111264149999342E-16, -69.50000000000000000, -33.25000000000000000 ) ) ;
#3920 = CARTESIAN_POINT ( 'NONE',  ( 23.32816514950000197, -93.91547326110000427, -8.285286069360001449 ) ) ;
#3921 = VERTEX_POINT ( 'NONE', #14971 ) ;
#3922 = AXIS2_PLACEMENT_3D ( 'NONE', #27351, #5349, #20802 ) ;
#3923 = CARTESIAN_POINT ( 'NONE',  ( 29.77631732523176566, -92.68577957616035690, 6.604815473007913162 ) ) ;
#3924 = CARTESIAN_POINT ( 'NONE',  ( -38.25000000000000000, -65.17124718639999514, -2.640283750789999662 ) ) ;
#3925 = ORIENTED_EDGE ( 'NONE', *, *, #17240, .F. ) ;
#3926 = CARTESIAN_POINT ( 'NONE',  ( 21.79230230059999940, -37.95144147500000287, -8.472395268590000583 ) ) ;
#3927 = DIRECTION ( 'NONE',  ( 0.4794255386042040046, 0.000000000000000000, 0.8775825618903722036 ) ) ;
#3928 = CARTESIAN_POINT ( 'NONE',  ( 6.139035473192171466, -92.73901256242973545, 28.87717835461170424 ) ) ;
#3929 = CARTESIAN_POINT ( 'NONE',  ( 22.96745989159999723, -18.50000000000000000, 9.091461454319999191 ) ) ;
#3930 = CARTESIAN_POINT ( 'NONE',  ( -38.66568593819999933, -65.21397798589998729, 2.791092524920000262 ) ) ;
#3931 = DIRECTION ( 'NONE',  ( 0.000000000000000000, 1.000000000000000000, 0.000000000000000000 ) ) ;
#3932 = EDGE_CURVE ( 'NONE', #8854, #9278, #13385, .T. ) ;
#3933 = CARTESIAN_POINT ( 'NONE',  ( 0.000000000000000000, 0.000000000000000000, 0.000000000000000000 ) ) ;
#3934 = AXIS2_PLACEMENT_3D ( 'NONE', #18719, #7656, #20306 ) ;
#3935 = ORIENTED_EDGE ( 'NONE', *, *, #1821, .T. ) ;
#3936 = CARTESIAN_POINT ( 'NONE',  ( 19.53732555980000285, -35.60472305269999538, -8.991793591719998702 ) ) ;
#3937 = VERTEX_POINT ( 'NONE', #17038 ) ;
#3938 = CARTESIAN_POINT ( 'NONE',  ( 19.93895660729999975, -35.91131188369999450, -9.181219786679999828 ) ) ;
#3939 = DIRECTION ( 'NONE',  ( 0.09756097560976770278, 0.000000000000000000, 0.9952295494196654602 ) ) ;
#3940 = EDGE_LOOP ( 'NONE', ( #3816, #24067, #10685, #2239 ) ) ;
#3941 = CARTESIAN_POINT ( 'NONE',  ( -13.19565947609999945, -101.4334236450000049, -9.166987053370000638 ) ) ;
#3942 = EDGE_CURVE ( 'NONE', #4043, #7539, #2730, .T. ) ;
#3943 = CARTESIAN_POINT ( 'NONE',  ( -14.07810103419999948, -92.69822489080000594, -24.05355070809999773 ) ) ;
#3944 = CARTESIAN_POINT ( 'NONE',  ( -7.946020008919999711, -100.0482783049999966, 15.24923535169999944 ) ) ;
#3945 = AXIS2_PLACEMENT_3D ( 'NONE', #16672, #10093, #19012 ) ;
#3946 = DIRECTION ( 'NONE',  ( 0.000000000000000000, -1.000000000000000000, 0.000000000000000000 ) ) ;
#3947 = CARTESIAN_POINT ( 'NONE',  ( 19.90557383419769266, -34.65022531193147159, -8.965967189900016621 ) ) ;
#3948 = FACE_OUTER_BOUND ( 'NONE', #26376, .T. ) ;
#3949 = CARTESIAN_POINT ( 'NONE',  ( 6.114061450890000415, -101.1889999979999999, -13.40104985119999981 ) ) ;
#3950 = ORIENTED_EDGE ( 'NONE', *, *, #14642, .T. ) ;
#3951 = CARTESIAN_POINT ( 'NONE',  ( 12.62420072685640271, -101.5740747342616856, -9.923100141449944900 ) ) ;
#3952 = CARTESIAN_POINT ( 'NONE',  ( 22.95539802729999579, -27.05112424559999695, 1.027418781419999982 ) ) ;
#3953 = CARTESIAN_POINT ( 'NONE',  ( 25.28698659450000363, -67.37930764479999368, 10.90088209369999994 ) ) ;
#3954 = CARTESIAN_POINT ( 'NONE',  ( 9.015422398089999234, -94.52293512109999085, -22.16844759350000160 ) ) ;
#3955 = ORIENTED_EDGE ( 'NONE', *, *, #9552, .F. ) ;
#3956 = VECTOR ( 'NONE', #9738, 1000.000000000000000 ) ;
#3957 = CARTESIAN_POINT ( 'NONE',  ( -23.77081188420000046, -91.50000000000000000, -19.11016751280000037 ) ) ;
#3958 = B_SPLINE_CURVE_WITH_KNOTS ( 'NONE', 3,
 ( #14342, #23378, #23238, #10086, #25563, #21058, #1117, #12285, #11862, #21194, #9671, #9532, #5171, #7929, #14055, #27475, #25709 ),
 .UNSPECIFIED., .F., .F.,
 ( 4, 2, 2, 1, 1, 1, 1, 1, 2, 2, 4 ),
 ( 0.000000000000000000, 0.2500000000000325295, 0.3750000000000475175, 0.4375000000000550116, 0.4687500000000596745, 0.4843750000000613398, 0.4921875000000622280, 0.4960937500000626721, 0.4980468750000630607, 0.5000000000000635048, 1.000000000000000000 ),
 .UNSPECIFIED. ) ;
#3959 = CARTESIAN_POINT ( 'NONE',  ( -38.71641004229999794, -73.50000000000000000, 7.135467526410000261 ) ) ;
#3960 = CARTESIAN_POINT ( 'NONE',  ( -41.51316926232986049, -63.06504043304238394, -2.884616214739031737 ) ) ;
#3961 = CARTESIAN_POINT ( 'NONE',  ( -20.54704754939906763, -92.97190650805515588, 17.33505249212057819 ) ) ;
#3962 = ORIENTED_EDGE ( 'NONE', *, *, #6296, .T. ) ;
#3963 = CARTESIAN_POINT ( 'NONE',  ( 28.27563371580000151, -71.49912264920001803, 2.269389644629999925 ) ) ;
#3964 = B_SPLINE_CURVE_WITH_KNOTS ( 'NONE', 3,
 ( #2672, #15611, #24512, #4548 ),
 .UNSPECIFIED., .F., .F.,
 ( 4, 4 ),
 ( -19.56549066489999689, -15.82800262790000012 ),
 .UNSPECIFIED. ) ;
#3965 = CARTESIAN_POINT ( 'NONE',  ( 9.020398574519999713, -35.69157542760000013, -19.55164510480000217 ) ) ;
#3966 = CARTESIAN_POINT ( 'NONE',  ( 9.629159357529998076, -60.22022526889999483, -23.71524624790000146 ) ) ;
#3967 = CARTESIAN_POINT ( 'NONE',  ( -12.07720592679999960, -68.19952391640001110, -25.04943555990000448 ) ) ;
#3968 = CARTESIAN_POINT ( 'NONE',  ( 22.89499695709999827, -58.22369335140000146, 10.25598920059999841 ) ) ;
#3969 = FACE_OUTER_BOUND ( 'NONE', #27510, .T. ) ;
#3970 = ORIENTED_EDGE ( 'NONE', *, *, #23115, .T. ) ;
#3971 = EDGE_CURVE ( 'NONE', #9596, #6780, #3192, .T. ) ;
#3972 = CARTESIAN_POINT ( 'NONE',  ( 6.274723105890000596, -100.5027207520000019, 14.99162967899999899 ) ) ;
#3973 = CARTESIAN_POINT ( 'NONE',  ( 15.52324312520000049, -101.3138676899999950, 3.505211958319999876 ) ) ;
#3974 = CARTESIAN_POINT ( 'NONE',  ( -5.720570170225761863, -97.24405583566215228, 20.01131529210075755 ) ) ;
#3975 = CARTESIAN_POINT ( 'NONE',  ( -40.00000000000000000, -84.00000000000000000, -8.881784197000000993E-16 ) ) ;
#3976 = DIRECTION ( 'NONE',  ( 0.000000000000000000, 1.000000000000000000, 0.000000000000000000 ) ) ;
#3977 = EDGE_CURVE ( 'NONE', #21398, #24310, #21890, .T. ) ;
#3978 = DIRECTION ( 'NONE',  ( 0.7506477800816132584, 0.000000000000000000, -0.6607025883546591150 ) ) ;
#3979 = ORIENTED_EDGE ( 'NONE', *, *, #14699, .T. ) ;
#3980 = CARTESIAN_POINT ( 'NONE',  ( 6.576566045489999901, -93.21603264559999502, -26.30976280700000203 ) ) ;
#3981 = CARTESIAN_POINT ( 'NONE',  ( 0.000000000000000000, -35.29999999999999716, 0.000000000000000000 ) ) ;
#3982 = CARTESIAN_POINT ( 'NONE',  ( -6.522510977999999682, -101.1411470200000053, 13.93862250449999785 ) ) ;
#3983 = ORIENTED_EDGE ( 'NONE', *, *, #25055, .T. ) ;
#3984 = CARTESIAN_POINT ( 'NONE',  ( -14.65665286289999969, -79.25000000000000000, 36.94583910070000599 ) ) ;
#3985 = DIRECTION ( 'NONE',  ( -0.7071067811865470176, 0.000000000000000000, 0.7071067811865480168 ) ) ;
#3986 = ORIENTED_EDGE ( 'NONE', *, *, #14508, .F. ) ;
#3987 = CARTESIAN_POINT ( 'NONE',  ( 23.63615965700000032, -94.63960343439998724, -2.179844538739999837 ) ) ;
#3988 = EDGE_LOOP ( 'NONE', ( #1397, #1967, #22313, #27858 ) ) ;
#3989 = CARTESIAN_POINT ( 'NONE',  ( -1.200716280800000035, -101.4309749570000037, -16.11926675319999802 ) ) ;
#3990 = CARTESIAN_POINT ( 'NONE',  ( 21.65058109989999835, -18.61782386119999799, -0.1214948449970000149 ) ) ;
#3991 = DIRECTION ( 'NONE',  ( 1.000000000000000000, 0.000000000000000000, 0.000000000000000000 ) ) ;
#3992 = CARTESIAN_POINT ( 'NONE',  ( 14.40601943769999949, -92.50000000000000000, 26.88338899689999906 ) ) ;
#3993 = CARTESIAN_POINT ( 'NONE',  ( -6.708539788989999586, -101.2358105800000061, 13.65871639999999942 ) ) ;
#3994 = DIRECTION ( 'NONE',  ( 0.000000000000000000, 1.000000000000000000, 0.000000000000000000 ) ) ;
#3995 = CARTESIAN_POINT ( 'NONE',  ( 13.77368720893815635, -100.0863963177836666, -10.35768808805547181 ) ) ;
#3996 = CARTESIAN_POINT ( 'NONE',  ( -18.71988641671584119, -19.47731532785768849, 13.50356754889457100 ) ) ;
#3997 = CARTESIAN_POINT ( 'NONE',  ( 7.100559683520000220, -35.25283571269999783, -21.44183144160000154 ) ) ;
#3998 = AXIS2_PLACEMENT_3D ( 'NONE', #5896, #21352, #4139 ) ;
#3999 = DIRECTION ( 'NONE',  ( 0.8172561201429209277, 0.000000000000000000, 0.5762746169049438594 ) ) ;
#4000 = ORIENTED_EDGE ( 'NONE', *, *, #16564, .F. ) ;
#4001 = CARTESIAN_POINT ( 'NONE',  ( 36.74383114260000127, -74.66666666670001007, -14.69280904159999857 ) ) ;
#4002 = CARTESIAN_POINT ( 'NONE',  ( -39.50000000000000000, -63.30468293320000583, 2.309401076760000393 ) ) ;
#4003 = PRODUCT_DEFINITION ( 'UNKNOWN', '', #19919, #4811 ) ;
#4004 = EDGE_CURVE ( 'NONE', #20846, #10652, #27375, .T. ) ;
#4005 = CARTESIAN_POINT ( 'NONE',  ( -1.348885035479999939, -65.00127796780000722, -25.13407207219999862 ) ) ;
#4006 = B_SPLINE_CURVE_WITH_KNOTS ( 'NONE', 5,
 ( #14237, #14085, #25319, #9699, #18613, #20942, #7554, #10111, #19031 ),
 .UNSPECIFIED., .F., .F.,
 ( 6, 3, 6 ),
 ( 0.000000000000000000, 0.5000000000000000000, 1.000000000000000000 ),
 .UNSPECIFIED. ) ;
#4007 = EDGE_CURVE ( 'NONE', #17905, #20759, #10567, .T. ) ;
#4008 = CARTESIAN_POINT ( 'NONE',  ( -25.22186920720000103, -94.24983875570001146, -3.042057529720000097 ) ) ;
#4009 = CARTESIAN_POINT ( 'NONE',  ( -19.56318090859999970, -55.04870336940000186, 12.97254176369999890 ) ) ;
#4010 = ADVANCED_FACE ( 'NONE', ( #22134 ), #6384, .T. ) ;
#4011 = DIRECTION ( 'NONE',  ( 0.000000000000000000, 1.000000000000000000, 0.000000000000000000 ) ) ;
#4012 = VERTEX_POINT ( 'NONE', #1610 ) ;
#4013 = CARTESIAN_POINT ( 'NONE',  ( -22.29269500190000386, -94.98812477769999418, -8.065858985560000249 ) ) ;
#4014 = CARTESIAN_POINT ( 'NONE',  ( -13.31136841900000078, -101.0685845459999967, -9.042836269629999535 ) ) ;
#4015 = EDGE_LOOP ( 'NONE', ( #18351, #27042 ) ) ;
#4016 = CARTESIAN_POINT ( 'NONE',  ( -40.00000000000000000, -94.00000000000000000, 0.000000000000000000 ) ) ;
#4017 = CARTESIAN_POINT ( 'NONE',  ( -14.30456952449999797, -80.50000235099999202, 36.55186667960000335 ) ) ;
#4018 = CARTESIAN_POINT ( 'NONE',  ( -17.81645507309999843, -18.50000000000000000, 13.97041869859999963 ) ) ;
#4019 = CARTESIAN_POINT ( 'NONE',  ( 21.88295226250000169, -19.17792668139999890, 9.573516633400002362 ) ) ;
#4020 = CARTESIAN_POINT ( 'NONE',  ( -32.46498206463285641, -74.10093221338760827, -22.13944811776638133 ) ) ;
#4021 = CARTESIAN_POINT ( 'NONE',  ( 11.15108825559999950, -100.9197081840000010, -10.94438638200000113 ) ) ;
#4022 = B_SPLINE_SURFACE_WITH_KNOTS ( 'NONE', 5, 5, ( 
 ( #6856, #15576, #15421, #8585, #24332, #15718, #2053, #4663, #13388 ),
 ( #22449, #24479, #22292, #2495, #1905, #15267, #11349, #20253, #320 ),
 ( #4372, #22005, #10894, #10747, #19659, #4218, #2341, #13244, #11194 ),
 ( #20106, #4512, #17342, #28549, #8868, #15125, #24034, #17488, #22152 ),
 ( #26372, #6400, #2191, #24187, #13093, #8714, #11031, #6560, #17781 ),
 ( #28681, #17634, #26520, #26669, #6710, #7297, #14139, #909, #9751 ) ),
 .UNSPECIFIED., .F., .F., .F.,
 ( 6, 6 ),
 ( 6, 3, 6 ),
 ( 10.27982891500000129, 28.98450582939999975 ),
 ( 0.000000000000000000, 0.2500000000000000000, 0.5000000000000000000 ),
 .UNSPECIFIED. ) ;
#4023 = VERTEX_POINT ( 'NONE', #24020 ) ;
#4024 = CARTESIAN_POINT ( 'NONE',  ( 27.68682485439999752, -24.80000000000000071, 50.68039294919999804 ) ) ;
#4025 = CARTESIAN_POINT ( 'NONE',  ( -12.44597910190000079, -100.6809449770000100, -10.73533039990000049 ) ) ;
#4026 = DIRECTION ( 'NONE',  ( 0.000000000000000000, 0.000000000000000000, -1.000000000000000000 ) ) ;
#4027 = CARTESIAN_POINT ( 'NONE',  ( -7.129748092820078931, -101.5409490182324532, 14.41619968365793625 ) ) ;
#4028 = ORIENTED_EDGE ( 'NONE', *, *, #15849, .T. ) ;
#4029 = CARTESIAN_POINT ( 'NONE',  ( 6.623136366559999821, -93.00000000000000000, -29.58057261400000115 ) ) ;
#4030 = DIRECTION ( 'NONE',  ( 1.000000000000000000, 0.000000000000000000, 0.000000000000000000 ) ) ;
#4031 = ORIENTED_EDGE ( 'NONE', *, *, #1746, .T. ) ;
#4032 = EDGE_CURVE ( 'NONE', #20809, #24813, #4094, .T. ) ;
#4033 = CARTESIAN_POINT ( 'NONE',  ( 36.79450594634548111, -79.51015800609961559, -14.61067903185865013 ) ) ;
#4034 = CARTESIAN_POINT ( 'NONE',  ( -5.582122996319999864, -100.8816831189999874, 14.77497816989999890 ) ) ;
#4035 = DIRECTION ( 'NONE',  ( -0.7071067811865457964, 0.000000000000000000, -0.7071067811865492381 ) ) ;
#4036 = EDGE_CURVE ( 'NONE', #6381, #26221, #13076, .T. ) ;
#4037 = VERTEX_POINT ( 'NONE', #21985 ) ;
#4038 = CARTESIAN_POINT ( 'NONE',  ( -19.90809684629999765, -55.86335041469999396, 12.11525402310000032 ) ) ;
#4039 = CARTESIAN_POINT ( 'NONE',  ( -19.99038385860702505, -95.81012667687654982, 9.711302805237647107 ) ) ;
#4040 = ORIENTED_EDGE ( 'NONE', *, *, #20407, .T. ) ;
#4041 = CARTESIAN_POINT ( 'NONE',  ( 20.56950839670000164, -55.05548131559999803, 10.89901456070000130 ) ) ;
#4042 = DIRECTION ( 'NONE',  ( 0.9952295494196653491, 0.000000000000000000, -0.09756097560976997873 ) ) ;
#4043 = VERTEX_POINT ( 'NONE', #2033 ) ;
#4044 = CARTESIAN_POINT ( 'NONE',  ( -41.78262379717566688, -65.71460843033148080, 1.333804927987287225 ) ) ;
#4045 = CARTESIAN_POINT ( 'NONE',  ( 0.000000000000000000, -102.5000000000000000, 0.000000000000000000 ) ) ;
#4046 = AXIS2_PLACEMENT_3D ( 'NONE', #21478, #28178, #1534 ) ;
#4047 = DIRECTION ( 'NONE',  ( 0.5301416321220552286, 0.000000000000000000, 0.8479091047340884257 ) ) ;
#4048 = CARTESIAN_POINT ( 'NONE',  ( -11.48284226354935988, -58.59018045370876138, -22.64916359960036729 ) ) ;
#4049 = CARTESIAN_POINT ( 'NONE',  ( -2.792231499789999738, -18.50000000000000000, -21.92192335580000062 ) ) ;
#4050 = EDGE_LOOP ( 'NONE', ( #11231, #3153, #12446, #23594 ) ) ;
#4051 = CARTESIAN_POINT ( 'NONE',  ( 25.14694229440000228, -65.07443093669999712, -0.3759436444569999591 ) ) ;
#4052 = CARTESIAN_POINT ( 'NONE',  ( 12.84172902559999940, -100.7776802639999971, -9.219477447620000987 ) ) ;
#4053 = DIRECTION ( 'NONE',  ( 0.000000000000000000, -1.000000000000000000, 0.000000000000000000 ) ) ;
#4054 = ORIENTED_EDGE ( 'NONE', *, *, #25632, .F. ) ;
#4055 = AXIS2_PLACEMENT_3D ( 'NONE', #26440, #21921, #26878 ) ;
#4056 = CARTESIAN_POINT ( 'NONE',  ( 29.83256477045206623, -92.59735406127096269, 6.345759108124658709 ) ) ;
#4057 = CARTESIAN_POINT ( 'NONE',  ( -19.59431184860000030, -18.62337006899999992, 14.76282615579999913 ) ) ;
#4058 = ORIENTED_EDGE ( 'NONE', *, *, #4331, .F. ) ;
#4059 = DIRECTION ( 'NONE',  ( 1.000000000000000000, 0.000000000000000000, 0.000000000000000000 ) ) ;
#4060 = B_SPLINE_CURVE_WITH_KNOTS ( 'NONE', 5,
 ( #9305, #5523, #25630, #1046, #16737, #7442 ),
 .UNSPECIFIED., .F., .F.,
 ( 6, 6 ),
 ( -7.329014384030000606, -6.713731535029999975 ),
 .UNSPECIFIED. ) ;
#4061 = LINE ( 'NONE', #17773, #28738 ) ;
#4062 = FACE_OUTER_BOUND ( 'NONE', #10262, .T. ) ;
#4063 = CARTESIAN_POINT ( 'NONE',  ( 7.879643458700000380, -36.30219044630000269, -21.38844997820000060 ) ) ;
#4064 = CARTESIAN_POINT ( 'NONE',  ( -0.7914099002037787711, -92.53260370683119618, -30.48976482468907534 ) ) ;
#4065 = ADVANCED_FACE ( 'NONE', ( #10873, #19783 ), #17613, .T. ) ;
#4066 = VECTOR ( 'NONE', #9857, 1000.000000000000000 ) ;
#4067 = CARTESIAN_POINT ( 'NONE',  ( -11.91266501540000000, -79.50000000000000000, 46.64429291560000479 ) ) ;
#4068 = CARTESIAN_POINT ( 'NONE',  ( -11.29408752129999982, -94.76700071680001258, -21.12307072750000358 ) ) ;
#4069 = EDGE_CURVE ( 'NONE', #4763, #22615, #13226, .T. ) ;
#4070 = ORIENTED_EDGE ( 'NONE', *, *, #15260, .T. ) ;
#4071 = CARTESIAN_POINT ( 'NONE',  ( -27.18988201479999844, -14.89844555430000028, -49.77074518290000071 ) ) ;
#4072 = CARTESIAN_POINT ( 'NONE',  ( 24.41687773985064780, -18.97801304285953350, 1.565715090140727517 ) ) ;
#4073 = ORIENTED_EDGE ( 'NONE', *, *, #13996, .F. ) ;
#4074 = AXIS2_PLACEMENT_3D ( 'NONE', #17331, #24027, #6251 ) ;
#4075 = CARTESIAN_POINT ( 'NONE',  ( 20.95125717089999995, -36.09768395309999534, -8.611231333170000113 ) ) ;
#4076 = CARTESIAN_POINT ( 'NONE',  ( -43.12299426110000411, -65.19264941160000149, -0.2176643648609999926 ) ) ;
#4077 = ORIENTED_EDGE ( 'NONE', *, *, #22960, .F. ) ;
#4078 = CARTESIAN_POINT ( 'NONE',  ( -12.81629053550000030, -101.0555477039999914, -8.711806805760000216 ) ) ;
#4079 = PRODUCT_DEFINITION_SHAPE ( 'NONE', 'NONE',  #26287 ) ;
#4080 = CARTESIAN_POINT ( 'NONE',  ( -3.356616257537091474, -68.05312507927790477, -27.55666181306940032 ) ) ;
#4081 = CARTESIAN_POINT ( 'NONE',  ( -0.5590517731190000061, -18.50000000000000000, -21.02688049580000040 ) ) ;
#4082 = CARTESIAN_POINT ( 'NONE',  ( 1.741343278310000020, -92.68419354089999729, 27.53437997139999993 ) ) ;
#4083 = CARTESIAN_POINT ( 'NONE',  ( -30.40264043347529466, -92.82668962668607548, 2.435048001739037904 ) ) ;
#4084 = DIRECTION ( 'NONE',  ( -0.9952295494196657932, 0.000000000000000000, 0.09756097560976527416 ) ) ;
#4085 = CARTESIAN_POINT ( 'NONE',  ( -10.44618222529999940, -18.50000000000000000, -18.70089465730000100 ) ) ;
#4086 = CARTESIAN_POINT ( 'NONE',  ( -39.95292656566140721, -65.74401284883323626, 2.175430544872245964 ) ) ;
#4087 = ORIENTED_EDGE ( 'NONE', *, *, #24723, .F. ) ;
#4088 = AXIS2_PLACEMENT_3D ( 'NONE', #2177, #4497, #11015 ) ;
#4089 = DIRECTION ( 'NONE',  ( 1.000000000000000000, 0.000000000000000000, 0.000000000000000000 ) ) ;
#4090 = CARTESIAN_POINT ( 'NONE',  ( 22.02876637549999828, -19.46348310600000175, -0.4636467615609999871 ) ) ;
#4091 = CARTESIAN_POINT ( 'NONE',  ( 23.20278881559999817, -65.91612967349999508, 11.11676163019999919 ) ) ;
#4092 = CARTESIAN_POINT ( 'NONE',  ( 9.370945274540000369, -94.71481430550001335, -22.48432346729999765 ) ) ;
#4093 = VERTEX_POINT ( 'NONE', #2321 ) ;
#4094 = CIRCLE ( 'NONE', #18065, 28.68388914670000034 ) ;
#4095 = CARTESIAN_POINT ( 'NONE',  ( 4.882943008269999509E-15, -73.00000000000000000, -40.00000000000000000 ) ) ;
#4096 = CARTESIAN_POINT ( 'NONE',  ( -14.80857177290000060, -92.53271748610001168, 24.80080696000000273 ) ) ;
#4097 = CARTESIAN_POINT ( 'NONE',  ( -20.54120388167250510, -92.96187023300437602, 17.39114321432820987 ) ) ;
#4098 = ORIENTED_EDGE ( 'NONE', *, *, #24752, .T. ) ;
#4099 = CARTESIAN_POINT ( 'NONE',  ( 36.82697894980000086, -80.49999984420000487, -13.57704391360000074 ) ) ;
#4100 =( GEOMETRIC_REPRESENTATION_CONTEXT ( 3 ) GLOBAL_UNCERTAINTY_ASSIGNED_CONTEXT ( ( #25217 ) ) GLOBAL_UNIT_ASSIGNED_CONTEXT ( ( #7186, #2669, #27289 ) ) REPRESENTATION_CONTEXT ( 'NONE', 'WORKASPACE' ) );
#4101 = CARTESIAN_POINT ( 'NONE',  ( 0.5427213986669999768, -100.0482783049999966, -17.18673518379999621 ) ) ;
#4102 = CARTESIAN_POINT ( 'NONE',  ( 7.268665519299999822, -62.14086513569999681, -22.85591912949999838 ) ) ;
#4103 = CARTESIAN_POINT ( 'NONE',  ( 15.50047883180000063, -101.1716782080000030, 2.701940809000000332 ) ) ;
#4104 = CARTESIAN_POINT ( 'NONE',  ( 22.86993016659999967, -57.41946943429999806, 10.24154007049999926 ) ) ;
#4105 = CARTESIAN_POINT ( 'NONE',  ( 24.16120406939999654, -64.60178126830000167, -9.605465959289999134 ) ) ;
#4106 = VERTEX_POINT ( 'NONE', #11173 ) ;
#4107 = EDGE_CURVE ( 'NONE', #27931, #54, #10133, .T. ) ;
#4108 = CARTESIAN_POINT ( 'NONE',  ( 6.185491179879999635, -101.0875971110000080, 14.11315596670000083 ) ) ;
#4109 = CARTESIAN_POINT ( 'NONE',  ( 14.81927149150000034, -101.2530993010000060, 3.356308434120000239 ) ) ;
#4110 = CARTESIAN_POINT ( 'NONE',  ( -4.986610887291577754, -96.57210917192522004, 21.09623979869162724 ) ) ;
#4111 = CIRCLE ( 'NONE', #24122, 21.03431122519999974 ) ;
#4112 = ORIENTED_EDGE ( 'NONE', *, *, #19158, .F. ) ;
#4113 = CARTESIAN_POINT ( 'NONE',  ( 21.02495559440000150, -29.55373279730000391, -7.687066009020000479 ) ) ;
#4114 = CARTESIAN_POINT ( 'NONE',  ( 23.90010427143523941, -63.16487826049581145, 10.68054471888447843 ) ) ;
#4115 = CARTESIAN_POINT ( 'NONE',  ( 25.26718046270000073, -74.00000000000000000, 6.129403842640000377 ) ) ;
#4116 = CARTESIAN_POINT ( 'NONE',  ( 4.420730772149999765, -92.67327634539999792, -27.51018170170000232 ) ) ;
#4117 = CARTESIAN_POINT ( 'NONE',  ( 6.741848109771249931, -101.4304678898295293, 14.69584814897645586 ) ) ;
#4118 = DIRECTION ( 'NONE',  ( 1.000000000000000000, 0.000000000000000000, 0.000000000000000000 ) ) ;
#4119 = ORIENTED_EDGE ( 'NONE', *, *, #13410, .F. ) ;
#4120 = DIRECTION ( 'NONE',  ( 0.4794255386042040601, 0.000000000000000000, 0.8775825618903722036 ) ) ;
#4121 = CARTESIAN_POINT ( 'NONE',  ( -13.05879515434285132, -100.1994045928751120, -11.10531386412310262 ) ) ;
#4122 = VERTEX_POINT ( 'NONE', #13966 ) ;
#4123 = CARTESIAN_POINT ( 'NONE',  ( 9.028475982079999795, -35.72979163269999958, -19.84586683699999909 ) ) ;
#4124 = FACE_OUTER_BOUND ( 'NONE', #7426, .T. ) ;
#4125 = CARTESIAN_POINT ( 'NONE',  ( -0.9221465140669999894, -101.1499348409999897, -15.72402173499999911 ) ) ;
#4126 = ADVANCED_FACE ( 'NONE', ( #9003 ), #12840, .T. ) ;
#4127 = CARTESIAN_POINT ( 'NONE',  ( 22.01810471299999961, -19.15810975349999978, -0.4634309158250000116 ) ) ;
#4128 = CARTESIAN_POINT ( 'NONE',  ( -43.29047163944868259, -63.05597747387585628, 0.07115400839859020721 ) ) ;
#4129 = AXIS2_PLACEMENT_3D ( 'NONE', #13062, #4483, #6676 ) ;
#4130 = CARTESIAN_POINT ( 'NONE',  ( 23.56559805210000036, -58.81638232979999970, -9.577937461890000392 ) ) ;
#4131 = ORIENTED_EDGE ( 'NONE', *, *, #10950, .T. ) ;
#4132 = CARTESIAN_POINT ( 'NONE',  ( -15.39276618189999901, -101.4254873440000040, 4.250919977269999706 ) ) ;
#4133 = DIRECTION ( 'NONE',  ( 0.000000000000000000, 1.000000000000000000, 0.000000000000000000 ) ) ;
#4134 = AXIS2_PLACEMENT_3D ( 'NONE', #8089, #14907, #5894 ) ;
#4135 = DIRECTION ( 'NONE',  ( 0.000000000000000000, 1.000000000000000000, 0.000000000000000000 ) ) ;
#4136 = AXIS2_PLACEMENT_3D ( 'NONE', #3949, #1503, #6414 ) ;
#4137 = CIRCLE ( 'NONE', #25110, 24.40223267850000255 ) ;
#4138 = CARTESIAN_POINT ( 'NONE',  ( -18.48666763681400838, -19.46756325244718155, 12.61459962061059059 ) ) ;
#4139 = DIRECTION ( 'NONE',  ( 1.000000000000000000, 0.000000000000000000, 0.000000000000000000 ) ) ;
#4140 = CARTESIAN_POINT ( 'NONE',  ( 24.65020093668425005, -93.55106866415557931, -11.39260662483369124 ) ) ;
#4141 = CARTESIAN_POINT ( 'NONE',  ( 19.98296175649999995, -94.98812477599999227, 14.17692170039999944 ) ) ;
#4142 = ORIENTED_EDGE ( 'NONE', *, *, #3932, .T. ) ;
#4143 = CARTESIAN_POINT ( 'NONE',  ( 7.593154301330000244, -18.50000000000000000, -19.61724635699999908 ) ) ;
#4144 = CARTESIAN_POINT ( 'NONE',  ( 22.68565687650000129, -36.18510625669999570, -10.42651188819999852 ) ) ;
#4145 = CARTESIAN_POINT ( 'NONE',  ( -0.8491947589009999353, -58.35623000289999851, -23.39045838330000038 ) ) ;
#4146 = CIRCLE ( 'NONE', #24159, 34.89999999999999858 ) ;
#4147 = CARTESIAN_POINT ( 'NONE',  ( 10.65875326940000001, -36.00000000000000000, -21.02691194339999825 ) ) ;
#4148 = CARTESIAN_POINT ( 'NONE',  ( -24.98485751299999791, -93.92589062430000979, -2.982315457539999937 ) ) ;
#4149 = DIRECTION ( 'NONE',  ( 1.000000000000000000, 0.000000000000000000, 0.000000000000000000 ) ) ;
#4150 = FACE_OUTER_BOUND ( 'NONE', #7759, .T. ) ;
#4151 = CIRCLE ( 'NONE', #12978, 6.750000000000000000 ) ;
#4152 = AXIS2_PLACEMENT_3D ( 'NONE', #21003, #5267, #9765 ) ;
#4153 = EDGE_LOOP ( 'NONE', ( #19680, #18918, #5533, #22054 ) ) ;
#4154 = CARTESIAN_POINT ( 'NONE',  ( 21.41502072009999935, -35.30712908469999434, -7.187003606720000271 ) ) ;
#4155 = CARTESIAN_POINT ( 'NONE',  ( -36.90000000000000568, -65.00000000000000000, 2.131628207279999844E-14 ) ) ;
#4156 = ORIENTED_EDGE ( 'NONE', *, *, #5146, .F. ) ;
#4157 = DIRECTION ( 'NONE',  ( 0.8775825618903719816, 0.000000000000000000, 0.4794255386042042821 ) ) ;
#4158 = CARTESIAN_POINT ( 'NONE',  ( -14.28268380569999962, -79.99937754569999981, 36.92904800159999468 ) ) ;
#4159 = EDGE_CURVE ( 'NONE', #11754, #26673, #7275, .T. ) ;
#4160 = CARTESIAN_POINT ( 'NONE',  ( -9.435680430750000625, -18.50000000000000000, -20.63248585200000207 ) ) ;
#4161 = DIRECTION ( 'NONE',  ( 0.000000000000000000, 1.000000000000000000, 0.000000000000000000 ) ) ;
#4162 = EDGE_CURVE ( 'NONE', #5957, #12729, #26421, .T. ) ;
#4163 = CARTESIAN_POINT ( 'NONE',  ( -26.69328098980000163, -74.00000000000000000, -35.88566914520000495 ) ) ;
#4164 = CARTESIAN_POINT ( 'NONE',  ( 10.08507888390000140, -64.24505061060000344, -24.78972398320000181 ) ) ;
#4165 = CARTESIAN_POINT ( 'NONE',  ( -13.15133833870000046, -100.9197081840000010, -8.436152112259998503 ) ) ;
#4166 = ORIENTED_EDGE ( 'NONE', *, *, #9964, .T. ) ;
#4167 = CYLINDRICAL_SURFACE ( 'NONE', #7406, 3.749999999999996447 ) ;
#4168 = CARTESIAN_POINT ( 'NONE',  ( -12.01303215110000089, -101.1284992150000051, -9.644678736739999536 ) ) ;
#4169 = EDGE_CURVE ( 'NONE', #26586, #28649, #17404, .T. ) ;
#4170 = CARTESIAN_POINT ( 'NONE',  ( 25.49913305207284253, -93.00000166546709579, 13.79230533256381186 ) ) ;
#4171 = CARTESIAN_POINT ( 'NONE',  ( -7.293834223439488618, -101.4241070620022640, 14.43537265006951742 ) ) ;
#4172 = ORIENTED_EDGE ( 'NONE', *, *, #24675, .F. ) ;
#4173 = EDGE_CURVE ( 'NONE', #6867, #9479, #13896, .T. ) ;
#4174 = AXIS2_PLACEMENT_3D ( 'NONE', #4222, #8719, #3939 ) ;
#4175 = B_SPLINE_CURVE_WITH_KNOTS ( 'NONE', 5,
 ( #5384, #12581, #23819, #8358, #6328, #23022, #3073, #11927, #892, #18649, #21354, #1411, #7587, #16450, #14267, #15638, #24693, #26584 ),
 .UNSPECIFIED., .F., .F.,
 ( 6, 3, 3, 3, 3, 6 ),
 ( 0.000000000000000000, 1.123597580079999991, 2.251105601749999963, 3.378920662530000563, 4.507088924770000560, 5.576980223840000583 ),
 .UNSPECIFIED. ) ;
#4176 = CARTESIAN_POINT ( 'NONE',  ( -1.207226396496814180, -101.4218099523420449, -16.12573525851230372 ) ) ;
#4177 = CARTESIAN_POINT ( 'NONE',  ( -32.08921965649999919, -74.00994675159999758, -21.99574735890000099 ) ) ;
#4178 = ORIENTED_EDGE ( 'NONE', *, *, #12355, .T. ) ;
#4179 = B_SPLINE_CURVE_WITH_KNOTS ( 'NONE', 5,
 ( #10758, #4382, #19670, #2063, #28689, #28558 ),
 .UNSPECIFIED., .F., .F.,
 ( 6, 6 ),
 ( 0.000000000000000000, 1.000000000000000000 ),
 .UNSPECIFIED. ) ;
#4180 = DIRECTION ( 'NONE',  ( -1.000000000000000000, 0.000000000000000000, 0.000000000000000000 ) ) ;
#4181 = CARTESIAN_POINT ( 'NONE',  ( 24.92937355771860197, -41.21911678059012729, 1.391361396670305339 ) ) ;
#4182 = CARTESIAN_POINT ( 'NONE',  ( -22.43272077086249183, -80.34292036766261447, -32.20769378288610341 ) ) ;
#4183 = ORIENTED_EDGE ( 'NONE', *, *, #20242, .T. ) ;
#4184 = CARTESIAN_POINT ( 'NONE',  ( -18.95261912118637682, -97.48771974254098893, 6.567162275491772228 ) ) ;
#4185 = ORIENTED_EDGE ( 'NONE', *, *, #3910, .T. ) ;
#4186 = CARTESIAN_POINT ( 'NONE',  ( 25.89192503760000008, -92.65715432180000732, 10.49931292039999953 ) ) ;
#4187 = DIRECTION ( 'NONE',  ( 0.000000000000000000, 1.000000000000000000, 0.000000000000000000 ) ) ;
#4188 = ORIENTED_EDGE ( 'NONE', *, *, #14258, .T. ) ;
#4189 = AXIS2_PLACEMENT_3D ( 'NONE', #19021, #12432, #23257 ) ;
#4190 = CARTESIAN_POINT ( 'NONE',  ( 21.64387303326116196, -18.61794787929532546, -0.4555539749991904808 ) ) ;
#4191 = CARTESIAN_POINT ( 'NONE',  ( -22.87716665625361045, -94.65677004888377155, -7.699218993550634771 ) ) ;
#4192 = CIRCLE ( 'NONE', #4685, 3.000000000000002665 ) ;
#4193 = TOROIDAL_SURFACE ( 'NONE', #7504, 38.75000000000000000, 0.5000000000000000000 ) ;
#4194 = CARTESIAN_POINT ( 'NONE',  ( 9.377113207090001623, -36.00000000019999646, -20.73064381829999903 ) ) ;
#4195 = CARTESIAN_POINT ( 'NONE',  ( -21.87838817989999995, -92.50732182800000203, -19.74814203740000096 ) ) ;
#4196 = CARTESIAN_POINT ( 'NONE',  ( -1.156789036890000011, -18.50000000000000000, -21.06078022829999696 ) ) ;
#4197 = EDGE_LOOP ( 'NONE', ( #7874, #15535, #5355, #12327 ) ) ;
#4198 = EDGE_CURVE ( 'NONE', #27292, #23692, #10055, .T. ) ;
#4199 = DIRECTION ( 'NONE',  ( 0.4794255386042040601, 0.000000000000000000, 0.8775825618903720926 ) ) ;
#4200 = CARTESIAN_POINT ( 'NONE',  ( 13.83027782289999941, -99.92384627689999377, -9.732040768319999202 ) ) ;
#4201 = CARTESIAN_POINT ( 'NONE',  ( -2.664535259099999805E-15, -72.82938648530000592, -3.552713678799999608E-15 ) ) ;
#4202 = CARTESIAN_POINT ( 'NONE',  ( -5.405932493604948874, -98.40858131475137327, -19.29511042873029680 ) ) ;
#4203 = DIRECTION ( 'NONE',  ( -1.000000000000000000, 0.000000000000000000, -3.081450948259999971E-16 ) ) ;
#4204 = ADVANCED_FACE ( 'NONE', ( #25203 ), #8910, .F. ) ;
#4205 = CARTESIAN_POINT ( 'NONE',  ( 10.04439987701514880, -72.76369477738892044, -26.87308552718831933 ) ) ;
#4206 = LINE ( 'NONE', #21989, #8901 ) ;
#4207 = ORIENTED_EDGE ( 'NONE', *, *, #17771, .T. ) ;
#4208 = EDGE_CURVE ( 'NONE', #2510, #7623, #1084, .T. ) ;
#4209 = FACE_OUTER_BOUND ( 'NONE', #6195, .T. ) ;
#4210 = FACE_OUTER_BOUND ( 'NONE', #24404, .T. ) ;
#4211 = DIRECTION ( 'NONE',  ( 0.000000000000000000, 1.000000000000000000, 0.000000000000000000 ) ) ;
#4212 = CARTESIAN_POINT ( 'NONE',  ( -38.58844719860000083, -65.17124718639999514, 2.835686332019999867 ) ) ;
#4213 = TOROIDAL_SURFACE ( 'NONE', #5625, 9.000000000000000000, 1.000000000000000000 ) ;
#4214 = AXIS2_PLACEMENT_3D ( 'NONE', #280, #6963, #15973 ) ;
#4215 = DIRECTION ( 'NONE',  ( 0.000000000000000000, 0.000000000000000000, 1.000000000000000000 ) ) ;
#4216 = CARTESIAN_POINT ( 'NONE',  ( -10.13149966729999818, -18.50000000000000000, 18.43352823549999897 ) ) ;
#4217 = ORIENTED_EDGE ( 'NONE', *, *, #4407, .T. ) ;
#4218 = CARTESIAN_POINT ( 'NONE',  ( 19.28934113089999869, -98.24904978849998827, -0.4858748118589999443 ) ) ;
#4220 = ORIENTED_EDGE ( 'NONE', *, *, #26245, .F. ) ;
#4219 = B_SPLINE_CURVE_WITH_KNOTS ( 'NONE', 3,
 ( #26883, #24695, #24983, #4731, #13609, #22517, #1770, #13401, #13107, #6124, #14997, #26095, #19960, #2067, #4232, #10614, #22162, #22019, #8730, #20116, #2202, #6272, #8451, #15278, #19673, #2352, #10905, #24200, #19813, #26529, #19530, #11044, #28692 ),
 .UNSPECIFIED., .F., .F.,
 ( 4, 2, 1, 1, 2, 2, 1, 1, 1, 2, 2, 2, 1, 1, 2, 2, 1, 1, 2, 2, 4 ),
 ( 0.000000000000000000, 0.06249999999994848565, 0.09374999999993488542, 0.1093749999999379940, 0.1171874999999479444, 0.1249999999999578948, 0.1874999999999998335, 0.2187500000000123235, 0.2343750000000191513, 0.2421875000000219269, 0.2500000000000247025, 0.3750000000000558997, 0.4375000000000673905, 0.4687500000000705547, 0.4843750000000699441, 0.5000000000000693889, 0.6250000000000489608, 0.6875000000000387468, 0.7187500000000344169, 0.7500000000000300870, 1.000000000000000000 ),
 .UNSPECIFIED. ) ;
#4221 = CARTESIAN_POINT ( 'NONE',  ( 28.63360765790000073, -72.82938648530000592, 1.697648101029999967 ) ) ;
#4222 = CARTESIAN_POINT ( 'NONE',  ( -41.00000000000000000, -82.25000000000000000, -10.20110288159999890 ) ) ;
#4223 = ORIENTED_EDGE ( 'NONE', *, *, #626, .F. ) ;
#4224 = DIRECTION ( 'NONE',  ( 1.000000000000000000, 0.000000000000000000, 0.000000000000000000 ) ) ;
#4225 = CARTESIAN_POINT ( 'NONE',  ( -13.10651977150000036, -92.87496808400000248, -23.83817077610000368 ) ) ;
#4226 = LINE ( 'NONE', #19525, #8440 ) ;
#4227 = ORIENTED_EDGE ( 'NONE', *, *, #18836, .F. ) ;
#4228 = CARTESIAN_POINT ( 'NONE',  ( -8.882254428079999542, -95.94151723290001144, -20.27227240450000068 ) ) ;
#4229 = EDGE_CURVE ( 'NONE', #16936, #26524, #5025, .T. ) ;
#4230 = CARTESIAN_POINT ( 'NONE',  ( 1.631276547419999945, -94.59276292389999696, 23.74086995720000104 ) ) ;
#4231 = CARTESIAN_POINT ( 'NONE',  ( -20.27480750739999849, -94.70871900059999859, 12.26045949169999894 ) ) ;
#4232 = CARTESIAN_POINT ( 'NONE',  ( -29.70690187338877308, -92.71619979444709259, 6.910137393209939027 ) ) ;
#4233 = AXIS2_PLACEMENT_3D ( 'NONE', #5450, #14333, #3275 ) ;
#4234 = CARTESIAN_POINT ( 'NONE',  ( 12.00265656396589975, -100.1470170749897619, -13.12398194341028024 ) ) ;
#4235 = EDGE_LOOP ( 'NONE', ( #13213, #23112, #4649, #7 ) ) ;
#4236 = VECTOR ( 'NONE', #21129, 1000.000000000000000 ) ;
#4237 = EDGE_CURVE ( 'NONE', #1488, #1054, #3479, .T. ) ;
#4238 = CARTESIAN_POINT ( 'NONE',  ( 4.500000000000000000, -11.00000000000000000, -40.50000000000000000 ) ) ;
#4239 = AXIS2_PLACEMENT_3D ( 'NONE', #2565, #11414, #20315 ) ;
#4240 = CARTESIAN_POINT ( 'NONE',  ( 22.64221431050000177, -34.66889731630000426, 0.1161384314939999940 ) ) ;
#4241 = CARTESIAN_POINT ( 'NONE',  ( 24.22381685739999924, -64.24504218810000111, 10.76340169160000038 ) ) ;
#4242 = FACE_OUTER_BOUND ( 'NONE', #6855, .T. ) ;
#4243 = ORIENTED_EDGE ( 'NONE', *, *, #11672, .F. ) ;
#4244 = CARTESIAN_POINT ( 'NONE',  ( -2.605870139415221942, -64.47176446041650877, -25.91539817187144834 ) ) ;
#4245 = CARTESIAN_POINT ( 'NONE',  ( -18.00579138470000018, -93.94806047000001570, 18.35448323720000019 ) ) ;
#4246 = FACE_OUTER_BOUND ( 'NONE', #4153, .T. ) ;
#4247 = ORIENTED_EDGE ( 'NONE', *, *, #11163, .T. ) ;
#4248 = ADVANCED_FACE ( 'NONE', ( #1855 ), #24276, .T. ) ;
#4249 = DIRECTION ( 'NONE',  ( 0.4794255386042000078, 0.000000000000000000, 0.8775825618903743131 ) ) ;
#4250 = CARTESIAN_POINT ( 'NONE',  ( 0.7792231278100000269, -100.9137139110000021, -15.61347424839999931 ) ) ;
#4251 = CARTESIAN_POINT ( 'NONE',  ( 7.675802467109999583, -57.47600031380000729, -22.13628273389999990 ) ) ;
#4252 = CARTESIAN_POINT ( 'NONE',  ( 14.98792925300000078, -101.2530993039999885, 2.502342737139999773 ) ) ;
#4253 = CARTESIAN_POINT ( 'NONE',  ( 21.17771081649999942, -61.87790347820000392, 11.21104585369999995 ) ) ;
#4254 = CARTESIAN_POINT ( 'NONE',  ( 22.88682908910000435, -61.98361058570000637, -8.756040560759998925 ) ) ;
#4255 = ORIENTED_EDGE ( 'NONE', *, *, #4752, .T. ) ;
#4256 = FACE_OUTER_BOUND ( 'NONE', #21115, .T. ) ;
#4257 = TOROIDAL_SURFACE ( 'NONE', #6596, 60.85000000000000142, 0.5000000000000000000 ) ;
#4258 = CIRCLE ( 'NONE', #24270, 0.9999999999999980016 ) ;
#4259 = ORIENTED_EDGE ( 'NONE', *, *, #2346, .F. ) ;
#4260 = DIRECTION ( 'NONE',  ( 0.4794255386042040046, 0.000000000000000000, 0.8775825618903722036 ) ) ;
#4261 = CARTESIAN_POINT ( 'NONE',  ( -15.50938051129999984, -111.0000000000000000, 4.855933523060000034 ) ) ;
#4262 = CARTESIAN_POINT ( 'NONE',  ( -41.93357002089393859, -65.74109373451008764, -1.008753740007117816 ) ) ;
#4263 = ORIENTED_EDGE ( 'NONE', *, *, #4749, .F. ) ;
#4264 = CARTESIAN_POINT ( 'NONE',  ( 8.831064156680000110, -94.59276292120000562, -22.09756269280000041 ) ) ;
#4265 = CARTESIAN_POINT ( 'NONE',  ( 20.70967183530000000, -25.50459736320000204, -8.132923256100001552 ) ) ;
#4266 = LINE ( 'NONE', #10794, #7920 ) ;
#4267 = CARTESIAN_POINT ( 'NONE',  ( -6.805335268389999470, -101.3256027139999986, 14.37758720309999916 ) ) ;
#4268 = VERTEX_POINT ( 'NONE', #19189 ) ;
#4269 = CARTESIAN_POINT ( 'NONE',  ( 47.16974535660000356, -74.50000000000000000, -1.075756255579999987 ) ) ;
#4270 = CARTESIAN_POINT ( 'NONE',  ( -13.29096466015767852, -99.96200787834916923, -11.12774058592850679 ) ) ;
#4271 = VERTEX_POINT ( 'NONE', #17004 ) ;
#4272 = DIRECTION ( 'NONE',  ( 1.000000000000000000, 0.000000000000000000, 0.000000000000000000 ) ) ;
#4273 = DIRECTION ( 'NONE',  ( 0.000000000000000000, -1.000000000000000000, 0.000000000000000000 ) ) ;
#4274 = VERTEX_POINT ( 'NONE', #10696 ) ;
#4275 = EDGE_CURVE ( 'NONE', #22021, #12657, #9696, .T. ) ;
#4276 = CARTESIAN_POINT ( 'NONE',  ( -1.125884257989999915, -101.0535396030000044, -15.55188116729999770 ) ) ;
#4277 = CARTESIAN_POINT ( 'NONE',  ( 21.02965312769999784, -18.50000000000000000, -0.4426264348499999723 ) ) ;
#4278 = DIRECTION ( 'NONE',  ( 0.000000000000000000, 1.000000000000000000, 0.000000000000000000 ) ) ;
#4279 = CARTESIAN_POINT ( 'NONE',  ( -21.30003612899999865, -93.00000000000000000, -21.83021898440000186 ) ) ;
#4280 = ORIENTED_EDGE ( 'NONE', *, *, #5356, .F. ) ;
#4281 = EDGE_CURVE ( 'NONE', #15723, #7597, #19107, .T. ) ;
#4282 = CARTESIAN_POINT ( 'NONE',  ( -14.67001285520000131, -101.1516882750000121, 4.438127419890000702 ) ) ;
#4283 = CIRCLE ( 'NONE', #20585, 0.7500000000000006661 ) ;
#4284 = CARTESIAN_POINT ( 'NONE',  ( -13.32502991189999797, -19.49268876740000067, 20.00853956230000108 ) ) ;
#4285 = CARTESIAN_POINT ( 'NONE',  ( 16.36049596713812093, -94.62565524723831345, 17.22219307773070440 ) ) ;
#4286 = CARTESIAN_POINT ( 'NONE',  ( -43.75000000000000000, -69.00000000000000000, 0.000000000000000000 ) ) ;
#4287 = B_SPLINE_CURVE_WITH_KNOTS ( 'NONE', 3,
 ( #11490, #3491, #16602, #16464, #27259, #5528 ),
 .UNSPECIFIED., .F., .F.,
 ( 4, 2, 4 ),
 ( 0.000000000000000000, 0.5000000000000000000, 1.000000000000000000 ),
 .UNSPECIFIED. ) ;
#4288 = FACE_OUTER_BOUND ( 'NONE', #28698, .T. ) ;
#4289 = DIRECTION ( 'NONE',  ( 0.4794255386042040046, 0.000000000000000000, 0.8775825618903722036 ) ) ;
#4290 = DIRECTION ( 'NONE',  ( 0.000000000000000000, -1.000000000000000000, 0.000000000000000000 ) ) ;
#4291 = CARTESIAN_POINT ( 'NONE',  ( 24.64984454473747277, -93.08996811592339782, -15.39677593028482505 ) ) ;
#4292 = CARTESIAN_POINT ( 'NONE',  ( 27.15071147507873306, -93.11247489698153856, 9.921984135710960828 ) ) ;
#4293 = VERTEX_POINT ( 'NONE', #1438 ) ;
#4294 = CARTESIAN_POINT ( 'NONE',  ( -10.93437413680000070, -19.50000027030000282, -21.85842452360000010 ) ) ;
#4295 = CARTESIAN_POINT ( 'NONE',  ( 22.23224290750000165, -37.35114138160000152, -9.119208908199999186 ) ) ;
#4296 = ORIENTED_EDGE ( 'NONE', *, *, #24688, .F. ) ;
#4297 = ADVANCED_BREP_SHAPE_REPRESENTATION ( '', ( #15722, #26433 ), #911 ) ;
#4298 = EDGE_CURVE ( 'NONE', #19516, #9243, #8290, .T. ) ;
#4299 = CARTESIAN_POINT ( 'NONE',  ( -11.86778496400000016, -60.57945642420000354, 20.49707039420000143 ) ) ;
#4300 = CARTESIAN_POINT ( 'NONE',  ( -25.76715338260000010, -94.09272382160000348, -2.407609377890000069 ) ) ;
#4301 = VECTOR ( 'NONE', #18518, 1000.000000000000114 ) ;
#4302 = CARTESIAN_POINT ( 'NONE',  ( -19.99335094079999919, -53.79621871020000157, 14.42235124120000123 ) ) ;
#4303 = CARTESIAN_POINT ( 'NONE',  ( 19.95150103176392520, -19.47987602260658235, -8.638154654088172180 ) ) ;
#4304 = CARTESIAN_POINT ( 'NONE',  ( 16.25788162539999959, -100.4650220110000021, 4.370703170420000561 ) ) ;
#4305 = ORIENTED_EDGE ( 'NONE', *, *, #11011, .F. ) ;
#4306 = DIRECTION ( 'NONE',  ( -0.000000000000000000, 1.000000000000000000, 0.000000000000000000 ) ) ;
#4307 = DIRECTION ( 'NONE',  ( 0.000000000000000000, 1.000000000000000000, 0.000000000000000000 ) ) ;
#4308 = ORIENTED_EDGE ( 'NONE', *, *, #11306, .F. ) ;
#4309 = DIRECTION ( 'NONE',  ( 1.000000000000000000, 0.000000000000000000, 0.000000000000000000 ) ) ;
#4310 = ADVANCED_FACE ( 'NONE', ( #20339 ), #16825, .T. ) ;
#4311 = CARTESIAN_POINT ( 'NONE',  ( -10.89815191770000169, -18.50000000000000000, -17.99090140869999743 ) ) ;
#4312 = CYLINDRICAL_SURFACE ( 'NONE', #15781, 9.500000000000001776 ) ;
#4313 = CARTESIAN_POINT ( 'NONE',  ( -13.82310862910000004, -74.00000000000000000, 36.20061004779999791 ) ) ;
#4314 = CARTESIAN_POINT ( 'NONE',  ( 11.00114453930000025, -68.91000853889998723, -26.38226308069999959 ) ) ;
#4315 = CARTESIAN_POINT ( 'NONE',  ( -40.33877555573290863, -63.33820092556621972, 2.216318100457958629 ) ) ;
#4316 = VERTEX_POINT ( 'NONE', #9561 ) ;
#4317 = EDGE_CURVE ( 'NONE', #4037, #24255, #15946, .T. ) ;
#4318 = AXIS2_PLACEMENT_3D ( 'NONE', #11199, #24633, #4668 ) ;
#4319 = B_SPLINE_CURVE_WITH_KNOTS ( 'NONE', 3,
 ( #16301, #13975, #3208, #18652, #25358, #25211, #22880, #20837, #18359, #2921, #20538, #16153, #9304, #27393, #27546, #11784, #23165, #895, #7590, #16010, #5093, #610, #13683, #11628, #16455, #11480, #20386, #24915, #5244, #9600, #5388, #6998, #9882, #9453, #15861, #460, #14270, #14128, #18797, #27247, #12069, #13827, #22732, #23026, #3077, #1045, #2633, #20980, #24771, #22590, #4807, #20695, #18207, #755, #27105, #7144, #4946, #2773, #25059 ),
 .UNSPECIFIED., .F., .F.,
 ( 4, 2, 1, 1, 2, 2, 2, 2, 1, 1, 2, 2, 2, 2, 2, 2, 2, 1, 1, 2, 2, 2, 1, 1, 2, 2, 2, 1, 2, 2, 2, 2, 2, 4 ),
 ( 0.000000000000000000, 0.06249999999986541321, 0.09374999999980372645, 0.1093749999997741945, 0.1171874999997657707, 0.1249999999997573330, 0.1874999999997541689, 0.2187499999997595257, 0.2343749999997633837, 0.2421874999997600253, 0.2460937499997583322, 0.2499999999997566391, 0.3124999999997333799, 0.3437499999997205569, 0.3749999999997077338, 0.4374999999996713185, 0.4687499999996531108, 0.4843749999996440070, 0.4921874999996383448, 0.4960937499996446731, 0.4999999999996509459, 0.5624999999997148947, 0.5937499999997458699, 0.6093749999997675193, 0.6171874999997792877, 0.6249999999997910560, 0.6874999999998409050, 0.7187499999998658851, 0.7343749999998772093, 0.7499999999998882005, 0.8124999999999155120, 0.8437499999999296119, 0.8749999999999436007, 1.000000000000000000 ),
 .UNSPECIFIED. ) ;
#4320 = CARTESIAN_POINT ( 'NONE',  ( -13.44405788329999929, -68.28990366489999531, 22.97003105929999833 ) ) ;
#4321 = DIRECTION ( 'NONE',  ( 0.000000000000000000, 1.000000000000000000, 0.000000000000000000 ) ) ;
#4322 = CARTESIAN_POINT ( 'NONE',  ( -11.72126804459999860, -100.9137139110000021, -10.34406313869999927 ) ) ;
#4323 = CARTESIAN_POINT ( 'NONE',  ( -22.62625778519381825, -72.15620726826487896, 17.99661011978010805 ) ) ;
#4324 = CARTESIAN_POINT ( 'NONE',  ( -13.14566783280000095, -99.53431386179998697, -11.42099844400000030 ) ) ;
#4325 = ORIENTED_EDGE ( 'NONE', *, *, #10370, .T. ) ;
#4326 = B_SPLINE_CURVE_WITH_KNOTS ( 'NONE', 5,
 ( #13868, #2812, #22321, #346, #24504, #26848, #794, #4541, #496 ),
 .UNSPECIFIED., .F., .F.,
 ( 6, 3, 6 ),
 ( 0.000000000000000000, 0.5000000000000000000, 1.000000000000000000 ),
 .UNSPECIFIED. ) ;
#4327 = CARTESIAN_POINT ( 'NONE',  ( 0.000000000000000000, -23.00000000000000000, 0.000000000000000000 ) ) ;
#4328 = CARTESIAN_POINT ( 'NONE',  ( -32.46073318370000038, -74.16345073059999038, -21.90351770710000068 ) ) ;
#4329 = CARTESIAN_POINT ( 'NONE',  ( -22.52722182890634528, -79.95932862086812065, -32.70629964928058087 ) ) ;
#4330 = VERTEX_POINT ( 'NONE', #27776 ) ;
#4331 = EDGE_CURVE ( 'NONE', #25273, #15079, #22952, .T. ) ;
#4332 = DIRECTION ( 'NONE',  ( 0.000000000000000000, 1.000000000000000000, 0.000000000000000000 ) ) ;
#4333 = CIRCLE ( 'NONE', #8958, 0.4999999999999981126 ) ;
#4334 = EDGE_CURVE ( 'NONE', #19799, #927, #26754, .T. ) ;
#4335 = CARTESIAN_POINT ( 'NONE',  ( -5.873421706809999421, -101.3150700380000018, 15.15334630729999965 ) ) ;
#4336 = CARTESIAN_POINT ( 'NONE',  ( 12.78426795600000077, -92.51541980399998977, 27.21084123129999810 ) ) ;
#4337 = EDGE_LOOP ( 'NONE', ( #16167, #17740, #7822, #7304 ) ) ;
#4338 = CARTESIAN_POINT ( 'NONE',  ( -19.27031001210522732, -97.04315770582992684, 7.370512498575622296 ) ) ;
#4339 = ORIENTED_EDGE ( 'NONE', *, *, #6688, .T. ) ;
#4340 = CARTESIAN_POINT ( 'NONE',  ( 21.04495798600000001, -93.87552356599999825, 13.16258487500000030 ) ) ;
#4341 = CARTESIAN_POINT ( 'NONE',  ( 46.38894337929999523, -73.82071635820000211, -3.552936482959999864 ) ) ;
#4342 = EDGE_CURVE ( 'NONE', #6001, #3048, #15615, .T. ) ;
#4343 = EDGE_LOOP ( 'NONE', ( #18037, #5993, #19219, #19660, #27783, #18851, #19413 ) ) ;
#4344 = AXIS2_PLACEMENT_3D ( 'NONE', #8270, #21408, #17170 ) ;
#4345 = CARTESIAN_POINT ( 'NONE',  ( -41.93083144778949389, -65.74402527487352188, 1.006537937124212911 ) ) ;
#4346 = CARTESIAN_POINT ( 'NONE',  ( -21.80755408569999787, -80.04548719450001215, -32.63464586140000279 ) ) ;
#4347 = DIRECTION ( 'NONE',  ( 0.000000000000000000, -1.000000000000000000, 0.000000000000000000 ) ) ;
#4348 = CARTESIAN_POINT ( 'NONE',  ( -20.51010360339999750, -92.96321827540000982, -20.71562969230000206 ) ) ;
#4349 = DIRECTION ( 'NONE',  ( 1.000000000000000000, 0.000000000000000000, 0.000000000000000000 ) ) ;
#4350 = ORIENTED_EDGE ( 'NONE', *, *, #27903, .T. ) ;
#4351 = CARTESIAN_POINT ( 'NONE',  ( 36.33976381259999755, -73.99988452930000449, -13.99159891000000044 ) ) ;
#4352 = B_SPLINE_CURVE_WITH_KNOTS ( 'NONE', 4,
 ( #8581, #10891, #26514, #11028, #11191 ),
 .UNSPECIFIED., .F., .F.,
 ( 5, 5 ),
 ( 0.000000000000000000, 1.000000000000000000 ),
 .UNSPECIFIED. ) ;
#4353 = CARTESIAN_POINT ( 'NONE',  ( 12.08982211680000063, -101.2010924020000004, -9.314613846919998608 ) ) ;
#4354 = CARTESIAN_POINT ( 'NONE',  ( 25.26718046270000073, -18.50000000000000000, 6.129403842640000377 ) ) ;
#4355 = CARTESIAN_POINT ( 'NONE',  ( -11.69653532996436063, -94.52419745024094766, -20.97822779232529200 ) ) ;
#4356 = CIRCLE ( 'NONE', #22042, 1.000000000000000444 ) ;
#4357 = CARTESIAN_POINT ( 'NONE',  ( 40.00000000000000000, -69.50000000000000000, 3.566319567039999839E-15 ) ) ;
#4358 = CARTESIAN_POINT ( 'NONE',  ( 29.80903961887878850, -92.62938374245408113, 6.455398338214653364 ) ) ;
#4359 = CARTESIAN_POINT ( 'NONE',  ( -18.41637023339999857, -19.15979404320000157, 12.71575957319999972 ) ) ;
#4360 = ORIENTED_EDGE ( 'NONE', *, *, #6094, .T. ) ;
#4361 = DIRECTION ( 'NONE',  ( 0.000000000000000000, 1.000000000000000000, 0.000000000000000000 ) ) ;
#4362 = DIRECTION ( 'NONE',  ( 0.000000000000000000, 1.000000000000000000, 0.000000000000000000 ) ) ;
#4363 = CARTESIAN_POINT ( 'NONE',  ( -23.99741465927868234, -92.66191076881281674, -18.82493379776595432 ) ) ;
#4364 = CARTESIAN_POINT ( 'NONE',  ( 22.80182977730000005, -18.50000000000000000, 8.962866840220000242 ) ) ;
#4365 = CARTESIAN_POINT ( 'NONE',  ( -1.177688289451497061, -92.49999999999998579, -30.47756502919148147 ) ) ;
#4366 = AXIS2_PLACEMENT_3D ( 'NONE', #13336, #2884, #11441 ) ;
#4367 = PRODUCT_RELATED_PRODUCT_CATEGORY ( 'part', '', ( #26194 ) ) ;
#4368 = DIRECTION ( 'NONE',  ( 0.000000000000000000, 1.000000000000000000, 0.000000000000000000 ) ) ;
#4369 = ADVANCED_FACE ( 'NONE', ( #26712 ), #1800, .F. ) ;
#4370 = ORIENTED_EDGE ( 'NONE', *, *, #8559, .T. ) ;
#4371 = AXIS2_PLACEMENT_3D ( 'NONE', #1114, #5316, #7661 ) ;
#4372 = CARTESIAN_POINT ( 'NONE',  ( 19.76462585710000042, -98.69238697660000526, -0.3789175872999999695 ) ) ;
#4373 = ORIENTED_EDGE ( 'NONE', *, *, #26793, .T. ) ;
#4374 = AXIS2_PLACEMENT_3D ( 'NONE', #21491, #3857, #24532 ) ;
#4375 = CARTESIAN_POINT ( 'NONE',  ( 22.35420107259999867, -19.50000000000000000, 9.881343484100000296 ) ) ;
#4376 = CARTESIAN_POINT ( 'NONE',  ( 14.62247892739999955, -91.50000000000000000, 26.76626813769999913 ) ) ;
#4377 = EDGE_CURVE ( 'NONE', #17392, #25360, #13515, .T. ) ;
#4378 = ORIENTED_EDGE ( 'NONE', *, *, #23973, .F. ) ;
#4379 = CARTESIAN_POINT ( 'NONE',  ( 16.58537726420000169, -94.98812477769999418, 16.93952758609999876 ) ) ;
#4380 = ADVANCED_FACE ( 'NONE', ( #2675 ), #10053, .T. ) ;
#4381 = CARTESIAN_POINT ( 'NONE',  ( -8.862540297109999798, -96.28763787000001173, -20.93955327700000169 ) ) ;
#4382 = CARTESIAN_POINT ( 'NONE',  ( 7.462391103660000802, -101.2375126459999848, 13.25959037569999843 ) ) ;
#4383 = DIRECTION ( 'NONE',  ( 0.000000000000000000, -1.000000000000000000, 0.000000000000000000 ) ) ;
#4384 = DIRECTION ( 'NONE',  ( 0.000000000000000000, 1.000000000000000000, 0.000000000000000000 ) ) ;
#4385 = CIRCLE ( 'NONE', #4366, 30.50000000000000000 ) ;
#4386 = CARTESIAN_POINT ( 'NONE',  ( -10.21740987579999782, -18.50000000000000000, -18.48932970370000106 ) ) ;
#4387 = CARTESIAN_POINT ( 'NONE',  ( 47.20757201636944700, -79.28844410293223177, -0.9918251209386655942 ) ) ;
#4388 = ORIENTED_EDGE ( 'NONE', *, *, #27194, .T. ) ;
#4389 = CARTESIAN_POINT ( 'NONE',  ( 10.13270341610000180, -93.01085527740001169, -25.43967382270000144 ) ) ;
#4390 = CARTESIAN_POINT ( 'NONE',  ( 0.000000000000000000, -107.1975888269999899, 0.000000000000000000 ) ) ;
#4391 = DIRECTION ( 'NONE',  ( 1.000000000000000000, 0.000000000000000000, 0.000000000000000000 ) ) ;
#4392 = CARTESIAN_POINT ( 'NONE',  ( 28.66244647610000129, -93.00000000000000000, 10.42660836539999991 ) ) ;
#4393 = ORIENTED_EDGE ( 'NONE', *, *, #8059, .F. ) ;
#4394 = AXIS2_PLACEMENT_3D ( 'NONE', #22250, #13346, #16122 ) ;
#4395 = CARTESIAN_POINT ( 'NONE',  ( -0.8216735279219999910, -65.07443093669999712, -25.13632616349999793 ) ) ;
#4396 = CARTESIAN_POINT ( 'NONE',  ( -17.76804213369999985, -93.83763213849999829, 19.50200951540000105 ) ) ;
#4397 = DIRECTION ( 'NONE',  ( 0.9295286103719527793, 0.000000000000000000, 0.3687499999999814260 ) ) ;
#4398 = EDGE_LOOP ( 'NONE', ( #16457, #24875, #14601 ) ) ;
#4399 = FACE_OUTER_BOUND ( 'NONE', #21298, .T. ) ;
#4400 = AXIS2_PLACEMENT_3D ( 'NONE', #4895, #17865, #24418 ) ;
#4401 = CARTESIAN_POINT ( 'NONE',  ( 0.6960536556740000158, -100.3517545579999961, -16.73679824259999904 ) ) ;
#4402 = CARTESIAN_POINT ( 'NONE',  ( 24.27931843075214147, -74.17320152699277003, -30.68465547482643885 ) ) ;
#4403 = CARTESIAN_POINT ( 'NONE',  ( 15.66918838289999982, -101.3256027080000052, 2.740257563980000199 ) ) ;
#4404 = CARTESIAN_POINT ( 'NONE',  ( 23.19820347179999942, -63.60137401019999714, -8.029207517830000640 ) ) ;
#4405 = CARTESIAN_POINT ( 'NONE',  ( 36.22844186549999534, -74.00000000000000000, -13.75000000000000000 ) ) ;
#4406 = DIRECTION ( 'NONE',  ( 0.4794255386042000078, 0.000000000000000000, 0.8775825618903743131 ) ) ;
#4407 = EDGE_CURVE ( 'NONE', #15327, #12701, #9791, .T. ) ;
#4408 = ORIENTED_EDGE ( 'NONE', *, *, #23513, .T. ) ;
#4409 = CARTESIAN_POINT ( 'NONE',  ( 28.21920633877042661, -92.66972459461230471, 11.57265855722420511 ) ) ;
#4410 = CARTESIAN_POINT ( 'NONE',  ( 24.38417282560000032, -18.50000000000000000, 2.479391470229999950 ) ) ;
#4411 = AXIS2_PLACEMENT_3D ( 'NONE', #5838, #14721, #174 ) ;
#4412 = CARTESIAN_POINT ( 'NONE',  ( -3.055530930329999784, -94.70873613630000420, 23.49572349450000175 ) ) ;
#4413 = ORIENTED_EDGE ( 'NONE', *, *, #5538, .F. ) ;
#4414 = CARTESIAN_POINT ( 'NONE',  ( 8.920172905260001173, -94.54719310899999130, -22.12533866800000126 ) ) ;
#4415 = EDGE_CURVE ( 'NONE', #26598, #26756, #7392, .T. ) ;
#4416 = CARTESIAN_POINT ( 'NONE',  ( 4.362772401299999991, -17.50000000000000000, 7.986001313199998286 ) ) ;
#4417 = ORIENTED_EDGE ( 'NONE', *, *, #20782, .T. ) ;
#4418 = AXIS2_PLACEMENT_3D ( 'NONE', #14842, #18959, #27842 ) ;
#4419 = CARTESIAN_POINT ( 'NONE',  ( 27.05591625959999647, -101.1889999979999999, 12.64646362319999895 ) ) ;
#4420 = DIRECTION ( 'NONE',  ( 0.000000000000000000, 1.000000000000000000, 0.000000000000000000 ) ) ;
#4421 = CARTESIAN_POINT ( 'NONE',  ( 9.038647844559999811, -35.72724450169999955, -19.55068585869999964 ) ) ;
#4422 = DIRECTION ( 'NONE',  ( 0.8775825618903724257, 0.000000000000000000, 0.4794255386042037825 ) ) ;
#4423 = CARTESIAN_POINT ( 'NONE',  ( 9.165534020729998232, -98.33329995120000433, 16.60371393490000003 ) ) ;
#4424 = DIRECTION ( 'NONE',  ( -0.2653025664749695811, -0.9430444279528923390, -0.2007031517659765008 ) ) ;
#4425 = CARTESIAN_POINT ( 'NONE',  ( -7.384731337359999870, -94.63960162979999780, -22.55849179059999798 ) ) ;
#4426 = CARTESIAN_POINT ( 'NONE',  ( 14.16648691321227815, -92.50630337894781974, 27.01069259898191532 ) ) ;
#4427 = ORIENTED_EDGE ( 'NONE', *, *, #301, .T. ) ;
#4428 = CARTESIAN_POINT ( 'NONE',  ( 11.66470437849999975, -101.1042759770000004, -10.63853114260000154 ) ) ;
#4429 = DIRECTION ( 'NONE',  ( -0.8775825618903722036, 0.000000000000000000, 0.4794255386042041156 ) ) ;
#4430 = DIRECTION ( 'NONE',  ( 0.4794255386042040601, 0.000000000000000000, 0.8775825618903720926 ) ) ;
#4431 = CARTESIAN_POINT ( 'NONE',  ( 23.92053897610000135, -93.00000000000000000, -18.92241567810000191 ) ) ;
#4432 = DIRECTION ( 'NONE',  ( 0.000000000000000000, 0.000000000000000000, 1.000000000000000000 ) ) ;
#4433 = CARTESIAN_POINT ( 'NONE',  ( -12.24426935569999841, -66.16381828960000178, -22.75094555550000308 ) ) ;
#4434 = CARTESIAN_POINT ( 'NONE',  ( -38.38520059305543697, -65.09619745166223481, -2.875091199968994093 ) ) ;
#4435 = DIRECTION ( 'NONE',  ( 0.000000000000000000, -1.000000000000000000, 0.000000000000000000 ) ) ;
#4436 = CARTESIAN_POINT ( 'NONE',  ( 22.57356305922917628, -93.98969193917014309, 13.12592337714520241 ) ) ;
#4437 = ORIENTED_EDGE ( 'NONE', *, *, #5861, .T. ) ;
#4438 = CARTESIAN_POINT ( 'NONE',  ( 7.599202688140000106, -18.61794787459999867, -20.27108524870000039 ) ) ;
#4439 = B_SPLINE_CURVE_WITH_KNOTS ( 'NONE', 5,
 ( #5037, #5190, #27049, #7095, #15958, #4600 ),
 .UNSPECIFIED., .F., .F.,
 ( 6, 6 ),
 ( 0.000000000000000000, 1.000000000000000000 ),
 .UNSPECIFIED. ) ;
#4440 = CARTESIAN_POINT ( 'NONE',  ( 7.750008477179999744, -101.2850603089999879, 13.91843549959999926 ) ) ;
#4441 = EDGE_CURVE ( 'NONE', #8283, #15872, #17711, .T. ) ;
#4442 = CARTESIAN_POINT ( 'NONE',  ( -11.50108207929999971, -62.13448031410000283, 21.04282218430000029 ) ) ;
#4443 = CARTESIAN_POINT ( 'NONE',  ( 0.000000000000000000, -84.75000000000000000, 0.000000000000000000 ) ) ;
#4444 = FACE_OUTER_BOUND ( 'NONE', #8413, .T. ) ;
#4445 = CARTESIAN_POINT ( 'NONE',  ( -20.22316239190000076, -53.78538132969999452, 14.63937920919999947 ) ) ;
#4446 = EDGE_CURVE ( 'NONE', #28390, #13967, #21186, .T. ) ;
#4447 = CARTESIAN_POINT ( 'NONE',  ( -17.42343749999999858, -79.50000000000000000, 43.92022684009999978 ) ) ;
#4448 = CIRCLE ( 'NONE', #20765, 60.85000000000000142 ) ;
#4449 = EDGE_LOOP ( 'NONE', ( #11293, #17968, #10763, #8184, #9815, #6982 ) ) ;
#4450 = DIRECTION ( 'NONE',  ( -0.9839596076661280000, 0.000000000000000000, -0.1783913968820232399 ) ) ;
#4451 = CARTESIAN_POINT ( 'NONE',  ( 29.25372036608126081, -74.33334105576250295, -26.12545324891368992 ) ) ;
#4452 = CARTESIAN_POINT ( 'NONE',  ( 7.314380512960000580, -73.97629583769999329, -39.54203581849999694 ) ) ;
#4453 = ORIENTED_EDGE ( 'NONE', *, *, #6926, .T. ) ;
#4454 = DIRECTION ( 'NONE',  ( 1.000000000000000000, 0.000000000000000000, 0.000000000000000000 ) ) ;
#4455 = ORIENTED_EDGE ( 'NONE', *, *, #9170, .T. ) ;
#4456 = DIRECTION ( 'NONE',  ( 0.000000000000000000, 1.000000000000000000, 0.000000000000000000 ) ) ;
#4457 = CARTESIAN_POINT ( 'NONE',  ( 21.00956971319999766, -32.71502530459999747, 9.728137178119999007 ) ) ;
#4458 = AXIS2_PLACEMENT_3D ( 'NONE', #20579, #20876, #5280 ) ;
#4459 = CARTESIAN_POINT ( 'NONE',  ( 0.000000000000000000, -11.00000000000000000, 24.50000000000000000 ) ) ;
#4460 = CARTESIAN_POINT ( 'NONE',  ( 24.46247886789999981, -92.83702889919999279, -17.01249244230000102 ) ) ;
#4461 = CARTESIAN_POINT ( 'NONE',  ( 19.36781163719999910, -19.46510053389999939, 10.50580276810000058 ) ) ;
#4462 = CARTESIAN_POINT ( 'NONE',  ( 11.10253387620000076, -70.67754404800000145, -26.52623155260000232 ) ) ;
#4463 = CARTESIAN_POINT ( 'NONE',  ( 14.07913102130000027, -97.93128678259999731, -14.20797793960000099 ) ) ;
#4464 = EDGE_CURVE ( 'NONE', #18925, #14853, #5045, .T. ) ;
#4465 = VERTEX_POINT ( 'NONE', #12629 ) ;
#4466 = DIRECTION ( 'NONE',  ( 1.000000000000000000, 0.000000000000000000, 0.000000000000000000 ) ) ;
#4467 = DIRECTION ( 'NONE',  ( 0.2414462220490750377, 0.000000000000000000, 0.9704142011833034598 ) ) ;
#4468 = CARTESIAN_POINT ( 'NONE',  ( -13.20967871329999888, -99.69348480060000384, -11.20452871620000046 ) ) ;
#4469 = CARTESIAN_POINT ( 'NONE',  ( 21.58901261035154562, -19.48534489990760221, 9.514599319613230577 ) ) ;
#4470 = CARTESIAN_POINT ( 'NONE',  ( -40.35968420210000573, -74.26794181949999540, -7.250122995599999065 ) ) ;
#4471 = EDGE_LOOP ( 'NONE', ( #8423, #17164, #17093, #24858 ) ) ;
#4472 = DIRECTION ( 'NONE',  ( 0.6285074900730011072, 0.000000000000000000, -0.7778035323409996371 ) ) ;
#4473 = ORIENTED_EDGE ( 'NONE', *, *, #24881, .F. ) ;
#4474 = EDGE_CURVE ( 'NONE', #2458, #7636, #23656, .T. ) ;
#4475 = EDGE_CURVE ( 'NONE', #6357, #4763, #14182, .T. ) ;
#4476 = DIRECTION ( 'NONE',  ( 1.555923129751019993E-15, 1.000000000000000000, 1.096297985141100053E-15 ) ) ;
#4477 = CARTESIAN_POINT ( 'NONE',  ( -5.750263158049999213, -100.9405345029999950, 14.87178882549999948 ) ) ;
#4478 = ORIENTED_EDGE ( 'NONE', *, *, #2009, .T. ) ;
#4479 = CARTESIAN_POINT ( 'NONE',  ( -19.68295015794943126, -96.39141346198870508, 8.586065742081073537 ) ) ;
#4480 = ORIENTED_EDGE ( 'NONE', *, *, #22135, .T. ) ;
#4481 = DIRECTION ( 'NONE',  ( 0.000000000000000000, 1.000000000000000000, 0.000000000000000000 ) ) ;
#4482 = CARTESIAN_POINT ( 'NONE',  ( 21.21659859809999915, -93.92589142420000314, 13.52749749360000031 ) ) ;
#4483 = DIRECTION ( 'NONE',  ( 0.000000000000000000, 1.000000000000000000, 0.000000000000000000 ) ) ;
#4484 = ORIENTED_EDGE ( 'NONE', *, *, #24003, .T. ) ;
#4485 = CARTESIAN_POINT ( 'NONE',  ( 16.46460381570141962, -94.70873790529931568, 17.03825317169986064 ) ) ;
#4486 = CARTESIAN_POINT ( 'NONE',  ( 22.25602728219974935, -57.44036991818945381, 10.13208872879983424 ) ) ;
#4487 = CARTESIAN_POINT ( 'NONE',  ( -37.75000000000000000, -65.00000000000000000, -0.7216878364849999006 ) ) ;
#4488 = DIRECTION ( 'NONE',  ( 0.000000000000000000, 1.000000000000000000, 0.000000000000000000 ) ) ;
#4489 = CARTESIAN_POINT ( 'NONE',  ( -6.665307709260000379, -92.50000000000000000, -13.13558364449999871 ) ) ;
#4490 = VERTEX_POINT ( 'NONE', #23076 ) ;
#4491 = CARTESIAN_POINT ( 'NONE',  ( -5.909020910341554078, -101.4218099524584602, 15.05258134268767378 ) ) ;
#4492 = DIRECTION ( 'NONE',  ( 0.4794255386042036715, 0.000000000000000000, 0.8775825618903724257 ) ) ;
#4493 = CARTESIAN_POINT ( 'NONE',  ( -38.62788659690000515, -74.00000000000000000, 7.627568735119999666 ) ) ;
#4494 = CARTESIAN_POINT ( 'NONE',  ( -22.06287047380000033, -74.01117791779999777, -32.15233126369999894 ) ) ;
#4495 = ADVANCED_FACE ( 'NONE', ( #3905 ), #18700, .F. ) ;
#4496 = CARTESIAN_POINT ( 'NONE',  ( -1.977702949901789520, -100.7438493865795692, -16.89156302428552436 ) ) ;
#4497 = DIRECTION ( 'NONE',  ( 0.000000000000000000, -1.000000000000000000, 0.000000000000000000 ) ) ;
#4498 = CARTESIAN_POINT ( 'NONE',  ( -7.327696733890933345, -73.99971689350539350, 39.44377223208145011 ) ) ;
#4499 = CARTESIAN_POINT ( 'NONE',  ( -18.78219790299999659, -19.46510053389999939, 11.52011550950000007 ) ) ;
#4500 = ORIENTED_EDGE ( 'NONE', *, *, #16529, .T. ) ;
#4501 = CARTESIAN_POINT ( 'NONE',  ( -36.92846103339999786, -63.00000000000000000, 1.677989385109999843 ) ) ;
#4502 = FACE_OUTER_BOUND ( 'NONE', #22257, .T. ) ;
#4503 = CARTESIAN_POINT ( 'NONE',  ( -24.05612431029909715, -92.62938374242331463, -18.74977050185806604 ) ) ;
#4504 = DIRECTION ( 'NONE',  ( 0.9952295494196657932, 0.000000000000000000, 0.09756097560976527416 ) ) ;
#4505 = DIRECTION ( 'NONE',  ( -0.09756097560976760563, 0.000000000000000000, -0.9952295494196654602 ) ) ;
#4506 = PRODUCT_DEFINITION_CONTEXT ( 'detailed design', #8834, 'design' ) ;
#4507 = B_SPLINE_SURFACE_WITH_KNOTS ( 'NONE', 5, 5, ( 
 ( #22956, #14474, #23371, #7659, #5314, #21190, #27749, #5593, #27619 ),
 ( #12135, #18574, #14203, #11857, #7516, #677, #18722, #7787, #23097 ),
 ( #1112, #1241, #7358, #25287, #27469, #27172, #16079, #27318, #9527 ),
 ( #2997, #24979, #5012, #20617, #13900, #20767, #16525, #22804, #16375 ),
 ( #2842, #973, #20908, #18428, #25422, #5454, #14337, #23230, #3280 ),
 ( #11702, #16221, #25136, #5728, #27876, #17079, #17370, #25973, #3552 ) ),
 .UNSPECIFIED., .F., .F., .F.,
 ( 6, 6 ),
 ( 6, 3, 6 ),
 ( 36.59856967279999651, 66.18347591719999912 ),
 ( 0.000000000000000000, 1.000000000000000000, 2.000000000000000000 ),
 .UNSPECIFIED. ) ;
#4508 = CARTESIAN_POINT ( 'NONE',  ( 0.000000000000000000, 0.000000000000000000, 0.000000000000000000 ) ) ;
#4509 = CYLINDRICAL_SURFACE ( 'NONE', #18633, 0.4999999999999982236 ) ;
#4510 = ORIENTED_EDGE ( 'NONE', *, *, #28496, .F. ) ;
#4511 = CARTESIAN_POINT ( 'NONE',  ( -41.00000000000000000, -82.25000000000000000, 10.20110288159999890 ) ) ;
#4512 = CARTESIAN_POINT ( 'NONE',  ( 21.31239851289999976, -97.32097375579999721, -2.189509325750000013 ) ) ;
#4513 = ORIENTED_EDGE ( 'NONE', *, *, #4162, .F. ) ;
#4514 = CARTESIAN_POINT ( 'NONE',  ( -11.32359561920000068, -49.87552377809999626, 20.13167398270000064 ) ) ;
#4515 = DIRECTION ( 'NONE',  ( 0.5301416321220552286, 0.000000000000000000, 0.8479091047340884257 ) ) ;
#4516 = EDGE_LOOP ( 'NONE', ( #16483, #13971, #7468, #3315 ) ) ;
#4517 = CARTESIAN_POINT ( 'NONE',  ( 13.46942446439999941, -96.16288795909999010, 17.21854863529999946 ) ) ;
#4518 = CARTESIAN_POINT ( 'NONE',  ( -5.273680924649999824, -107.5000000000000000, -9.653408180790000515 ) ) ;
#4519 = AXIS2_PLACEMENT_3D ( 'NONE', #14714, #10456, #14979 ) ;
#4520 = CARTESIAN_POINT ( 'NONE',  ( 1.631276547419999945, -94.59276292389999696, 23.74086995720000104 ) ) ;
#4521 = CARTESIAN_POINT ( 'NONE',  ( 8.681080848429999719, -37.64807918700000045, -21.92361636220000065 ) ) ;
#4522 = CARTESIAN_POINT ( 'NONE',  ( -18.01262108789999772, -98.65106254609999326, 4.840278925599998949 ) ) ;
#4523 = CARTESIAN_POINT ( 'NONE',  ( -10.46177781019999919, -18.61797548019999837, -19.17903742680000079 ) ) ;
#4524 = CARTESIAN_POINT ( 'NONE',  ( 21.49292127480903503, -37.16720133427794082, -7.554708306457890821 ) ) ;
#4525 = VERTEX_POINT ( 'NONE', #16505 ) ;
#4526 = CARTESIAN_POINT ( 'NONE',  ( -17.94180966909999597, -18.50000000000000000, 18.81731824139999887 ) ) ;
#4527 = FACE_OUTER_BOUND ( 'NONE', #21595, .T. ) ;
#4528 = CARTESIAN_POINT ( 'NONE',  ( -36.25000000000000000, -69.00000000000000000, 2.124561919619999789E-15 ) ) ;
#4529 = VERTEX_POINT ( 'NONE', #10438 ) ;
#4530 = DIRECTION ( 'NONE',  ( 0.000000000000000000, -1.000000000000000000, 0.000000000000000000 ) ) ;
#4531 = CARTESIAN_POINT ( 'NONE',  ( -13.55845395530000097, -93.00000046469999404, 27.19007896420000137 ) ) ;
#4532 = CARTESIAN_POINT ( 'NONE',  ( -14.60044964929999978, -79.81260323630000642, 36.96978765280000090 ) ) ;
#4533 = ORIENTED_EDGE ( 'NONE', *, *, #6978, .T. ) ;
#4534 = CIRCLE ( 'NONE', #12864, 7.250000000000000000 ) ;
#4535 = ADVANCED_FACE ( 'NONE', ( #19356 ), #448, .T. ) ;
#4536 =( GEOMETRIC_REPRESENTATION_CONTEXT ( 3 ) GLOBAL_UNCERTAINTY_ASSIGNED_CONTEXT ( ( #16739 ) ) GLOBAL_UNIT_ASSIGNED_CONTEXT ( ( #7496, #18263, #9510 ) ) REPRESENTATION_CONTEXT ( 'NONE', 'WORKASPACE' ) );
#4537 = CARTESIAN_POINT ( 'NONE',  ( 27.49606721070000148, -67.46050995630001523, 1.934822350479999953 ) ) ;
#4538 = CARTESIAN_POINT ( 'NONE',  ( -12.92437881006504874, -101.4628082233713258, -9.386789896503060504 ) ) ;
#4539 = CARTESIAN_POINT ( 'NONE',  ( 0.8834120860809999698, -100.8023006570000035, -15.75170354469999978 ) ) ;
#4540 = CARTESIAN_POINT ( 'NONE',  ( 14.28941763439999946, -101.1889999979999999, -3.575252188409999921 ) ) ;
#4541 = CARTESIAN_POINT ( 'NONE',  ( -19.79578083032381031, -57.47815899606673895, 12.40825019997615364 ) ) ;
#4542 = ADVANCED_FACE ( 'NONE', ( #27447 ), #27598, .T. ) ;
#4543 = ADVANCED_FACE ( 'NONE', ( #22935 ), #804, .T. ) ;
#4544 = DIRECTION ( 'NONE',  ( 1.000000000000000000, 0.000000000000000000, 0.000000000000000000 ) ) ;
#4545 = CONICAL_SURFACE ( 'NONE', #398, 24.40223267850002031, 0.7949521073230001456 ) ;
#4546 = B_SPLINE_CURVE_WITH_KNOTS ( 'NONE', 3,
 ( #14225, #13628, #22536, #4894 ),
 .UNSPECIFIED., .F., .F.,
 ( 4, 4 ),
 ( 8.029182300089999980E-15, 6.855861996790000745 ),
 .UNSPECIFIED. ) ;
#4547 = CARTESIAN_POINT ( 'NONE',  ( 28.07360232333943628, -92.59033770620598602, 11.92235161152704670 ) ) ;
#4548 = CARTESIAN_POINT ( 'NONE',  ( 7.181689689069999716, -99.92967571559999840, 15.80535034289999885 ) ) ;
#4549 = CARTESIAN_POINT ( 'NONE',  ( 17.23458459540000121, -95.71128709549999769, 14.57456978229999933 ) ) ;
#4550 = VERTEX_POINT ( 'NONE', #20889 ) ;
#4551 = CARTESIAN_POINT ( 'NONE',  ( 36.36887067909999871, -79.00000000000000000, -14.85406736540000061 ) ) ;
#4552 = DIRECTION ( 'NONE',  ( 0.000000000000000000, 1.000000000000000000, 0.000000000000000000 ) ) ;
#4553 = CONICAL_SURFACE ( 'NONE', #24565, 55.67692378859999280, 1.047197551199999799 ) ;
#4554 = DIRECTION ( 'NONE',  ( 0.000000000000000000, 1.000000000000000000, 0.000000000000000000 ) ) ;
#4555 = CARTESIAN_POINT ( 'NONE',  ( 23.47058412056877330, -19.48405044125010832, 1.414240622653882173 ) ) ;
#4556 = ORIENTED_EDGE ( 'NONE', *, *, #19091, .T. ) ;
#4557 = DIRECTION ( 'NONE',  ( 0.000000000000000000, -1.000000000000000000, 0.000000000000000000 ) ) ;
#4558 = CARTESIAN_POINT ( 'NONE',  ( 8.391519205499999856, -36.85003413439999775, -21.45231170510000140 ) ) ;
#4559 = CARTESIAN_POINT ( 'NONE',  ( 7.894290250409162546, -19.46654752400787203, -20.57171819332643636 ) ) ;
#4560 = ORIENTED_EDGE ( 'NONE', *, *, #3456, .F. ) ;
#4561 = DIRECTION ( 'NONE',  ( 0.000000000000000000, 0.000000000000000000, -1.000000000000000000 ) ) ;
#4562 = SPHERICAL_SURFACE ( 'NONE', #25663, 2.000000000000000000 ) ;
#4563 = CARTESIAN_POINT ( 'NONE',  ( -12.25492964594734779, -19.47261237683157020, 19.18132429780293080 ) ) ;
#4564 = CARTESIAN_POINT ( 'NONE',  ( -7.550577645110000624, -94.89196973819998959, -22.44319288410000368 ) ) ;
#4565 = CARTESIAN_POINT ( 'NONE',  ( -20.38647250310078718, -92.66455718077615700, -22.68571774292804122 ) ) ;
#4566 = PRODUCT_DEFINITION_FORMATION_WITH_SPECIFIED_SOURCE ( 'ANY', '', #3620, .NOT_KNOWN. ) ;
#4567 = ORIENTED_EDGE ( 'NONE', *, *, #6819, .T. ) ;
#4568 = CARTESIAN_POINT ( 'NONE',  ( 11.83146313070000133, -101.1461874320000049, -11.00634697169999932 ) ) ;
#4569 = LINE ( 'NONE', #8929, #11088 ) ;
#4570 = CARTESIAN_POINT ( 'NONE',  ( 11.46395552116856464, -97.04146848922184176, 17.18158243287650677 ) ) ;
#4571 = EDGE_CURVE ( 'NONE', #24255, #9243, #28130, .T. ) ;
#4572 = DIRECTION ( 'NONE',  ( 0.000000000000000000, 1.000000000000000000, 0.000000000000000000 ) ) ;
#4573 = B_SPLINE_SURFACE_WITH_KNOTS ( 'NONE', 5, 5, ( 
 ( #1099, #9939, #27740, #26687, #17210, #15001, #28566, #8735, #4090 ),
 ( #10618, #13259, #8601, #6577, #3952, #17652, #23772, #12676, #1775 ),
 ( #22166, #2206, #14865, #2071, #26533, #28422, #4240, #3814, #6418 ),
 ( #15142, #24050, #17358, #23915, #21725, #15282, #26102, #17504, #12958 ),
 ( #10482, #15438, #26389, #11050, #22023, #21872, #19965, #19394, #17796 ),
 ( #12815, #24204, #13112, #19534, #21587, #6128, #8455, #6276, #10910 ) ),
 .UNSPECIFIED., .F., .F., .F.,
 ( 6, 6 ),
 ( 6, 3, 6 ),
 ( 15.94303934750000096, 69.72897805040000208 ),
 ( 0.000000000000000000, 1.000000000000000000, 2.000000000000000000 ),
 .UNSPECIFIED. ) ;
#4574 = B_SPLINE_CURVE_WITH_KNOTS ( 'NONE', 5,
 ( #25923, #12780, #17172, #17465, #26061, #3637, #15243, #24162, #6089, #4049, #19363, #26351, #19637, #5819, #4196, #14829, #13071, #1606 ),
 .UNSPECIFIED., .F., .F.,
 ( 6, 3, 3, 3, 3, 6 ),
 ( 0.000000000000000000, 1.124498255630000054, 2.252774941520000240, 3.380756636290000117, 4.508382774200000220, 5.576981603780000185 ),
 .UNSPECIFIED. ) ;
#4575 = DIRECTION ( 'NONE',  ( 0.000000000000000000, 1.000000000000000000, 0.000000000000000000 ) ) ;
#4576 = CARTESIAN_POINT ( 'NONE',  ( -12.61432613040000028, -66.29767256870000836, -22.40516107950000091 ) ) ;
#4577 = CARTESIAN_POINT ( 'NONE',  ( 9.718892398710000435, -93.00000000000000000, 28.91008700340000104 ) ) ;
#4578 = CARTESIAN_POINT ( 'NONE',  ( -10.20110288159999890, -84.00000000000000000, -41.00000000000000000 ) ) ;
#4579 = CARTESIAN_POINT ( 'NONE',  ( 28.17677534670164263, -93.02765837720463082, 8.900282725603984701 ) ) ;
#4580 = ORIENTED_EDGE ( 'NONE', *, *, #19698, .F. ) ;
#4581 = EDGE_CURVE ( 'NONE', #21750, #11312, #6936, .T. ) ;
#4582 = CARTESIAN_POINT ( 'NONE',  ( 36.25015153569999882, -74.79528478139999947, -15.04955598449999954 ) ) ;
#4583 = VECTOR ( 'NONE', #17765, 1000.000000000000000 ) ;
#4584 = VECTOR ( 'NONE', #952, 1000.000000000000000 ) ;
#4585 = CARTESIAN_POINT ( 'NONE',  ( 8.037687215760000115, -101.3302889870000030, 13.99636585439999870 ) ) ;
#4586 = ORIENTED_EDGE ( 'NONE', *, *, #11404, .T. ) ;
#4587 = CARTESIAN_POINT ( 'NONE',  ( -14.88246912999999871, -67.03279743669999391, 22.48335306070000073 ) ) ;
#4588 = DIRECTION ( 'NONE',  ( 0.000000000000000000, -1.000000000000000000, 0.000000000000000000 ) ) ;
#4589 = CARTESIAN_POINT ( 'NONE',  ( 7.242418264991816734, -74.21175622417943885, 40.33192879158703192 ) ) ;
#4590 = CARTESIAN_POINT ( 'NONE',  ( -23.61874792040000060, -94.52293239719999463, -3.856435390649999739 ) ) ;
#4591 = CARTESIAN_POINT ( 'NONE',  ( -27.18988201479999844, -34.70155444569999759, -49.77074518290000071 ) ) ;
#4592 = CARTESIAN_POINT ( 'NONE',  ( 15.97524996809999998, -100.1512121650000040, 4.654508469899999668 ) ) ;
#4593 = VERTEX_POINT ( 'NONE', #21971 ) ;
#4594 = B_SPLINE_CURVE_WITH_KNOTS ( 'NONE', 3,
 ( #4294, #8225, #21928, #14914, #15338, #22214 ),
 .UNSPECIFIED., .F., .F.,
 ( 4, 2, 4 ),
 ( 0.000000000000000000, 0.5000000000000000000, 1.000000000000000000 ),
 .UNSPECIFIED. ) ;
#4595 = FACE_BOUND ( 'NONE', #12615, .T. ) ;
#4596 = CARTESIAN_POINT ( 'NONE',  ( 7.219507042790000106, -73.62951539670000045, -39.18035607859999914 ) ) ;
#4597 = ORIENTED_EDGE ( 'NONE', *, *, #18469, .F. ) ;
#4598 = CARTESIAN_POINT ( 'NONE',  ( 7.937989663683267416, -92.55017404142785153, 29.44891095136318881 ) ) ;
#4599 = DIRECTION ( 'NONE',  ( 3.652049423109066841E-16, 0.000000000000000000, -1.000000000000000000 ) ) ;
#4600 = CARTESIAN_POINT ( 'NONE',  ( -8.209463884390000743, -99.53431386179998697, 15.35748973489999969 ) ) ;
#4601 = AXIS2_PLACEMENT_3D ( 'NONE', #5149, #20750, #4709 ) ;
#4602 = CARTESIAN_POINT ( 'NONE',  ( -9.762708992400000341, -18.50000000000000000, -19.20397640299999864 ) ) ;
#4603 = EDGE_CURVE ( 'NONE', #13115, #26201, #16701, .T. ) ;
#4604 = DIRECTION ( 'NONE',  ( 0.8775825618903720926, 0.000000000000000000, 0.4794255386042039491 ) ) ;
#4605 = CARTESIAN_POINT ( 'NONE',  ( -7.234868202896564071, -73.70809116070437028, -39.52985788730124739 ) ) ;
#4606 = EDGE_CURVE ( 'NONE', #8919, #19884, #8319, .T. ) ;
#4607 = CARTESIAN_POINT ( 'NONE',  ( 20.73142793440000275, -60.32026811789999954, 11.32541297100000044 ) ) ;
#4608 = DIRECTION ( 'NONE',  ( -0.7071067811865474617, 0.000000000000000000, 0.7071067811865474617 ) ) ;
#4609 = CARTESIAN_POINT ( 'NONE',  ( 13.80438629439999865, -99.83167544280000527, -10.46687976449999979 ) ) ;
#4610 = ORIENTED_EDGE ( 'NONE', *, *, #24145, .F. ) ;
#4611 = DIRECTION ( 'NONE',  ( 0.000000000000000000, 1.000000000000000000, 0.000000000000000000 ) ) ;
#4612 = CARTESIAN_POINT ( 'NONE',  ( -40.00000000000000000, -94.00000000000000000, 0.000000000000000000 ) ) ;
#4613 = CARTESIAN_POINT ( 'NONE',  ( -12.32361334809999853, -100.1340845430000002, -11.17997075410000107 ) ) ;
#4614 = CARTESIAN_POINT ( 'NONE',  ( 20.56960363573175243, -19.47131810281557307, 9.532984917462295371 ) ) ;
#4615 = CARTESIAN_POINT ( 'NONE',  ( 14.32275000858649250, -96.09421897364175891, 17.10293378353320648 ) ) ;
#4616 = ORIENTED_EDGE ( 'NONE', *, *, #1278, .T. ) ;
#4617 = EDGE_CURVE ( 'NONE', #19075, #17884, #19038, .T. ) ;
#4618 = AXIS2_PLACEMENT_3D ( 'NONE', #21047, #16073, #11852 ) ;
#4619 = CARTESIAN_POINT ( 'NONE',  ( 26.64225616468215563, -92.66972459460608036, -14.84722933505276465 ) ) ;
#4620 = ORIENTED_EDGE ( 'NONE', *, *, #15788, .F. ) ;
#4621 = CIRCLE ( 'NONE', #8299, 7.249999999999999112 ) ;
#4622 = CIRCLE ( 'NONE', #25601, 6.000000000000000000 ) ;
#4623 = TOROIDAL_SURFACE ( 'NONE', #28342, 9.000000000000000000, 2.000000000000000000 ) ;
#4624 = DIRECTION ( 'NONE',  ( 0.1279666792900072403, 8.881784197000502906E-16, -0.9917784676990565318 ) ) ;
#4625 = DIRECTION ( 'NONE',  ( 1.000000000000000000, 0.000000000000000000, 0.000000000000000000 ) ) ;
#4626 = CARTESIAN_POINT ( 'NONE',  ( 19.64679318960000032, -35.95469792330000303, -9.266762188240001308 ) ) ;
#4627 = CARTESIAN_POINT ( 'NONE',  ( 12.77963394200000025, -92.50000200689999019, 27.13243699659999919 ) ) ;
#4628 = VERTEX_POINT ( 'NONE', #24594 ) ;
#4629 = ORIENTED_EDGE ( 'NONE', *, *, #5318, .F. ) ;
#4630 = CARTESIAN_POINT ( 'NONE',  ( -22.90089770769782618, -70.95732848294369433, 15.81452471505874158 ) ) ;
#4631 = CARTESIAN_POINT ( 'NONE',  ( 26.23214993620000257, -92.98926460689999374, 10.85177180670000041 ) ) ;
#4632 = FACE_OUTER_BOUND ( 'NONE', #8473, .T. ) ;
#4633 = ORIENTED_EDGE ( 'NONE', *, *, #21807, .T. ) ;
#4634 = DIRECTION ( 'NONE',  ( 0.000000000000000000, 1.000000000000000000, 0.000000000000000000 ) ) ;
#4635 = CARTESIAN_POINT ( 'NONE',  ( -22.13232309480000026, -79.66742592930000910, -32.73892524850000285 ) ) ;
#4636 = CARTESIAN_POINT ( 'NONE',  ( 11.92432098210000113, -101.1411470200000053, -9.728253486470000766 ) ) ;
#4637 = DIRECTION ( 'NONE',  ( 0.000000000000000000, 1.000000000000000000, 0.000000000000000000 ) ) ;
#4638 = ORIENTED_EDGE ( 'NONE', *, *, #19763, .T. ) ;
#4639 = CIRCLE ( 'NONE', #23709, 0.3500000000000003664 ) ;
#4640 = CARTESIAN_POINT ( 'NONE',  ( -6.285925807789999986, -101.6484611540000031, 14.71350185169999847 ) ) ;
#4641 = EDGE_CURVE ( 'NONE', #452, #11938, #24629, .T. ) ;
#4642 = FACE_OUTER_BOUND ( 'NONE', #3033, .T. ) ;
#4643 = DIRECTION ( 'NONE',  ( 0.9704142011833034598, 0.000000000000000000, -0.2414462220490750932 ) ) ;
#4644 = CARTESIAN_POINT ( 'NONE',  ( 26.77683864449999973, -26.59999999999999787, 49.01467436490000296 ) ) ;
#4645 = CARTESIAN_POINT ( 'NONE',  ( -2.565530488230000294, -57.41946977150000464, -24.92670969510000134 ) ) ;
#4646 = CARTESIAN_POINT ( 'NONE',  ( 0.000000000000000000, -16.00000000000000000, 0.000000000000000000 ) ) ;
#4647 = CARTESIAN_POINT ( 'NONE',  ( -38.55000000000000426, -65.14977478849999670, 2.857883832489999776 ) ) ;
#4648 = CARTESIAN_POINT ( 'NONE',  ( -18.56585641370000062, -19.46390881170000142, 11.87275530319999817 ) ) ;
#4649 = ORIENTED_EDGE ( 'NONE', *, *, #2009, .F. ) ;
#4650 = CARTESIAN_POINT ( 'NONE',  ( -7.550578184249999047, -94.89197151660000884, -22.44319203070000057 ) ) ;
#4651 = CARTESIAN_POINT ( 'NONE',  ( 0.000000000000000000, -36.20000000000000284, 0.000000000000000000 ) ) ;
#4652 = FACE_OUTER_BOUND ( 'NONE', #28454, .T. ) ;
#4653 = DIRECTION ( 'NONE',  ( 0.000000000000000000, -1.000000000000000000, 0.000000000000000000 ) ) ;
#4654 = CARTESIAN_POINT ( 'NONE',  ( 47.11905485129999960, -79.66016163019999397, -1.826180561010000147 ) ) ;
#4655 = CARTESIAN_POINT ( 'NONE',  ( 0.000000000000000000, -13.40000000000000036, 0.000000000000000000 ) ) ;
#4656 = CIRCLE ( 'NONE', #16284, 3.750000000000000000 ) ;
#4657 = LINE ( 'NONE', #2492, #90 ) ;
#4658 = CARTESIAN_POINT ( 'NONE',  ( -11.67870406890000012, -57.47571038070000782, -20.30949878500000239 ) ) ;
#4659 = AXIS2_PLACEMENT_3D ( 'NONE', #28136, #18697, #3391 ) ;
#4660 = ORIENTED_EDGE ( 'NONE', *, *, #9104, .F. ) ;
#4661 = ADVANCED_FACE ( 'NONE', ( #4632 ), #20430, .T. ) ;
#4662 = DIRECTION ( 'NONE',  ( 0.9704142011833030157, 0.000000000000000000, -0.2414462220490760924 ) ) ;
#4663 = CARTESIAN_POINT ( 'NONE',  ( 15.54119315139999991, -100.8869813350000015, 1.981730678670000190 ) ) ;
#4664 = ORIENTED_EDGE ( 'NONE', *, *, #8307, .T. ) ;
#4665 = LINE ( 'NONE', #8718, #7501 ) ;
#4666 = CARTESIAN_POINT ( 'NONE',  ( 8.916781105359106618, -18.97801339259782338, -18.93583224184311220 ) ) ;
#4667 = ORIENTED_EDGE ( 'NONE', *, *, #12318, .F. ) ;
#4668 = DIRECTION ( 'NONE',  ( -1.000000000000000000, 0.000000000000000000, 1.286327366459999920E-15 ) ) ;
#4669 = CARTESIAN_POINT ( 'NONE',  ( 5.711762562947686028, -93.38554229049410083, -27.07704979681747659 ) ) ;
#4670 = CARTESIAN_POINT ( 'NONE',  ( 8.721287999440001215, -37.33944922460000271, -21.87060590859999820 ) ) ;
#4671 = DIRECTION ( 'NONE',  ( 0.000000000000000000, -1.000000000000000000, 0.000000000000000000 ) ) ;
#4672 = CARTESIAN_POINT ( 'NONE',  ( 4.500000000000000000, -15.00000000000000000, -50.00000000000000000 ) ) ;
#4673 = CARTESIAN_POINT ( 'NONE',  ( 21.47791241899999903, -36.56811125080000835, -7.356933755090000027 ) ) ;
#4674 = VERTEX_POINT ( 'NONE', #28653 ) ;
#4675 = DIRECTION ( 'NONE',  ( -0.8775825618903722036, 0.000000000000000000, 0.4794255386042041156 ) ) ;
#4676 = EDGE_CURVE ( 'NONE', #11154, #2880, #26949, .T. ) ;
#4677 = CARTESIAN_POINT ( 'NONE',  ( -20.41203979210912678, -61.51300819583687485, 12.46450689150019286 ) ) ;
#4678 = CARTESIAN_POINT ( 'NONE',  ( -32.77174709959999888, -74.43710720380001078, -21.60034937849999892 ) ) ;
#4679 = ORIENTED_EDGE ( 'NONE', *, *, #3792, .T. ) ;
#4680 = AXIS2_PLACEMENT_3D ( 'NONE', #2723, #18153, #11577 ) ;
#4681 = DIRECTION ( 'NONE',  ( 0.4794255386042040601, 0.000000000000000000, 0.8775825618903720926 ) ) ;
#4682 = CARTESIAN_POINT ( 'NONE',  ( -17.33149606389999775, -93.33737544240000261, 19.25501164609999805 ) ) ;
#4683 = DIRECTION ( 'NONE',  ( 0.000000000000000000, 1.000000000000000000, 0.000000000000000000 ) ) ;
#4684 = ORIENTED_EDGE ( 'NONE', *, *, #6517, .F. ) ;
#4685 = AXIS2_PLACEMENT_3D ( 'NONE', #16923, #8169, #26522 ) ;
#4686 = CARTESIAN_POINT ( 'NONE',  ( -14.94261203119999948, -100.8733967390000004, 4.897670397449999768 ) ) ;
#4687 = AXIS2_PLACEMENT_3D ( 'NONE', #27950, #7725, #18650 ) ;
#4688 = CARTESIAN_POINT ( 'NONE',  ( 0.3417563417390000469, -101.0151300849999814, -15.63443945619999731 ) ) ;
#4689 = CARTESIAN_POINT ( 'NONE',  ( 9.099148368519999863, -57.44066836780000074, -22.71963871379999844 ) ) ;
#4690 = B_SPLINE_CURVE_WITH_KNOTS ( 'NONE', 3,
 ( #14715, #18059, #17623, #15115, #8576, #26812, #13379, #26961, #6548, #161, #6701, #21993, #17480, #19937, #2483, #26363, #313, #4363, #4503, #9014, #15710, #13528, #22144, #28540, #11340, #20246, #2183, #17920, #15412, #22439, #24620, #1897, #9152 ),
 .UNSPECIFIED., .F., .F.,
 ( 4, 2, 1, 1, 2, 2, 1, 1, 1, 2, 2, 2, 1, 1, 2, 2, 1, 1, 2, 2, 4 ),
 ( 0.000000000000000000, 0.06250000000002969847, 0.09375000000005637157, 0.1093750000000590639, 0.1171875000000546785, 0.1250000000000502931, 0.1875000000001130762, 0.2187500000001388889, 0.2343750000001501854, 0.2421875000001594003, 0.2500000000001686429, 0.3750000000001466050, 0.4375000000001378897, 0.4687500000001335043, 0.4843750000001280087, 0.5000000000001224576, 0.6250000000000865974, 0.6875000000000731637, 0.7187500000000640599, 0.7500000000000549560, 1.000000000000000000 ),
 .UNSPECIFIED. ) ;
#4691 = DIRECTION ( 'NONE',  ( 1.000000000000000000, 0.000000000000000000, 5.551115123129980921E-17 ) ) ;
#4692 = CARTESIAN_POINT ( 'NONE',  ( -11.74918180529999923, -34.66943697800000734, -19.26448814340000126 ) ) ;
#4693 = CARTESIAN_POINT ( 'NONE',  ( 7.040046461240000220, -99.69348480060000384, 15.82639634539999918 ) ) ;
#4694 = DIRECTION ( 'NONE',  ( 1.000000000000000000, 0.000000000000000000, 0.000000000000000000 ) ) ;
#4695 = EDGE_LOOP ( 'NONE', ( #10714, #5228, #22393, #28228 ) ) ;
#4696 = EDGE_CURVE ( 'NONE', #26457, #9687, #17458, .T. ) ;
#4697 = CARTESIAN_POINT ( 'NONE',  ( 13.12517053680000068, -91.50000000000000000, 27.53143473160000099 ) ) ;
#4698 = CARTESIAN_POINT ( 'NONE',  ( 24.58030493329999899, -18.50000000000000000, 2.442848308399999890 ) ) ;
#4699 = CARTESIAN_POINT ( 'NONE',  ( 12.46091330099999972, -98.29703159100000676, 14.48139617630000053 ) ) ;
#4700 = AXIS2_PLACEMENT_3D ( 'NONE', #3673, #10484, #8050 ) ;
#4701 = CARTESIAN_POINT ( 'NONE',  ( 7.279135155890000597, -73.90050421709999284, 39.59102417159999021 ) ) ;
#4702 = CARTESIAN_POINT ( 'NONE',  ( 26.57391653120000186, -92.50000460620000808, 13.43926559110000163 ) ) ;
#4703 = VECTOR ( 'NONE', #9577, 1000.000000000000000 ) ;
#4704 = AXIS2_PLACEMENT_3D ( 'NONE', #1903, #25432, #5460 ) ;
#4705 = CARTESIAN_POINT ( 'NONE',  ( 10.56566109427459033, -96.61062616328538866, -18.41854727118479218 ) ) ;
#4706 = CARTESIAN_POINT ( 'NONE',  ( -6.976086355399999661, -101.3852859389999992, 14.39181666049999997 ) ) ;
#4707 = ORIENTED_EDGE ( 'NONE', *, *, #16495, .F. ) ;
#4708 = CARTESIAN_POINT ( 'NONE',  ( 0.000000000000000000, -40.00000000000000000, 0.000000000000000000 ) ) ;
#4709 = DIRECTION ( 'NONE',  ( 1.000000000000000000, 0.000000000000000000, 0.000000000000000000 ) ) ;
#4710 = CARTESIAN_POINT ( 'NONE',  ( 8.704479342339999093, -36.45005858900000106, -21.20784114439999968 ) ) ;
#4711 = EDGE_CURVE ( 'NONE', #20961, #14272, #2295, .T. ) ;
#4712 = CARTESIAN_POINT ( 'NONE',  ( 0.000000000000000000, -57.47855601759999900, 0.000000000000000000 ) ) ;
#4713 = CARTESIAN_POINT ( 'NONE',  ( 7.501173096960000564, -99.48532946420000656, 15.95771025049999992 ) ) ;
#4714 = DIRECTION ( 'NONE',  ( 0.000000000000000000, 1.000000000000000000, 0.000000000000000000 ) ) ;
#4715 = FACE_OUTER_BOUND ( 'NONE', #9301, .T. ) ;
#4716 = CARTESIAN_POINT ( 'NONE',  ( -2.585842044862892042, -19.48733830549529600, -23.57049848989026231 ) ) ;
#4717 = ORIENTED_EDGE ( 'NONE', *, *, #19026, .F. ) ;
#4718 = CARTESIAN_POINT ( 'NONE',  ( 11.43994069400000058, -100.8816835080000089, -10.88980376029999952 ) ) ;
#4719 = CARTESIAN_POINT ( 'NONE',  ( -13.37241048499999962, -18.62107966670000181, 19.38866880850000030 ) ) ;
#4720 = CARTESIAN_POINT ( 'NONE',  ( 15.52051803399669261, -95.02776861797826768, 17.29095834261395126 ) ) ;
#4721 = CIRCLE ( 'NONE', #21026, 18.64285714289999873 ) ;
#4722 = DIRECTION ( 'NONE',  ( 1.000000000000000000, 0.000000000000000000, 0.000000000000000000 ) ) ;
#4723 = B_SPLINE_CURVE_WITH_KNOTS ( 'NONE', 5,
 ( #21148, #1330, #16616, #10174, #5268, #16330 ),
 .UNSPECIFIED., .F., .F.,
 ( 6, 6 ),
 ( 0.000000000000000000, 1.000000000000000000 ),
 .UNSPECIFIED. ) ;
#4724 = CARTESIAN_POINT ( 'NONE',  ( 9.356041104380000917, -74.50000000000000000, -37.60355029590000697 ) ) ;
#4725 = CYLINDRICAL_SURFACE ( 'NONE', #23103, 11.00000000000000000 ) ;
#4726 = CARTESIAN_POINT ( 'NONE',  ( 15.50925563669999896, -100.9197081840000010, 1.894558565230000102 ) ) ;
#4727 = CARTESIAN_POINT ( 'NONE',  ( 22.18949969423676905, -94.10917102494428832, 13.31178859376489321 ) ) ;
#4728 = AXIS2_PLACEMENT_3D ( 'NONE', #27616, #19130, #25418 ) ;
#4729 = EDGE_LOOP ( 'NONE', ( #25908, #1629, #10470, #27204 ) ) ;
#4730 = VECTOR ( 'NONE', #19381, 1000.000000000000000 ) ;
#4731 = CARTESIAN_POINT ( 'NONE',  ( -29.75530570606409597, -92.89593097428694080, 6.698644383117053458 ) ) ;
#4732 = AXIS2_PLACEMENT_3D ( 'NONE', #171, #17926, #26817 ) ;
#4733 = CARTESIAN_POINT ( 'NONE',  ( 7.976137737220000190, -101.5137793180000045, 13.98721220989999914 ) ) ;
#4734 = ORIENTED_EDGE ( 'NONE', *, *, #27565, .F. ) ;
#4735 = CARTESIAN_POINT ( 'NONE',  ( -12.24787727680000060, -65.07443125830000952, 21.96585809910000009 ) ) ;
#4736 = CARTESIAN_POINT ( 'NONE',  ( -13.48313256510000002, -64.78279493179998383, 21.61455522920000050 ) ) ;
#4737 = DIRECTION ( 'NONE',  ( 0.000000000000000000, 1.000000000000000000, 0.000000000000000000 ) ) ;
#4738 = CARTESIAN_POINT ( 'NONE',  ( -2.495716009669999735, -52.58489974409944523, -24.49317771889998241 ) ) ;
#4739 = ADVANCED_FACE ( 'NONE', ( #26343 ), #13089, .T. ) ;
#4740 = CARTESIAN_POINT ( 'NONE',  ( 22.17953377930000158, -65.07443093669999712, 11.85657293289999892 ) ) ;
#4741 = EDGE_CURVE ( 'NONE', #17152, #18837, #7869, .T. ) ;
#4742 = AXIS2_PLACEMENT_3D ( 'NONE', #4016, #26761, #4157 ) ;
#4743 = ORIENTED_EDGE ( 'NONE', *, *, #3582, .T. ) ;
#4744 = AXIS2_PLACEMENT_3D ( 'NONE', #17099, #23661, #12991 ) ;
#4745 = CARTESIAN_POINT ( 'NONE',  ( -7.255215663259999559, -74.34471143260000758, -40.30304758909999663 ) ) ;
#4746 = LINE ( 'NONE', #2575, #12542 ) ;
#4747 = CARTESIAN_POINT ( 'NONE',  ( -15.35950681959999997, -99.56347590750000620, -8.501124659940000328 ) ) ;
#4748 = ORIENTED_EDGE ( 'NONE', *, *, #2168, .F. ) ;
#4749 = EDGE_CURVE ( 'NONE', #14143, #16936, #12472, .T. ) ;
#4750 = AXIS2_PLACEMENT_3D ( 'NONE', #1174, #3339, #14405 ) ;
#4751 = CARTESIAN_POINT ( 'NONE',  ( -13.13725193384587264, -67.22652123493047327, -22.58921519140665168 ) ) ;
#4752 = EDGE_CURVE ( 'NONE', #25977, #9315, #21527, .T. ) ;
#4753 = DIRECTION ( 'NONE',  ( -0.3390050494208429743, 0.7071067811866730279, -0.6205445805637129775 ) ) ;
#4754 = B_SPLINE_CURVE_WITH_KNOTS ( 'NONE', 3,
 ( #1814, #13003, #21627, #1963, #15475, #23810 ),
 .UNSPECIFIED., .F., .F.,
 ( 4, 2, 4 ),
 ( 0.000000000000000000, 0.5000000000000000000, 1.000000000000000000 ),
 .UNSPECIFIED. ) ;
#4755 = DIRECTION ( 'NONE',  ( 0.000000000000000000, -1.000000000000000000, 0.000000000000000000 ) ) ;
#4756 = DIRECTION ( 'NONE',  ( 1.000000000000000000, 0.000000000000000000, 0.000000000000000000 ) ) ;
#4757 = DIRECTION ( 'NONE',  ( 1.000000000000000000, 0.000000000000000000, 0.000000000000000000 ) ) ;
#4758 = CARTESIAN_POINT ( 'NONE',  ( -7.218875474177550267, -73.62261561668539400, -39.32889484839753180 ) ) ;
#4759 = CARTESIAN_POINT ( 'NONE',  ( 20.91100902960000241, -19.47458110719999880, 9.394602247639998183 ) ) ;
#4760 = CARTESIAN_POINT ( 'NONE',  ( -41.45000000000000284, -65.14977478849999670, 2.857883832489999776 ) ) ;
#4761 = CARTESIAN_POINT ( 'NONE',  ( -15.64456437664894750, -99.93376895843553598, 6.429786443641783755 ) ) ;
#4762 = B_SPLINE_SURFACE_WITH_KNOTS ( 'NONE', 5, 5, ( 
 ( #22586, #9302, #18203, #24911, #22876, #16007 ),
 ( #15707, #9597, #310, #4943, #25056, #13824 ),
 ( #9012, #20243, #2769, #24616, #27390, #20535 ),
 ( #11179, #15858, #13972, #5240, #7436, #606 ),
 ( #16298, #25208, #20094, #9449, #6994, #18356 ),
 ( #158, #4650, #16150, #13526, #22437, #2480 ) ),
 .UNSPECIFIED., .F., .F., .F.,
 ( 6, 6 ),
 ( 6, 6 ),
 ( 14.35373998510000071, 23.44689954260000064 ),
 ( 0.000000000000000000, 0.5000000000000000000 ),
 .UNSPECIFIED. ) ;
#4763 = VERTEX_POINT ( 'NONE', #7568 ) ;
#4764 = CARTESIAN_POINT ( 'NONE',  ( -12.22902281400000035, -69.69726684059999400, -24.77074626769999810 ) ) ;
#4765 = CARTESIAN_POINT ( 'NONE',  ( 0.000000000000000000, -33.79999999999999716, 0.000000000000000000 ) ) ;
#4766 = CARTESIAN_POINT ( 'NONE',  ( -13.02860857159999952, -99.94751438429999268, -11.16201040320000004 ) ) ;
#4767 = CARTESIAN_POINT ( 'NONE',  ( 20.23144668435722338, -19.46809228182657492, 9.669420246545856301 ) ) ;
#4768 = CARTESIAN_POINT ( 'NONE',  ( -13.24425460951195888, -99.76647888979881884, -11.15875677615296091 ) ) ;
#4769 = VERTEX_POINT ( 'NONE', #9862 ) ;
#4770 = CIRCLE ( 'NONE', #21066, 32.39999999999999858 ) ;
#4771 = B_SPLINE_CURVE_WITH_KNOTS ( 'NONE', 3,
 ( #6546, #10881, #26361, #19791 ),
 .UNSPECIFIED., .F., .F.,
 ( 4, 4 ),
 ( 0.000000000000000000, 1.000000000000000000 ),
 .UNSPECIFIED. ) ;
#4772 = CARTESIAN_POINT ( 'NONE',  ( 26.47131973888236800, -92.75430643216988358, -15.14997898769894036 ) ) ;
#4773 = EDGE_LOOP ( 'NONE', ( #28293, #9989 ) ) ;
#4774 = AXIS2_PLACEMENT_3D ( 'NONE', #7797, #18586, #16385 ) ;
#4775 = DIRECTION ( 'NONE',  ( 1.000000000000000000, 0.000000000000000000, 0.000000000000000000 ) ) ;
#4776 = CARTESIAN_POINT ( 'NONE',  ( -4.062581167790000336, -98.51736893940000073, 19.25659066309999901 ) ) ;
#4777 = CARTESIAN_POINT ( 'NONE',  ( 8.007555411949999424, -93.15603699990001019, 27.33235638589999894 ) ) ;
#4778 = ORIENTED_EDGE ( 'NONE', *, *, #20355, .F. ) ;
#4779 = ADVANCED_FACE ( 'NONE', ( #16428 ), #9716, .T. ) ;
#4780 = ORIENTED_EDGE ( 'NONE', *, *, #10822, .F. ) ;
#4781 = DIRECTION ( 'NONE',  ( 0.000000000000000000, 1.000000000000000000, 0.000000000000000000 ) ) ;
#4782 = CARTESIAN_POINT ( 'NONE',  ( 20.62093289109999716, -94.45168212990000711, 13.94874876430000121 ) ) ;
#4783 = CARTESIAN_POINT ( 'NONE',  ( 46.85366533689999358, -73.91963657849998981, -2.428543975460000226 ) ) ;
#4784 = VERTEX_POINT ( 'NONE', #6974 ) ;
#4785 = CARTESIAN_POINT ( 'NONE',  ( -42.63274768570000361, -69.50000000000000000, -1.438276615809999992 ) ) ;
#4786 = CARTESIAN_POINT ( 'NONE',  ( -22.07482501520000184, -79.88234130290000223, -32.63328169969999948 ) ) ;
#4787 = ADVANCED_FACE ( 'NONE', ( #21103 ), #14390, .F. ) ;
#4788 = CIRCLE ( 'NONE', #16892, 3.750000000000000000 ) ;
#4789 = CARTESIAN_POINT ( 'NONE',  ( 12.19134911989999814, -101.1716782170000073, -9.946103829120000128 ) ) ;
#4790 = DIRECTION ( 'NONE',  ( 0.000000000000000000, 1.000000000000000000, 0.000000000000000000 ) ) ;
#4791 = AXIS2_PLACEMENT_3D ( 'NONE', #7460, #23043, #11943 ) ;
#4792 = CARTESIAN_POINT ( 'NONE',  ( -24.07228054242398230, -94.80026864433543210, -4.144187258122226325 ) ) ;
#4793 = ORIENTED_EDGE ( 'NONE', *, *, #17906, .T. ) ;
#4794 = FACE_OUTER_BOUND ( 'NONE', #22376, .T. ) ;
#4795 = CARTESIAN_POINT ( 'NONE',  ( 13.80769401629999926, -99.88067631459999518, -10.49277699589999813 ) ) ;
#4796 = CARTESIAN_POINT ( 'NONE',  ( -39.59102417159999021, -73.90050421709999284, 7.279135155890000597 ) ) ;
#4797 = CARTESIAN_POINT ( 'NONE',  ( -22.00249031559999935, -74.50000000000000000, -32.67527180329999936 ) ) ;
#4798 = DIRECTION ( 'NONE',  ( 1.000000000000000000, 0.000000000000000000, 0.000000000000000000 ) ) ;
#4799 = FACE_OUTER_BOUND ( 'NONE', #13249, .T. ) ;
#4800 = CARTESIAN_POINT ( 'NONE',  ( -7.485155838150649110, -73.99989100306002854, 38.96201482635396474 ) ) ;
#4801 = CARTESIAN_POINT ( 'NONE',  ( 31.00000000000000000, -15.00000000000000000, 4.500000000000000000 ) ) ;
#4802 = ORIENTED_EDGE ( 'NONE', *, *, #22374, .F. ) ;
#4803 = DIRECTION ( 'NONE',  ( 0.000000000000000000, -1.000000000000000000, 0.000000000000000000 ) ) ;
#4804 = AXIS2_PLACEMENT_3D ( 'NONE', #16954, #25845, #5867 ) ;
#4805 = CARTESIAN_POINT ( 'NONE',  ( 22.87354612120000041, -62.62089253239999920, 10.49332266949999948 ) ) ;
#4806 = FACE_OUTER_BOUND ( 'NONE', #13223, .T. ) ;
#4807 = CARTESIAN_POINT ( 'NONE',  ( 15.67135797424042742, -101.4728631013787208, 3.842886462708210438 ) ) ;
#4808 = CARTESIAN_POINT ( 'NONE',  ( 0.000000000000000000, -19.40000000000000213, 0.000000000000000000 ) ) ;
#4809 = ORIENTED_EDGE ( 'NONE', *, *, #27665, .T. ) ;
#4810 = CARTESIAN_POINT ( 'NONE',  ( 47.25120111029999492, -79.32896547530000930, -0.9107464912380001110 ) ) ;
#4811 = PRODUCT_DEFINITION_CONTEXT ( 'detailed design', #10323, 'design' ) ;
#4812 = CARTESIAN_POINT ( 'NONE',  ( -11.84069971089999918, -64.35840483370000698, -23.45279569499999894 ) ) ;
#4813 = AXIS2_PLACEMENT_3D ( 'NONE', #183, #4384, #22460 ) ;
#4814 = DIRECTION ( 'NONE',  ( -0.7071067811865475727, 0.000000000000000000, -0.7071067811865475727 ) ) ;
#4815 = DIRECTION ( 'NONE',  ( 0.000000000000000000, -1.000000000000000000, 0.000000000000000000 ) ) ;
#4816 = EDGE_LOOP ( 'NONE', ( #20575, #7039 ) ) ;
#4817 = ADVANCED_FACE ( 'NONE', ( #16572 ), #12187, .F. ) ;
#4818 = CARTESIAN_POINT ( 'NONE',  ( 40.00000000000000000, -84.00000000000000000, 0.000000000000000000 ) ) ;
#4819 = CARTESIAN_POINT ( 'NONE',  ( 46.80987811986599212, -73.90819598650089972, -2.489252664572485951 ) ) ;
#4820 = ORIENTED_EDGE ( 'NONE', *, *, #16351, .T. ) ;
#4821 = CARTESIAN_POINT ( 'NONE',  ( 27.75394116159999669, -74.50000000000000000, -27.75394116159999669 ) ) ;
#4822 = CARTESIAN_POINT ( 'NONE',  ( -17.94180966909999597, -19.50000000000000000, 18.81731824139999887 ) ) ;
#4823 = EDGE_LOOP ( 'NONE', ( #12314, #26010, #19397, #24221 ) ) ;
#4824 = DIRECTION ( 'NONE',  ( 1.000000000000000000, 0.000000000000000000, 0.000000000000000000 ) ) ;
#4825 = EDGE_CURVE ( 'NONE', #3611, #9035, #5423, .T. ) ;
#4826 = AXIS2_PLACEMENT_3D ( 'NONE', #7779, #10073, #23636 ) ;
#4827 = CARTESIAN_POINT ( 'NONE',  ( 8.153295725933123350, -94.16483583575367788, -24.44841081015503192 ) ) ;
#4828 = CARTESIAN_POINT ( 'NONE',  ( 9.014522480169999241, -36.52810941340000284, -21.48399575520000226 ) ) ;
#4829 = CARTESIAN_POINT ( 'NONE',  ( -41.75000000000000000, -63.17361819574031045, 2.263739386364747919 ) ) ;
#4830 = CARTESIAN_POINT ( 'NONE',  ( -9.489637567029999943, -18.50000000000000000, -21.46212729140000164 ) ) ;
#4831 = CARTESIAN_POINT ( 'NONE',  ( 21.53322619567358487, -37.52465077453045694, -7.784903219023103560 ) ) ;
#4832 = EDGE_LOOP ( 'NONE', ( #18242, #16244, #22403, #12092 ) ) ;
#4833 = CARTESIAN_POINT ( 'NONE',  ( 9.017793344559999369, -92.49999846069999876, -27.43401283590000261 ) ) ;
#4834 = CARTESIAN_POINT ( 'NONE',  ( -38.19683097078898015, -65.73348302053989300, -1.252585022352845412 ) ) ;
#4835 = CARTESIAN_POINT ( 'NONE',  ( -12.77311630576821244, -92.58347372263071406, 27.69652610236371970 ) ) ;
#4836 = ORIENTED_EDGE ( 'NONE', *, *, #17334, .T. ) ;
#4837 = FACE_OUTER_BOUND ( 'NONE', #3336, .T. ) ;
#4838 = CARTESIAN_POINT ( 'NONE',  ( -7.215414233289999757, -80.50000000000000000, 40.70731707320000226 ) ) ;
#4839 = CARTESIAN_POINT ( 'NONE',  ( -21.66710847110000060, -65.28157844300000079, 15.85023555240000093 ) ) ;
#4840 = ORIENTED_EDGE ( 'NONE', *, *, #19218, .T. ) ;
#4841 = CARTESIAN_POINT ( 'NONE',  ( -17.59164495649999793, -96.97509177549999038, 11.15485559729999920 ) ) ;
#4842 = EDGE_CURVE ( 'NONE', #18987, #25992, #27791, .T. ) ;
#4843 = CARTESIAN_POINT ( 'NONE',  ( -19.61616312839999665, -45.99906616869999709, 11.93235103359999982 ) ) ;
#4844 = CARTESIAN_POINT ( 'NONE',  ( 26.07817510496859725, -74.32881829746334290, -29.29368945734479013 ) ) ;
#4845 = CARTESIAN_POINT ( 'NONE',  ( -12.47290128200000048, -69.87861801290000585, -24.46965308400000083 ) ) ;
#4846 = CARTESIAN_POINT ( 'NONE',  ( -14.77602055539237647, -74.24330531883769879, 36.28595032296689027 ) ) ;
#4847 = CIRCLE ( 'NONE', #14145, 1.499999999999999556 ) ;
#4848 = DIRECTION ( 'NONE',  ( 0.7071067811865492381, 0.000000000000000000, -0.7071067811865457964 ) ) ;
#4849 = AXIS2_PLACEMENT_3D ( 'NONE', #409, #6952, #15213 ) ;
#4850 = EDGE_LOOP ( 'NONE', ( #24237, #333, #25194, #7191 ) ) ;
#4851 = ADVANCED_FACE ( 'NONE', ( #12596 ), #5909, .T. ) ;
#4852 = DIRECTION ( 'NONE',  ( -0.3928703629870110570, 0.000000000000000000, 0.9195938657290262386 ) ) ;
#4853 = CARTESIAN_POINT ( 'NONE',  ( 24.18500510740000209, -18.50000000000000000, 2.499651262099999993 ) ) ;
#4854 = CARTESIAN_POINT ( 'NONE',  ( 17.20775814350000132, -95.72998475950001307, 14.36350897220000000 ) ) ;
#4855 = ORIENTED_EDGE ( 'NONE', *, *, #19435, .F. ) ;
#4856 = AXIS2_PLACEMENT_3D ( 'NONE', #23600, #18827, #21417 ) ;
#4857 = CARTESIAN_POINT ( 'NONE',  ( 7.305170733980000719, -74.19145785139998850, 39.89387480210000092 ) ) ;
#4858 = CARTESIAN_POINT ( 'NONE',  ( 24.66732901470000172, -92.51556042380001088, 14.76695160569999921 ) ) ;
#4859 = EDGE_CURVE ( 'NONE', #7605, #3896, #21509, .T. ) ;
#4860 = CARTESIAN_POINT ( 'NONE',  ( 22.36835622256649714, -19.46749651865001596, 0.6186015604048864525 ) ) ;
#4861 = CARTESIAN_POINT ( 'NONE',  ( 8.971088436049999615, -36.01992746820000235, -20.53904558130000169 ) ) ;
#4862 = CARTESIAN_POINT ( 'NONE',  ( 8.542193844259857727, -19.47739189591211328, -20.07101182275077633 ) ) ;
#4863 = ORIENTED_EDGE ( 'NONE', *, *, #21508, .F. ) ;
#4864 = CARTESIAN_POINT ( 'NONE',  ( 7.181688671299999882, -99.92967573500000356, 15.80534928199999989 ) ) ;
#4865 = CARTESIAN_POINT ( 'NONE',  ( 23.56381625550000081, -19.17416318749999959, 1.511209194469999906 ) ) ;
#4866 = DIRECTION ( 'NONE',  ( 0.4794255386042041156, 0.000000000000000000, 0.8775825618903722036 ) ) ;
#4867 = VECTOR ( 'NONE', #13927, 1000.000000000000000 ) ;
#4868 = CARTESIAN_POINT ( 'NONE',  ( -1.557368374968634228, -19.46665351424891455, -22.24853037986929394 ) ) ;
#4869 = FACE_OUTER_BOUND ( 'NONE', #2326, .T. ) ;
#4870 = CARTESIAN_POINT ( 'NONE',  ( -13.09065259650000002, -19.17416291640000026, 19.65126003909999852 ) ) ;
#4871 = CARTESIAN_POINT ( 'NONE',  ( -41.00000000000000000, -84.00000000000000000, 10.20110288159999890 ) ) ;
#4872 = CARTESIAN_POINT ( 'NONE',  ( -38.38199864144505113, -63.05366291736240214, -2.876043459049374196 ) ) ;
#4873 = EDGE_CURVE ( 'NONE', #15079, #7833, #28657, .T. ) ;
#4874 = DIRECTION ( 'NONE',  ( 1.000000000000000000, 0.000000000000000000, 0.000000000000000000 ) ) ;
#4875 = CIRCLE ( 'NONE', #25361, 3.000000000000000000 ) ;
#4876 = CARTESIAN_POINT ( 'NONE',  ( -17.80822692750000158, -111.0000000000000000, -18.25149456069999943 ) ) ;
#4877 = DIRECTION ( 'NONE',  ( 1.000000000000000000, 0.000000000000000000, 0.000000000000000000 ) ) ;
#4878 = VERTEX_POINT ( 'NONE', #9349 ) ;
#4879 = CARTESIAN_POINT ( 'NONE',  ( 36.71193690820000199, -74.86352340930001503, -14.74418008200000152 ) ) ;
#4880 = AXIS2_PLACEMENT_3D ( 'NONE', #2453, #22404, #4775 ) ;
#4881 = CARTESIAN_POINT ( 'NONE',  ( 7.787105047099999844, -101.3792338629999961, 13.97258517809999923 ) ) ;
#4882 = EDGE_CURVE ( 'NONE', #8136, #6525, #19944, .T. ) ;
#4883 = CARTESIAN_POINT ( 'NONE',  ( -12.07243358760000085, -67.46050599719998786, -24.77970463289999969 ) ) ;
#4884 = CARTESIAN_POINT ( 'NONE',  ( -44.38791280949999418, -63.50000000000000000, -2.397127693020000283 ) ) ;
#4885 = DIRECTION ( 'NONE',  ( 1.000000000000000000, 0.000000000000000000, 0.000000000000000000 ) ) ;
#4886 = CARTESIAN_POINT ( 'NONE',  ( 20.85226889450000343, -36.17942473059999742, -9.018047964759999147 ) ) ;
#4887 = CARTESIAN_POINT ( 'NONE',  ( -1.456904695350001111, -52.62618816489944606, -23.34673678599997970 ) ) ;
#4888 = CARTESIAN_POINT ( 'NONE',  ( 20.77909565649999735, -36.00000000010000178, -9.444780804769999705 ) ) ;
#4889 = CARTESIAN_POINT ( 'NONE',  ( 16.52049151459999976, -99.72202992580000114, 4.688718860289999846 ) ) ;
#4890 = VERTEX_POINT ( 'NONE', #19983 ) ;
#4891 = CARTESIAN_POINT ( 'NONE',  ( 21.49478534619999692, -36.56947956670000366, -7.151043357429999858 ) ) ;
#4892 = CARTESIAN_POINT ( 'NONE',  ( -21.99303270440000446, -95.76596938280000870, -5.803739253210000726 ) ) ;
#4893 = ORIENTED_EDGE ( 'NONE', *, *, #20203, .F. ) ;
#4894 = CARTESIAN_POINT ( 'NONE',  ( 23.14416696340000001, -57.40875702419999982, 10.37855830930000067 ) ) ;
#4895 = CARTESIAN_POINT ( 'NONE',  ( 0.000000000000000000, -15.50000000000000000, 0.000000000000000000 ) ) ;
#4896 = DIRECTION ( 'NONE',  ( 0.4794255386042059475, 0.000000000000000000, 0.8775825618903710934 ) ) ;
#4897 = AXIS2_PLACEMENT_3D ( 'NONE', #16314, #13989, #9316 ) ;
#4898 = CARTESIAN_POINT ( 'NONE',  ( -11.89545460579999947, -101.2530993010000060, -9.453770335970000716 ) ) ;
#4899 = CARTESIAN_POINT ( 'NONE',  ( -7.249276399919747149, -74.06318173121573523, -40.12703402648163831 ) ) ;
#4900 = DIRECTION ( 'NONE',  ( 1.000000000000000000, 0.000000000000000000, 0.000000000000000000 ) ) ;
#4901 = CARTESIAN_POINT ( 'NONE',  ( 10.64645172839999887, -72.61900946069999918, -26.72437960700000303 ) ) ;
#4902 = CARTESIAN_POINT ( 'NONE',  ( -16.50266362683683141, -98.65920929149453400, 8.461970372646858252 ) ) ;
#4903 = EDGE_LOOP ( 'NONE', ( #11305, #7178, #27175, #28486 ) ) ;
#4904 = CARTESIAN_POINT ( 'NONE',  ( -12.79457676070000183, -70.02558174150000525, -24.23940011709999709 ) ) ;
#4905 = DIRECTION ( 'NONE',  ( 0.4794255386042028944, 0.000000000000000000, -0.8775825618903727587 ) ) ;
#4906 = CARTESIAN_POINT ( 'NONE',  ( 7.635702898730000854, -101.6454117330000031, 14.06304778130000166 ) ) ;
#4907 = PRODUCT_RELATED_PRODUCT_CATEGORY ( 'part', '', ( #26438 ) ) ;
#4908 = CARTESIAN_POINT ( 'NONE',  ( 21.27121383927310205, -19.48034373448365741, 9.460266570831914024 ) ) ;
#4909 = CARTESIAN_POINT ( 'NONE',  ( 22.54638839685503271, -60.33833132835033553, -7.163837719818888061 ) ) ;
#4910 = ORIENTED_EDGE ( 'NONE', *, *, #27863, .F. ) ;
#4911 = EDGE_CURVE ( 'NONE', #23865, #21973, #28712, .T. ) ;
#4912 = CARTESIAN_POINT ( 'NONE',  ( 26.89630156707283959, -92.56492639279250056, -14.38221850968363746 ) ) ;
#4913 = ORIENTED_EDGE ( 'NONE', *, *, #11083, .F. ) ;
#4914 = EDGE_CURVE ( 'NONE', #4550, #19124, #5995, .T. ) ;
#4915 = EDGE_CURVE ( 'NONE', #8492, #24436, #5537, .T. ) ;
#4916 = CIRCLE ( 'NONE', #18889, 30.50000000000000000 ) ;
#4917 = DIRECTION ( 'NONE',  ( 1.000000000000000000, 0.000000000000000000, 0.000000000000000000 ) ) ;
#4918 = DIRECTION ( 'NONE',  ( 0.000000000000000000, -1.000000000000000000, 0.000000000000000000 ) ) ;
#4919 = CARTESIAN_POINT ( 'NONE',  ( 7.995248799109998750, -92.98123155529999906, 27.31123713640000261 ) ) ;
#4920 = ORIENTED_EDGE ( 'NONE', *, *, #8637, .T. ) ;
#4921 = ORIENTED_EDGE ( 'NONE', *, *, #5667, .T. ) ;
#4922 = CARTESIAN_POINT ( 'NONE',  ( 36.24656966590000451, -75.00000018780001199, -15.05817676390000059 ) ) ;
#4923 = DIRECTION ( 'NONE',  ( 1.000000000000000000, 0.000000000000000000, 0.000000000000000000 ) ) ;
#4924 = CARTESIAN_POINT ( 'NONE',  ( 47.16888057639999943, -74.56821146769999586, -1.104573556149999858 ) ) ;
#4925 = ORIENTED_EDGE ( 'NONE', *, *, #2251, .F. ) ;
#4926 = LINE ( 'NONE', #27369, #23411 ) ;
#4927 = ORIENTED_EDGE ( 'NONE', *, *, #16564, .T. ) ;
#4928 = DIRECTION ( 'NONE',  ( 0.4794255386042036715, 0.000000000000000000, 0.8775825618903722036 ) ) ;
#4929 = CARTESIAN_POINT ( 'NONE',  ( 12.36959650760000073, -101.3256027139999986, -10.00103415339999913 ) ) ;
#4930 = CARTESIAN_POINT ( 'NONE',  ( -14.67423319995313413, -93.10940799664778922, -23.67382460028223434 ) ) ;
#4931 = ORIENTED_EDGE ( 'NONE', *, *, #23143, .T. ) ;
#4932 = CARTESIAN_POINT ( 'NONE',  ( 36.50549978619999791, -74.62369759450000117, -14.71598446109999969 ) ) ;
#4933 = CARTESIAN_POINT ( 'NONE',  ( -17.03413894869999723, -99.61736770250000461, 3.268853260370000235 ) ) ;
#4934 = CARTESIAN_POINT ( 'NONE',  ( 40.00000000000000000, -74.00000000000000000, 2.009834509230000106E-15 ) ) ;
#4935 = CARTESIAN_POINT ( 'NONE',  ( -21.99985828019999801, -74.00000000000000000, -31.89935321680000158 ) ) ;
#4936 = VERTEX_POINT ( 'NONE', #11522 ) ;
#4937 = B_SPLINE_CURVE_WITH_KNOTS ( 'NONE', 3,
 ( #2025, #17605, #15389, #2167 ),
 .UNSPECIFIED., .F., .F.,
 ( 4, 4 ),
 ( 0.000000000000000000, 1.000000000000000000 ),
 .UNSPECIFIED. ) ;
#4938 = CARTESIAN_POINT ( 'NONE',  ( -43.20000000000000284, -65.00000000000000000, -0.1732050807570000017 ) ) ;
#4939 = CARTESIAN_POINT ( 'NONE',  ( -7.499802406392214849, -73.99986890635469194, 38.92495601869831034 ) ) ;
#4940 = CARTESIAN_POINT ( 'NONE',  ( -18.23016591169999856, -18.61940624670000233, 13.57443799729999867 ) ) ;
#4941 = EDGE_LOOP ( 'NONE', ( #5657, #20805, #20571, #19479 ) ) ;
#4942 = EDGE_CURVE ( 'NONE', #21621, #22807, #8773, .T. ) ;
#4943 = CARTESIAN_POINT ( 'NONE',  ( -11.89700623620000108, -93.14241133300001252, -23.62892427899999959 ) ) ;
#4944 = CARTESIAN_POINT ( 'NONE',  ( 23.56050310359999855, -94.79581646409999962, -2.314011072670000058 ) ) ;
#4945 = DIRECTION ( 'NONE',  ( 0.4794255386042036715, 0.000000000000000000, 0.8775825618903724257 ) ) ;
#4946 = CARTESIAN_POINT ( 'NONE',  ( 15.61464033245285599, -101.6297509123138525, 3.556724360410273178 ) ) ;
#4947 = CARTESIAN_POINT ( 'NONE',  ( 28.63360765790000073, -72.82938648530000592, 1.697648101029999967 ) ) ;
#4948 = ORIENTED_EDGE ( 'NONE', *, *, #22750, .F. ) ;
#4949 = CARTESIAN_POINT ( 'NONE',  ( 47.25000000000000000, -79.00000000000000000, -7.713829575100000215E-13 ) ) ;
#4950 = AXIS2_PLACEMENT_3D ( 'NONE', #19829, #17808, #22178 ) ;
#4951 = ADVANCED_FACE ( 'NONE', ( #24663 ), #2187, .T. ) ;
#4952 = CARTESIAN_POINT ( 'NONE',  ( -12.00178822160000003, -62.10499660389999832, -20.82579118980000032 ) ) ;
#4953 = CARTESIAN_POINT ( 'NONE',  ( 26.98670340789999855, -72.82938977469999031, -9.720255250700001071 ) ) ;
#4954 = CARTESIAN_POINT ( 'NONE',  ( 11.66718683064264361, -93.00000367782563160, 27.62038300901093280 ) ) ;
#4955 = ORIENTED_EDGE ( 'NONE', *, *, #17035, .F. ) ;
#4956 = DIRECTION ( 'NONE',  ( 1.000000000000000000, 0.000000000000000000, 0.000000000000000000 ) ) ;
#4957 = CARTESIAN_POINT ( 'NONE',  ( -41.75000000000000000, -65.31510159580000163, -2.337827133099999788 ) ) ;
#4958 = ORIENTED_EDGE ( 'NONE', *, *, #14386, .T. ) ;
#4959 = CARTESIAN_POINT ( 'NONE',  ( 9.279094190537668041, -98.48918237499029260, 16.48187022330440499 ) ) ;
#4960 = ORIENTED_EDGE ( 'NONE', *, *, #3856, .F. ) ;
#4961 = CARTESIAN_POINT ( 'NONE',  ( -7.215414233289999757, -82.25000000000000000, -40.70731707320000226 ) ) ;
#4962 = CARTESIAN_POINT ( 'NONE',  ( 19.55068592539999983, -35.72724453810000256, -9.038647860560001135 ) ) ;
#4963 = CARTESIAN_POINT ( 'NONE',  ( -27.33230668875999925, -92.65509297689254709, -4.521833498730020828 ) ) ;
#4964 = CARTESIAN_POINT ( 'NONE',  ( -20.20541094980000096, -94.98812148390000232, 12.40015412250000004 ) ) ;
#4965 = CARTESIAN_POINT ( 'NONE',  ( -18.84946647679999998, -97.93129755900000077, 6.692285885629999598 ) ) ;
#4966 = CARTESIAN_POINT ( 'NONE',  ( -15.50938051129999984, -101.1889999979999999, 4.855933523060000034 ) ) ;
#4967 = CYLINDRICAL_SURFACE ( 'NONE', #7879, 2.999999999999996447 ) ;
#4968 = VERTEX_POINT ( 'NONE', #232 ) ;
#4969 = CARTESIAN_POINT ( 'NONE',  ( 13.12743937220000134, -94.59276479679999738, -19.84843662619999805 ) ) ;
#4970 = CARTESIAN_POINT ( 'NONE',  ( -37.95315413403665872, -65.71452780515592451, -0.8766092144919545026 ) ) ;
#4971 = CARTESIAN_POINT ( 'NONE',  ( 40.08893529097915120, -74.03750509247994671, 7.249551406115140928 ) ) ;
#4972 = ORIENTED_EDGE ( 'NONE', *, *, #10120, .T. ) ;
#4973 = DIRECTION ( 'NONE',  ( 1.000000000000000000, 0.000000000000000000, 0.000000000000000000 ) ) ;
#4974 = CARTESIAN_POINT ( 'NONE',  ( 0.000000000000000000, -84.75000000000000000, 0.000000000000000000 ) ) ;
#4975 = DIRECTION ( 'NONE',  ( -0.8775825618903722036, 0.000000000000000000, 0.4794255386042041156 ) ) ;
#4976 = ORIENTED_EDGE ( 'NONE', *, *, #23341, .T. ) ;
#4977 = EDGE_CURVE ( 'NONE', #18448, #14011, #4569, .T. ) ;
#4978 = CARTESIAN_POINT ( 'NONE',  ( -2.934900197419999746, -94.89197151660000884, 23.49669041109999768 ) ) ;
#4979 = CARTESIAN_POINT ( 'NONE',  ( -18.92164427849999697, -32.73099401719999690, 12.31425843260000086 ) ) ;
#4980 = DIRECTION ( 'NONE',  ( 0.000000000000000000, -1.000000000000000000, 0.000000000000000000 ) ) ;
#4981 = CARTESIAN_POINT ( 'NONE',  ( 31.03260167810000070, -72.62832455090000394, -20.30285101509999990 ) ) ;
#4982 = DIRECTION ( 'NONE',  ( 0.8775825618903720926, 0.000000000000000000, 0.4794255386042039491 ) ) ;
#4983 = ADVANCED_FACE ( 'NONE', ( #6620 ), #6913, .T. ) ;
#4984 = ORIENTED_EDGE ( 'NONE', *, *, #11303, .F. ) ;
#4985 = CARTESIAN_POINT ( 'NONE',  ( 9.212281862759999385, -37.98196146859999800, -22.49242731490000224 ) ) ;
#4986 = DIRECTION ( 'NONE',  ( 0.000000000000000000, -1.000000000000000000, 0.000000000000000000 ) ) ;
#4987 = DIRECTION ( 'NONE',  ( 0.000000000000000000, 1.000000000000000000, 0.000000000000000000 ) ) ;
#4988 = DIRECTION ( 'NONE',  ( 0.000000000000000000, 1.000000000000000000, 0.000000000000000000 ) ) ;
#4989 = ORIENTED_EDGE ( 'NONE', *, *, #25889, .F. ) ;
#4990 = CARTESIAN_POINT ( 'NONE',  ( -34.71422205039999653, -79.50000000000000000, -24.10762033259999981 ) ) ;
#4991 = CARTESIAN_POINT ( 'NONE',  ( 16.46460381569999853, -94.70873790529999781, 17.03825317170000275 ) ) ;
#4992 = B_SPLINE_SURFACE_WITH_KNOTS ( 'NONE', 5, 5, ( 
 ( #25684, #5709, #3534, #10201, #8176, #14728, #19116, #28006, #10475 ),
 ( #28268, #5845, #12528, #8303, #19252, #17205, #6122, #18340, #26676 ),
 ( #27230, #27373, #8874, #10902, #13104, #19956, #24341, #7415, #6718 ),
 ( #27, #2348, #24197, #17496, #5224, #2198, #8594, #6409, #7268 ),
 ( #2904, #4381, #15429, #19668, #16133, #28688, #11761, #4228, #19810 ),
 ( #11201, #26381, #11041, #25196, #22015, #17788, #6567, #15585, #13957 ) ),
 .UNSPECIFIED., .F., .F., .F.,
 ( 6, 6 ),
 ( 6, 3, 6 ),
 ( 10.27996124010000045, 28.19205293310000116 ),
 ( 0.000000000000000000, 0.2500000000000000000, 0.5000000000000000000 ),
 .UNSPECIFIED. ) ;
#4993 = CARTESIAN_POINT ( 'NONE',  ( 24.03793476618687919, -19.49371143355231339, 1.498876886815959431 ) ) ;
#4994 = CARTESIAN_POINT ( 'NONE',  ( -6.943253548370000416, -101.2902355740000075, 14.33557670620000124 ) ) ;
#4995 = CARTESIAN_POINT ( 'NONE',  ( 6.019085164319999848, -92.50000467790000869, 29.30686339500000059 ) ) ;
#4996 = CARTESIAN_POINT ( 'NONE',  ( 8.441591539670000088, -37.31515243520000524, -21.68264306949999920 ) ) ;
#4997 = CARTESIAN_POINT ( 'NONE',  ( 45.84677419350000349, -73.50000000000000000, -4.286925650119999709 ) ) ;
#4998 = VERTEX_POINT ( 'NONE', #17545 ) ;
#4999 = TOROIDAL_SURFACE ( 'NONE', #5915, 3.750000000000000000, 1.000000000000000000 ) ;
#5000 = CARTESIAN_POINT ( 'NONE',  ( 8.207855523239999229, -98.78769286879999356, 16.44907893679999944 ) ) ;
#5001 = CARTESIAN_POINT ( 'NONE',  ( -40.70731707320000226, -82.25000000000000000, -7.215414233289999757 ) ) ;
#5002 = CARTESIAN_POINT ( 'NONE',  ( -12.28242885148121566, -19.47294316487861821, 19.19149835041444874 ) ) ;
#5003 = DIRECTION ( 'NONE',  ( 0.9993816408608721114, 0.000000000000000000, -0.03516156865429537204 ) ) ;
#5004 = DIRECTION ( 'NONE',  ( 1.000000000000000000, 0.000000000000000000, 0.000000000000000000 ) ) ;
#5005 = FACE_OUTER_BOUND ( 'NONE', #27732, .T. ) ;
#5006 = FACE_OUTER_BOUND ( 'NONE', #21251, .T. ) ;
#5007 = CARTESIAN_POINT ( 'NONE',  ( 14.54939535876293988, -95.49908309382901450, 17.32799205191540892 ) ) ;
#5008 = EDGE_CURVE ( 'NONE', #13409, #12777, #12361, .T. ) ;
#5009 = DIRECTION ( 'NONE',  ( 0.4692400087391615515, 0.000000000000000000, -0.8830706733883034731 ) ) ;
#5010 = CIRCLE ( 'NONE', #21295, 0.4999999999999967804 ) ;
#5011 = CARTESIAN_POINT ( 'NONE',  ( 12.04737265770000043, -101.6484611540000031, -10.52904611289999970 ) ) ;
#5012 = CARTESIAN_POINT ( 'NONE',  ( 21.85814127600000134, -49.11291935110000395, -7.592835430120000062 ) ) ;
#5013 = EDGE_CURVE ( 'NONE', #15673, #6736, #11568, .T. ) ;
#5014 = CARTESIAN_POINT ( 'NONE',  ( 8.770435879969156190, -35.38531427029693077, -20.52569411805346178 ) ) ;
#5015 = CARTESIAN_POINT ( 'NONE',  ( -15.71875659940000247, -100.6826114469999993, 2.591326689040000186 ) ) ;
#5016 = ORIENTED_EDGE ( 'NONE', *, *, #14232, .T. ) ;
#5017 = CARTESIAN_POINT ( 'NONE',  ( 36.72991148340000223, -74.73026516779999895, -14.71529450729999944 ) ) ;
#5018 = CARTESIAN_POINT ( 'NONE',  ( 6.744238910220000882, -101.2530993010000060, 13.61507422070000040 ) ) ;
#5019 = CARTESIAN_POINT ( 'NONE',  ( -22.33509239084705555, -79.80951032333221917, -32.79088695412508514 ) ) ;
#5020 = B_SPLINE_CURVE_WITH_KNOTS ( 'NONE', 3,
 ( #28267, #17204, #6267, #15133, #2060, #10900, #24042, #19808, #4080, #12949, #28687, #21860, #1912, #20112, #22420, #11764, #1427 ),
 .UNSPECIFIED., .F., .F.,
 ( 4, 2, 2, 1, 1, 1, 1, 1, 2, 2, 4 ),
 ( 0.000000000000000000, 0.2499999999997198352, 0.3749999999995797806, 0.4374999999995097255, 0.4687499999994720890, 0.4843749999994530486, 0.4921874999994436117, 0.4960937499994417799, 0.4980468749994406141, 0.4999999999994395039, 1.000000000000000000 ),
 .UNSPECIFIED. ) ;
#5021 = CIRCLE ( 'NONE', #14344, 0.3500000000000003664 ) ;
#5022 = CARTESIAN_POINT ( 'NONE',  ( -15.22757417880000119, -66.82180077600000345, 22.72230046389999814 ) ) ;
#5023 = CARTESIAN_POINT ( 'NONE',  ( 8.346327226119999665, -35.76750032119999645, -21.11704210819999972 ) ) ;
#5024 = CARTESIAN_POINT ( 'NONE',  ( -2.337241308500000336, -64.69849383090000572, -25.49681307870000069 ) ) ;
#5025 = CIRCLE ( 'NONE', #8711, 8.999999999999998224 ) ;
#5026 = CARTESIAN_POINT ( 'NONE',  ( 26.43538883845638665, -72.55114739962129988, 11.02537517961439839 ) ) ;
#5027 = CARTESIAN_POINT ( 'NONE',  ( 20.11250903250000022, -36.00000000000000000, -9.561259576869998611 ) ) ;
#5028 = CARTESIAN_POINT ( 'NONE',  ( -14.64295283881845933, -93.98969193940334321, -21.62035027063686599 ) ) ;
#5029 = CARTESIAN_POINT ( 'NONE',  ( 16.52775595720000013, -99.70407914540000149, 4.748034318380000229 ) ) ;
#5030 = ORIENTED_EDGE ( 'NONE', *, *, #734, .T. ) ;
#5031 = CARTESIAN_POINT ( 'NONE',  ( 21.46601194620000186, -36.21205870680000061, -7.351927201700000580 ) ) ;
#5032 = DIRECTION ( 'NONE',  ( 1.000000000000000000, 0.000000000000000000, 0.000000000000000000 ) ) ;
#5033 = VERTEX_POINT ( 'NONE', #7206 ) ;
#5034 = CARTESIAN_POINT ( 'NONE',  ( 8.538276090549652864, -92.66777315148682703, 29.28050361645156840 ) ) ;
#5035 = ORIENTED_EDGE ( 'NONE', *, *, #20019, .T. ) ;
#5036 = LINE ( 'NONE', #22677, #4867 ) ;
#5037 = CARTESIAN_POINT ( 'NONE',  ( -3.215510237749999778, -94.59276292389999696, 23.57860181210000405 ) ) ;
#5038 = DIRECTION ( 'NONE',  ( 0.000000000000000000, 1.000000000000000000, 0.000000000000000000 ) ) ;
#5039 = CARTESIAN_POINT ( 'NONE',  ( -7.247546674761930596, -74.11886065900105791, -40.20585889325029427 ) ) ;
#5040 = AXIS2_PLACEMENT_3D ( 'NONE', #3886, #14804, #1711 ) ;
#5041 = CARTESIAN_POINT ( 'NONE',  ( -14.46844930820000030, -74.19081742459999873, 36.42578001110000230 ) ) ;
#5042 = CARTESIAN_POINT ( 'NONE',  ( -22.29197733299999840, -68.17313230439998506, 14.44572620890000003 ) ) ;
#5043 = CARTESIAN_POINT ( 'NONE',  ( -13.53684476099999934, -28.27010607350000271, 20.60385118230000145 ) ) ;
#5044 = ORIENTED_EDGE ( 'NONE', *, *, #9159, .T. ) ;
#5045 = CIRCLE ( 'NONE', #21332, 10.50000000000000000 ) ;
#5046 = DIRECTION ( 'NONE',  ( 0.000000000000000000, 1.000000000000000000, 0.000000000000000000 ) ) ;
#5047 = CARTESIAN_POINT ( 'NONE',  ( 7.680652413499999831, -31.56454373169999883, -21.10194041029999923 ) ) ;
#5048 = CARTESIAN_POINT ( 'NONE',  ( -7.443137591229999295, -74.00000000000000000, 35.37770683939999827 ) ) ;
#5049 = CARTESIAN_POINT ( 'NONE',  ( -12.57997069900000042, -101.2141467319999890, -8.613800160570001196 ) ) ;
#5050 = DIRECTION ( 'NONE',  ( 0.000000000000000000, 1.000000000000000000, 0.000000000000000000 ) ) ;
#5051 = ORIENTED_EDGE ( 'NONE', *, *, #217, .F. ) ;
#5052 = CARTESIAN_POINT ( 'NONE',  ( 27.24068616960000000, -92.50000000000000000, -13.71841889620000110 ) ) ;
#5053 =( GEOMETRIC_REPRESENTATION_CONTEXT ( 3 ) GLOBAL_UNCERTAINTY_ASSIGNED_CONTEXT ( ( #18800 ) ) GLOBAL_UNIT_ASSIGNED_CONTEXT ( ( #5697, #28128, #23755 ) ) REPRESENTATION_CONTEXT ( 'NONE', 'WORKASPACE' ) );
#5054 = ORIENTED_EDGE ( 'NONE', *, *, #24540, .T. ) ;
#5055 = CARTESIAN_POINT ( 'NONE',  ( -12.67352077070000149, -74.00000000000000000, 33.30278006909999533 ) ) ;
#5056 = CARTESIAN_POINT ( 'NONE',  ( 1.342713516450000144, -94.57749834670001121, 24.16140173950000047 ) ) ;
#5057 = CARTESIAN_POINT ( 'NONE',  ( 4.182785939470000436, -93.31177568259998623, 25.48038252359999944 ) ) ;
#5058 = ORIENTED_EDGE ( 'NONE', *, *, #8972, .F. ) ;
#5059 = CIRCLE ( 'NONE', #19027, 5.500000000000001776 ) ;
#5060 = CARTESIAN_POINT ( 'NONE',  ( -1.527823559601194425, -96.61062616600978004, 21.17880622167292159 ) ) ;
#5061 = AXIS2_PLACEMENT_3D ( 'NONE', #14357, #17102, #7940 ) ;
#5062 = CARTESIAN_POINT ( 'NONE',  ( -23.14039283085165266, -72.53276285757912945, 16.72032736073078851 ) ) ;
#5063 = CARTESIAN_POINT ( 'NONE',  ( -14.29547445250000060, -80.00000000000000000, 45.69901703040000029 ) ) ;
#5064 = CARTESIAN_POINT ( 'NONE',  ( 11.31764174110000098, -36.00000000000000000, -22.43277175240000076 ) ) ;
#5065 = ORIENTED_EDGE ( 'NONE', *, *, #11624, .T. ) ;
#5066 = DIRECTION ( 'NONE',  ( 0.4794255386042000078, 0.000000000000000000, 0.8775825618903743131 ) ) ;
#5067 = CARTESIAN_POINT ( 'NONE',  ( -11.45377175261103631, -61.32605129436165470, 20.94518220247841711 ) ) ;
#5068 = EDGE_CURVE ( 'NONE', #5395, #15179, #25417, .T. ) ;
#5069 = VERTEX_POINT ( 'NONE', #5309 ) ;
#5070 = CARTESIAN_POINT ( 'NONE',  ( 23.98990767258865375, -64.35840732026599653, 10.71073183009686858 ) ) ;
#5071 = FACE_OUTER_BOUND ( 'NONE', #27797, .T. ) ;
#5072 = CARTESIAN_POINT ( 'NONE',  ( -2.984168974620000192, -69.33908554340000308, -27.31525404649999800 ) ) ;
#5073 = ADVANCED_FACE ( 'NONE', ( #9523 ), #16239, .T. ) ;
#5074 = CARTESIAN_POINT ( 'NONE',  ( -15.68940877609999873, -70.60291157129999817, 23.18755817509999773 ) ) ;
#5075 = VERTEX_POINT ( 'NONE', #526 ) ;
#5076 = CARTESIAN_POINT ( 'NONE',  ( 0.3059185938709999553, -93.00000000000000000, 14.72672055670000013 ) ) ;
#5077 = CARTESIAN_POINT ( 'NONE',  ( -12.09704001540000107, -79.50000000000000000, 47.10905722069999513 ) ) ;
#5078 = CARTESIAN_POINT ( 'NONE',  ( 24.89712376119999959, -63.41220263479998920, 0.7891782316930000540 ) ) ;
#5079 = CARTESIAN_POINT ( 'NONE',  ( -21.86233684099999763, -74.36373701399999447, -32.64238205049999664 ) ) ;
#5080 = EDGE_LOOP ( 'NONE', ( #27622, #9216, #7491, #4567 ) ) ;
#5081 = AXIS2_PLACEMENT_3D ( 'NONE', #2222, #2090, #4694 ) ;
#5082 = DIRECTION ( 'NONE',  ( -1.000000000000000000, 0.000000000000000000, 5.075305255429999693E-16 ) ) ;
#5083 = FACE_OUTER_BOUND ( 'NONE', #21093, .T. ) ;
#5084 = CARTESIAN_POINT ( 'NONE',  ( 36.61058569223673942, -74.16120954504201279, -14.29449953322217048 ) ) ;
#5085 = EDGE_LOOP ( 'NONE', ( #10608, #16930 ) ) ;
#5086 = CIRCLE ( 'NONE', #2298, 23.36116116979999902 ) ;
#5087 = CIRCLE ( 'NONE', #8779, 15.19391340349999986 ) ;
#5088 = DIRECTION ( 'NONE',  ( -1.000000000000000000, 0.000000000000000000, 0.000000000000000000 ) ) ;
#5089 = B_SPLINE_CURVE_WITH_KNOTS ( 'NONE', 3,
 ( #10849, #6358, #3893, #28220 ),
 .UNSPECIFIED., .F., .F.,
 ( 4, 4 ),
 ( -3.225498864409999999, -2.709627031390000163 ),
 .UNSPECIFIED. ) ;
#5090 = CIRCLE ( 'NONE', #15274, 25.14975229270000057 ) ;
#5091 = CARTESIAN_POINT ( 'NONE',  ( 23.15160389369999905, -62.53529079469999630, 10.48384440070000068 ) ) ;
#5092 = FACE_OUTER_BOUND ( 'NONE', #20221, .T. ) ;
#5093 = CARTESIAN_POINT ( 'NONE',  ( 16.34170762565740631, -100.4872618028340838, 4.353002873095284997 ) ) ;
#5094 = CARTESIAN_POINT ( 'NONE',  ( 4.500000000000000000, -15.00000000000000000, 31.00000000000000000 ) ) ;
#5095 = ORIENTED_EDGE ( 'NONE', *, *, #25673, .T. ) ;
#5096 = CARTESIAN_POINT ( 'NONE',  ( 20.94731949980000252, -52.62618816490000029, 10.41165191589999850 ) ) ;
#5097 = CYLINDRICAL_SURFACE ( 'NONE', #5662, 18.64285714290000584 ) ;
#5098 = CARTESIAN_POINT ( 'NONE',  ( -11.40956707329999809, -19.15825154520000240, 19.02831704529999968 ) ) ;
#5099 = CARTESIAN_POINT ( 'NONE',  ( -11.65869911329999908, -63.24100619559999359, -22.48820904579999791 ) ) ;
#5100 = SPHERICAL_SURFACE ( 'NONE', #15, 1.000000000000000000 ) ;
#5101 = DIRECTION ( 'NONE',  ( -1.000000000000000000, 0.000000000000000000, 0.000000000000000000 ) ) ;
#5102 = ORIENTED_EDGE ( 'NONE', *, *, #12897, .T. ) ;
#5103 = CARTESIAN_POINT ( 'NONE',  ( 10.87364956280000072, -37.98927800880000660, 19.90408201490000195 ) ) ;
#5104 = DIRECTION ( 'NONE',  ( 1.000000000000000000, 0.000000000000000000, 0.000000000000000000 ) ) ;
#5106 = EDGE_LOOP ( 'NONE', ( #4028, #17306, #4984, #20070 ) ) ;
#5105 = AXIS2_PLACEMENT_3D ( 'NONE', #7315, #7475, #20869 ) ;
#5107 = CARTESIAN_POINT ( 'NONE',  ( 23.03829042120000281, -52.56313962730000355, 10.32398954119999956 ) ) ;
#5108 = CARTESIAN_POINT ( 'NONE',  ( 9.220169834277720966, -98.40144667389034794, 16.53004056780445907 ) ) ;
#5109 = VERTEX_POINT ( 'NONE', #16521 ) ;
#5110 = ADVANCED_FACE ( 'NONE', ( #5006 ), #23684, .T. ) ;
#5111 = CARTESIAN_POINT ( 'NONE',  ( -50.00000000000000000, -12.50000000000000000, 4.500000000000000000 ) ) ;
#5113 = ADVANCED_FACE ( 'NONE', ( #20456 ), #8434, .T. ) ;
#5112 = CIRCLE ( 'NONE', #26037, 57.75000000000000000 ) ;
#5114 = AXIS2_PLACEMENT_3D ( 'NONE', #27613, #14197, #7781 ) ;
#5115 = CARTESIAN_POINT ( 'NONE',  ( -0.5354892050589999952, -54.24814459719999604, -23.24218483219999953 ) ) ;
#5116 = DIRECTION ( 'NONE',  ( 0.000000000000000000, 1.000000000000000000, 0.000000000000000000 ) ) ;
#5117 = CARTESIAN_POINT ( 'NONE',  ( 23.42164048755097383, -94.71481465625956275, -6.692245640674809870 ) ) ;
#5118 = EDGE_CURVE ( 'NONE', #11046, #6607, #12538, .T. ) ;
#5119 = CARTESIAN_POINT ( 'NONE',  ( -10.25754198879999990, -18.86159979430000178, -20.74776445359999855 ) ) ;
#5120 = CARTESIAN_POINT ( 'NONE',  ( 9.794085904993929503, -62.04428797445658716, -24.13968230914114343 ) ) ;
#5121 = EDGE_LOOP ( 'NONE', ( #16180, #15140, #10621, #19728, #21896 ) ) ;
#5122 = EDGE_CURVE ( 'NONE', #27080, #2923, #26013, .T. ) ;
#5123 = LINE ( 'NONE', #25240, #20931 ) ;
#5124 = B_SPLINE_CURVE_WITH_KNOTS ( 'NONE', 5,
 ( #27308, #666, #13596, #20452, #7203, #8924 ),
 .UNSPECIFIED., .F., .F.,
 ( 6, 6 ),
 ( 0.000000000000000000, 1.000000000000000000 ),
 .UNSPECIFIED. ) ;
#5125 = CARTESIAN_POINT ( 'NONE',  ( -20.44377240776747584, -61.67331079074745759, 12.48822562784140011 ) ) ;
#5126 = CYLINDRICAL_SURFACE ( 'NONE', #10690, 0.5000000000000004441 ) ;
#5127 = ORIENTED_EDGE ( 'NONE', *, *, #16186, .F. ) ;
#5128 = DIRECTION ( 'NONE',  ( 1.000000000000000000, 0.000000000000000000, 0.000000000000000000 ) ) ;
#5129 = FACE_OUTER_BOUND ( 'NONE', #22546, .T. ) ;
#5130 = FACE_OUTER_BOUND ( 'NONE', #12351, .T. ) ;
#5131 = ORIENTED_EDGE ( 'NONE', *, *, #8271, .T. ) ;
#5132 = CARTESIAN_POINT ( 'NONE',  ( -17.93586394770000325, -95.70815265259999194, 13.56389423130000083 ) ) ;
#5133 = FACE_OUTER_BOUND ( 'NONE', #3399, .T. ) ;
#5134 = CARTESIAN_POINT ( 'NONE',  ( -12.79457955380000023, -70.02558078490001492, -24.23939601560000057 ) ) ;
#5135 = CARTESIAN_POINT ( 'NONE',  ( 22.42217291749999930, -60.60023544439999910, -7.442794370989999742 ) ) ;
#5136 = VECTOR ( 'NONE', #4988, 1000.000000000000000 ) ;
#5137 = CARTESIAN_POINT ( 'NONE',  ( 26.22710519529999829, -65.11419048929998610, 1.448574456039999792 ) ) ;
#5138 = B_SPLINE_CURVE_WITH_KNOTS ( 'NONE', 3,
 ( #27641, #7683, #25444, #10806, #6168, #28459, #23667, #17539, #17106, #12848 ),
 .UNSPECIFIED., .F., .F.,
 ( 4, 2, 2, 2, 4 ),
 ( 0.000000000000000000, 0.2500000000000000000, 0.5000000000000000000, 0.7500000000000000000, 1.000000000000000000 ),
 .UNSPECIFIED. ) ;
#5139 = ORIENTED_EDGE ( 'NONE', *, *, #13819, .T. ) ;
#5140 = DIRECTION ( 'NONE',  ( -0.2414462220490753985, 0.000000000000000000, 0.9704142011833032377 ) ) ;
#5141 = CARTESIAN_POINT ( 'NONE',  ( 21.59295723509999831, -37.02888336210000375, -8.543455487960001093 ) ) ;
#5142 = CARTESIAN_POINT ( 'NONE',  ( 14.78241224890000183, -96.95622554120001269, 14.77248467170000090 ) ) ;
#5143 = ORIENTED_EDGE ( 'NONE', *, *, #14512, .F. ) ;
#5144 = CARTESIAN_POINT ( 'NONE',  ( 7.256994698139999755, -74.37142462010000088, 40.28432270869999599 ) ) ;
#5145 = CARTESIAN_POINT ( 'NONE',  ( 16.42966481050000027, -94.59276479679999738, 17.21499971510000293 ) ) ;
#5146 = EDGE_CURVE ( 'NONE', #9249, #21683, #17224, .T. ) ;
#5147 = CARTESIAN_POINT ( 'NONE',  ( 47.25063473080000165, -79.41040171960000293, -0.8747163666420000316 ) ) ;
#5148 = SURFACE_SIDE_STYLE ('',( #25117 ) ) ;
#5149 = CARTESIAN_POINT ( 'NONE',  ( 0.000000000000000000, -111.0000000000000000, 0.000000000000000000 ) ) ;
#5150 = DIRECTION ( 'NONE',  ( 0.2414462220490755373, 0.000000000000000000, 0.9704142011833032377 ) ) ;
#5151 = CONICAL_SURFACE ( 'NONE', #24697, 21.99999999999999645, 0.03490658503990158590 ) ;
#5152 = CARTESIAN_POINT ( 'NONE',  ( -6.781378104809999030, -101.6484611540000031, 14.49182221120000058 ) ) ;
#5153 = ORIENTED_EDGE ( 'NONE', *, *, #19348, .F. ) ;
#5154 = CONICAL_SURFACE ( 'NONE', #8839, 55.67692378859999280, 1.047197551199999799 ) ;
#5155 = EDGE_CURVE ( 'NONE', #21247, #16409, #19401, .T. ) ;
#5156 = CARTESIAN_POINT ( 'NONE',  ( -39.46631086808643829, -73.67850591079914579, 7.230541818641200713 ) ) ;
#5157 = AXIS2_PLACEMENT_3D ( 'NONE', #24769, #2919, #608 ) ;
#5158 = CARTESIAN_POINT ( 'NONE',  ( 23.99083882220000064, -19.17999199609999650, 1.537804108040000006 ) ) ;
#5159 = CARTESIAN_POINT ( 'NONE',  ( 12.02679296059999814, -98.69238697830000717, -15.68885798269999832 ) ) ;
#5160 = ORIENTED_EDGE ( 'NONE', *, *, #27869, .T. ) ;
#5161 = CARTESIAN_POINT ( 'NONE',  ( -27.04683438039999999, -79.50000000000000000, -36.23922253580000330 ) ) ;
#5162 = DIRECTION ( 'NONE',  ( -0.4151946956541399669, 0.5000000000001689759, -0.7600087925152558821 ) ) ;
#5163 = CARTESIAN_POINT ( 'NONE',  ( -2.079970928869999902, -32.71502530469999925, -23.05888968329999855 ) ) ;
#5164 = CARTESIAN_POINT ( 'NONE',  ( 14.64236194031395044, -95.45364739782090169, 17.32643780036390879 ) ) ;
#5165 = DIRECTION ( 'NONE',  ( 0.8830706733883038062, 0.000000000000000000, 0.4692400087391607744 ) ) ;
#5166 = DIRECTION ( 'NONE',  ( 0.000000000000000000, 1.000000000000000000, 0.000000000000000000 ) ) ;
#5167 = CARTESIAN_POINT ( 'NONE',  ( -43.20000000000000284, -65.14977478849999670, 0.1732050807559999961 ) ) ;
#5168 = CARTESIAN_POINT ( 'NONE',  ( -26.69328098980000163, -79.50000000000000000, -35.88566914520000495 ) ) ;
#5169 = ORIENTED_EDGE ( 'NONE', *, *, #5850, .T. ) ;
#5170 = CARTESIAN_POINT ( 'NONE',  ( -32.83566819349999832, -74.43710720380001078, -22.22906645439999807 ) ) ;
#5171 = CARTESIAN_POINT ( 'NONE',  ( 13.87499543336579144, -97.43022994613481558, -15.19070948534773180 ) ) ;
#5172 = TOROIDAL_SURFACE ( 'NONE', #9818, 6.750000000000000000, 2.000000000000000000 ) ;
#5173 = CIRCLE ( 'NONE', #11664, 0.3500000000000003664 ) ;
#5174 = CIRCLE ( 'NONE', #19121, 0.5000000000000004441 ) ;
#5175 = CARTESIAN_POINT ( 'NONE',  ( -13.09595933279999969, -66.29670474889999809, 22.12657759070000196 ) ) ;
#5176 = CARTESIAN_POINT ( 'NONE',  ( 8.753525549769999969, -35.66748467180000404, -20.66368372700000222 ) ) ;
#5177 = FACE_OUTER_BOUND ( 'NONE', #27792, .T. ) ;
#5178 = DIRECTION ( 'NONE',  ( 1.000000000000000000, 0.000000000000000000, 0.000000000000000000 ) ) ;
#5179 = DIRECTION ( 'NONE',  ( 0.000000000000000000, -1.000000000000000000, 0.000000000000000000 ) ) ;
#5180 = CARTESIAN_POINT ( 'NONE',  ( -40.70731707320000226, -74.50000000000000000, 7.215414233289999757 ) ) ;
#5181 = EDGE_CURVE ( 'NONE', #3837, #20989, #21731, .T. ) ;
#5182 = EDGE_CURVE ( 'NONE', #21366, #7391, #1652, .T. ) ;
#5183 = ORIENTED_EDGE ( 'NONE', *, *, #18686, .F. ) ;
#5184 = DIRECTION ( 'NONE',  ( 0.000000000000000000, 1.000000000000000000, 0.000000000000000000 ) ) ;
#5185 = CARTESIAN_POINT ( 'NONE',  ( -17.80939098829999878, -98.43722211970001013, -8.214143917099999470 ) ) ;
#5186 = ORIENTED_EDGE ( 'NONE', *, *, #11965, .T. ) ;
#5187 = DIRECTION ( 'NONE',  ( 1.000000000000000000, 0.000000000000000000, 0.000000000000000000 ) ) ;
#5188 = EDGE_CURVE ( 'NONE', #15327, #20206, #12941, .T. ) ;
#5189 = CARTESIAN_POINT ( 'NONE',  ( 0.6125012097518164333, -100.6644468680149060, -16.75904295264657762 ) ) ;
#5190 = CARTESIAN_POINT ( 'NONE',  ( -4.643931556212963052, -95.55433702412769037, 22.13027306510061720 ) ) ;
#5191 = DIRECTION ( 'NONE',  ( 0.2414462220490755373, 0.000000000000000000, -0.9704142011833032377 ) ) ;
#5192 = AXIS2_PLACEMENT_3D ( 'NONE', #15288, #24357, #26540 ) ;
#5193 = CARTESIAN_POINT ( 'NONE',  ( -7.135467526410000261, -73.50000000000000000, -38.71641004229999794 ) ) ;
#5194 = VECTOR ( 'NONE', #6671, 1000.000000000000000 ) ;
#5195 = CIRCLE ( 'NONE', #984, 0.4999999999999981126 ) ;
#5196 = CARTESIAN_POINT ( 'NONE',  ( -14.51986742080000070, -74.16918790970001396, 36.33983588299999923 ) ) ;
#5197 = CARTESIAN_POINT ( 'NONE',  ( -20.89470113539999829, -64.89165740699999674, 14.23290170900000007 ) ) ;
#5198 = CARTESIAN_POINT ( 'NONE',  ( 23.77207126295173367, -92.72059904818672749, -19.10860135063087384 ) ) ;
#5199 = ORIENTED_EDGE ( 'NONE', *, *, #26685, .T. ) ;
#5200 = CYLINDRICAL_SURFACE ( 'NONE', #6943, 57.74999999999999289 ) ;
#5201 = CARTESIAN_POINT ( 'NONE',  ( 8.999623101399999214, -28.60070731709999947, -19.24185364099999873 ) ) ;
#5202 = DIRECTION ( 'NONE',  ( 0.7414456417930908039, 0.000000000000000000, 0.6710129359900831592 ) ) ;
#5203 = CARTESIAN_POINT ( 'NONE',  ( -41.70763373158882814, -63.05619511567403634, 2.812618181363554015 ) ) ;
#5204 = CARTESIAN_POINT ( 'NONE',  ( -38.71640952649999434, -73.65708014139998738, -7.135466514619999145 ) ) ;
#5205 = ORIENTED_EDGE ( 'NONE', *, *, #9166, .T. ) ;
#5206 = EDGE_CURVE ( 'NONE', #10474, #12521, #4146, .T. ) ;
#5207 = ORIENTED_EDGE ( 'NONE', *, *, #5941, .F. ) ;
#5208 = DIRECTION ( 'NONE',  ( 0.000000000000000000, 1.000000000000000000, 0.000000000000000000 ) ) ;
#5209 = CIRCLE ( 'NONE', #12617, 16.00000000000000000 ) ;
#5210 = CARTESIAN_POINT ( 'NONE',  ( 0.000000000000000000, -82.50000000000000000, 0.000000000000000000 ) ) ;
#5211 = DIRECTION ( 'NONE',  ( -0.4381045938801422235, -0.4061384660531317525, -0.8019450799232605842 ) ) ;
#5212 = CIRCLE ( 'NONE', #7562, 9.999999999999996447 ) ;
#5213 = CARTESIAN_POINT ( 'NONE',  ( 10.51051219959999905, -93.03281165500000327, 27.57047580710000290 ) ) ;
#5214 = EDGE_LOOP ( 'NONE', ( #20365, #13759, #26373, #1495 ) ) ;
#5215 = ADVANCED_FACE ( 'NONE', ( #17364 ), #28451, .T. ) ;
#5216 = ADVANCED_FACE ( 'NONE', ( #13412 ), #23249, .F. ) ;
#5217 = ORIENTED_EDGE ( 'NONE', *, *, #27565, .T. ) ;
#5218 = FACE_OUTER_BOUND ( 'NONE', #2000, .T. ) ;
#5219 = CARTESIAN_POINT ( 'NONE',  ( 0.000000000000000000, -17.30000000000000071, 0.000000000000000000 ) ) ;
#5220 = DIRECTION ( 'NONE',  ( 1.000000000000000000, 0.000000000000000000, 0.000000000000000000 ) ) ;
#5221 = ORIENTED_EDGE ( 'NONE', *, *, #11152, .F. ) ;
#5222 = CARTESIAN_POINT ( 'NONE',  ( 7.244487271036906151, -74.17548517116718187, -40.28268501225647213 ) ) ;
#5223 = CARTESIAN_POINT ( 'NONE',  ( -11.70222064965240172, -62.88295250684831927, 21.29956024434785533 ) ) ;
#5224 = CARTESIAN_POINT ( 'NONE',  ( -6.547105968080000338, -97.18075703250001141, -19.87372873440000376 ) ) ;
#5225 = CARTESIAN_POINT ( 'NONE',  ( -12.22512452690000018, -101.6484611540000031, -9.528710841509999696 ) ) ;
#5226 = CARTESIAN_POINT ( 'NONE',  ( -1.921056761090000009, -65.40406720010000186, -25.43250850220000103 ) ) ;
#5227 = CARTESIAN_POINT ( 'NONE',  ( -14.26173026869999916, -70.13572605659999226, 23.46380719780000135 ) ) ;
#5228 = ORIENTED_EDGE ( 'NONE', *, *, #23622, .T. ) ;
#5229 = DIRECTION ( 'NONE',  ( 0.000000000000000000, 1.000000000000000000, 0.000000000000000000 ) ) ;
#5230 = CARTESIAN_POINT ( 'NONE',  ( -15.72691182720000214, -100.6651030490000096, 2.680982550860000035 ) ) ;
#5231 = CARTESIAN_POINT ( 'NONE',  ( 25.13837759289999951, -65.04696659260000047, -0.1122880703080000042 ) ) ;
#5232 = CARTESIAN_POINT ( 'NONE',  ( 19.49031394080000013, -35.44486363859999756, -8.986483599810000555 ) ) ;
#5233 = ORIENTED_EDGE ( 'NONE', *, *, #7346, .F. ) ;
#5234 = DIRECTION ( 'NONE',  ( 0.000000000000000000, -1.000000000000000000, 0.000000000000000000 ) ) ;
#5235 = CIRCLE ( 'NONE', #10780, 3.000000000000000888 ) ;
#5236 = CARTESIAN_POINT ( 'NONE',  ( -2.659303201050000176, -19.18187901349999791, -24.02256761569999810 ) ) ;
#5237 = CARTESIAN_POINT ( 'NONE',  ( 24.18486883099999929, -92.81180222670001001, -12.79052883029999954 ) ) ;
#5239 = ORIENTED_EDGE ( 'NONE', *, *, #3504, .T. ) ;
#5238 = B_SPLINE_CURVE_WITH_KNOTS ( 'NONE', 3,
 ( #25080, #5115, #22902, #2941 ),
 .UNSPECIFIED., .F., .F.,
 ( 4, 4 ),
 ( 0.000000000000000000, 6.855861996820000748 ),
 .UNSPECIFIED. ) ;
#5240 = CARTESIAN_POINT ( 'NONE',  ( -9.548240116189999682, -93.74526857300000415, -23.19355367660000056 ) ) ;
#5241 = EDGE_CURVE ( 'NONE', #1763, #14956, #2361, .T. ) ;
#5242 = CARTESIAN_POINT ( 'NONE',  ( 22.19742911240000183, -63.93339545899999621, 11.06904267899999894 ) ) ;
#5243 = CARTESIAN_POINT ( 'NONE',  ( 8.448066558069998067, -35.04931392889999842, -20.87699790789999810 ) ) ;
#5244 = CARTESIAN_POINT ( 'NONE',  ( 16.03248225524879444, -100.8945630371651276, 4.256357661172395446 ) ) ;
#5245 = CARTESIAN_POINT ( 'NONE',  ( 29.41275679339999982, -10.50000000000000000, 53.83969017199999740 ) ) ;
#5246 = ORIENTED_EDGE ( 'NONE', *, *, #8164, .T. ) ;
#5247 = B_SPLINE_SURFACE_WITH_KNOTS ( 'NONE', 5, 5, ( 
 ( #7603, #23313, #18809, #19080, #27701, #5257, #3089, #11940, #27964 ),
 ( #8002, #7865, #3496, #16467, #23586, #5398, #3630, #3221, #769 ),
 ( #18942, #23040, #9614, #1192, #7739, #25501, #18515, #12354, #20994 ),
 ( #5532, #20712, #14552, #27408, #21264, #7457, #16316, #20853, #913 ),
 ( #9754, #3358, #18667, #14282, #23178, #12225, #23457, #21133, #12082 ),
 ( #10028, #1056, #27825, #16746, #25643, #5672, #1318, #10160, #28373 ) ),
 .UNSPECIFIED., .F., .F., .F.,
 ( 6, 6 ),
 ( 6, 3, 6 ),
 ( 4.816191416739999731, 6.255250589900000158 ),
 ( 0.000000000000000000, 0.2500000000000000000, 0.5000000000000000000 ),
 .UNSPECIFIED. ) ;
#5248 = CARTESIAN_POINT ( 'NONE',  ( -12.30071345790000059, -60.59571585039999775, -20.16720244700000109 ) ) ;
#5249 = ADVANCED_FACE ( 'NONE', ( #2661 ), #638, .T. ) ;
#5250 = CARTESIAN_POINT ( 'NONE',  ( 6.173817828315791623, -93.45278262996737340, 26.74719681978107744 ) ) ;
#5251 = ORIENTED_EDGE ( 'NONE', *, *, #14018, .T. ) ;
#5252 = CARTESIAN_POINT ( 'NONE',  ( 46.73654926506065266, -73.84018091753036117, -2.679827245328084029 ) ) ;
#5253 = ORIENTED_EDGE ( 'NONE', *, *, #21481, .F. ) ;
#5254 = B_SPLINE_CURVE_WITH_KNOTS ( 'NONE', 5,
 ( #25082, #11947, #9476, #7306, #7745, #5117, #21141, #918, #25648 ),
 .UNSPECIFIED., .F., .F.,
 ( 6, 3, 6 ),
 ( 0.000000000000000000, 0.5000000000000000000, 1.000000000000000000 ),
 .UNSPECIFIED. ) ;
#5255 = AXIS2_PLACEMENT_3D ( 'NONE', #25032, #5366, #5066 ) ;
#5256 = CARTESIAN_POINT ( 'NONE',  ( -10.80893812770000117, -34.66940579810000145, 19.80733931360000000 ) ) ;
#5257 = CARTESIAN_POINT ( 'NONE',  ( -5.582121642149999730, -100.8816835080000089, 14.77497840909999915 ) ) ;
#5258 = VERTEX_POINT ( 'NONE', #16336 ) ;
#5259 = CIRCLE ( 'NONE', #28501, 3.750000000000000000 ) ;
#5260 = CARTESIAN_POINT ( 'NONE',  ( 45.99664576397077553, -80.06168502921590857, -4.396813276268206394 ) ) ;
#5261 = DIRECTION ( 'NONE',  ( -0.000000000000000000, 1.000000000000000000, 0.000000000000000000 ) ) ;
#5262 = CARTESIAN_POINT ( 'NONE',  ( -10.45725474138590982, -19.47453298910726716, -20.36980114618768312 ) ) ;
#5263 = CARTESIAN_POINT ( 'NONE',  ( -13.36030084967533682, -101.4218099524540264, -9.110383877951878873 ) ) ;
#5264 = DIRECTION ( 'NONE',  ( 1.000000000000000000, 0.000000000000000000, 0.000000000000000000 ) ) ;
#5265 = CARTESIAN_POINT ( 'NONE',  ( 10.08508256729999886, -64.24504434620000382, -24.78974309399999854 ) ) ;
#5266 = VERTEX_POINT ( 'NONE', #27425 ) ;
#5267 = DIRECTION ( 'NONE',  ( 0.000000000000000000, -1.000000000000000000, 0.000000000000000000 ) ) ;
#5268 = CARTESIAN_POINT ( 'NONE',  ( 12.53707620288065350, -93.63284908669999140, -21.72543824449705596 ) ) ;
#5269 = CARTESIAN_POINT ( 'NONE',  ( -20.02788083190000279, -92.50000000000000000, 20.80461572599999798 ) ) ;
#5270 = DIRECTION ( 'NONE',  ( 0.4794255386042036715, 0.000000000000000000, 0.8775825618903724257 ) ) ;
#5271 = ORIENTED_EDGE ( 'NONE', *, *, #22051, .T. ) ;
#5272 = CIRCLE ( 'NONE', #20645, 0.5000000000000027756 ) ;
#5273 = FACE_OUTER_BOUND ( 'NONE', #563, .T. ) ;
#5274 = CARTESIAN_POINT ( 'NONE',  ( -12.23011636260000046, -101.1292389600000092, -9.532601661500001100 ) ) ;
#5275 = DIRECTION ( 'NONE',  ( 0.7506477800816132584, 0.000000000000000000, -0.6607025883546591150 ) ) ;
#5276 = ORIENTED_EDGE ( 'NONE', *, *, #6404, .F. ) ;
#5277 = CARTESIAN_POINT ( 'NONE',  ( -18.25187102170000131, -97.32059399370000108, 11.22053352470000043 ) ) ;
#5278 = TOROIDAL_SURFACE ( 'NONE', #2002, 55.85192378860000417, 0.3499999999999999778 ) ;
#5279 = CARTESIAN_POINT ( 'NONE',  ( -19.63703172620000004, -39.31812514049999407, 14.25736781099999995 ) ) ;
#5280 = DIRECTION ( 'NONE',  ( 0.4794255386042000078, 0.000000000000000000, 0.8775825618903743131 ) ) ;
#5281 = CARTESIAN_POINT ( 'NONE',  ( 27.75394116159999669, -74.50000000000000000, -27.75394116159999669 ) ) ;
#5282 = EDGE_CURVE ( 'NONE', #25457, #1700, #25762, .T. ) ;
#5283 = CARTESIAN_POINT ( 'NONE',  ( 23.45077801099999704, -61.76643916500000131, -9.453800512080000829 ) ) ;
#5284 = VECTOR ( 'NONE', #20673, 1000.000000000000000 ) ;
#5285 = EDGE_CURVE ( 'NONE', #2397, #22989, #3250, .T. ) ;
#5286 = EDGE_CURVE ( 'NONE', #16026, #20739, #8794, .T. ) ;
#5287 = EDGE_CURVE ( 'NONE', #6525, #8106, #1966, .T. ) ;
#5288 = VERTEX_POINT ( 'NONE', #25246 ) ;
#5289 = CARTESIAN_POINT ( 'NONE',  ( -7.105427357599999217E-15, -84.50000000000000000, -3.552713678799999608E-15 ) ) ;
#5290 = CARTESIAN_POINT ( 'NONE',  ( 1.598721155460000041E-15, -84.50000000000000000, 3.352873534370000046E-15 ) ) ;
#5291 = CIRCLE ( 'NONE', #675, 3.500000000000003109 ) ;
#5292 = CARTESIAN_POINT ( 'NONE',  ( 21.56903202939999886, -37.01027120230000378, -8.514697926349999335 ) ) ;
#5293 = DIRECTION ( 'NONE',  ( 0.000000000000000000, -1.000000000000000000, 0.000000000000000000 ) ) ;
#5294 = ORIENTED_EDGE ( 'NONE', *, *, #22492, .F. ) ;
#5295 = CARTESIAN_POINT ( 'NONE',  ( 21.32348952279355814, -36.24018116387741628, -9.136262763236869588 ) ) ;
#5296 = CARTESIAN_POINT ( 'NONE',  ( -13.41619584950000110, -101.2306315440000049, -9.103915625870000028 ) ) ;
#5297 = FACE_OUTER_BOUND ( 'NONE', #22057, .T. ) ;
#5298 = FILL_AREA_STYLE ('',( #3263 ) ) ;
#5299 = CARTESIAN_POINT ( 'NONE',  ( 8.437044979949998691, -36.55186187079999627, -21.65894763279999680 ) ) ;
#5300 = AXIS2_PLACEMENT_3D ( 'NONE', #17761, #26647, #4492 ) ;
#5301 = CARTESIAN_POINT ( 'NONE',  ( 7.555516771499999784, -101.3253988449999952, 13.99788120350000042 ) ) ;
#5302 = ORIENTED_EDGE ( 'NONE', *, *, #25396, .F. ) ;
#5303 = DIRECTION ( 'NONE',  ( 0.000000000000000000, 1.000000000000000000, 0.000000000000000000 ) ) ;
#5304 = FACE_OUTER_BOUND ( 'NONE', #22857, .T. ) ;
#5305 = CARTESIAN_POINT ( 'NONE',  ( 11.56404080679999957, -97.23151480800000002, -17.97423634720000152 ) ) ;
#5306 = ORIENTED_EDGE ( 'NONE', *, *, #15873, .T. ) ;
#5307 = CARTESIAN_POINT ( 'NONE',  ( -1.494460185578279088, -19.46625705891651847, -22.21735697087711969 ) ) ;
#5308 = CARTESIAN_POINT ( 'NONE',  ( 11.91199879370000048, -101.3256027080000052, -10.54214213689999902 ) ) ;
#5309 = CARTESIAN_POINT ( 'NONE',  ( 26.46310988749999993, -64.24504445130001784, 1.532420830840000026 ) ) ;
#5310 = CARTESIAN_POINT ( 'NONE',  ( -18.38790699489164737, -92.50638022835023833, 24.33425043882840200 ) ) ;
#5311 = AXIS2_PLACEMENT_3D ( 'NONE', #11779, #26956, #752 ) ;
#5312 = CARTESIAN_POINT ( 'NONE',  ( -38.90587669217570976, -73.50000000000002842, 7.169550435234046226 ) ) ;
#5313 = CARTESIAN_POINT ( 'NONE',  ( 11.91128644723943708, -101.5839620086842814, -10.75510067162974970 ) ) ;
#5314 = CARTESIAN_POINT ( 'NONE',  ( 21.65894763289999858, -36.55186186859999964, -8.437044980280001383 ) ) ;
#5315 = LINE ( 'NONE', #14205, #3028 ) ;
#5316 = DIRECTION ( 'NONE',  ( 0.000000000000000000, 1.000000000000000000, 0.000000000000000000 ) ) ;
#5317 = VERTEX_POINT ( 'NONE', #4838 ) ;
#5318 = EDGE_CURVE ( 'NONE', #77, #7539, #13941, .T. ) ;
#5319 = B_SPLINE_CURVE_WITH_KNOTS ( 'NONE', 3,
 ( #1199, #9762, #10034, #8010, #18818, #27707, #5407, #7746, #16612, #16900, #1735, #13221, #4048, #21979 ),
 .UNSPECIFIED., .F., .F.,
 ( 4, 2, 2, 1, 1, 2, 2, 4 ),
 ( 0.000000000000000000, 0.2500000000000178746, 0.3750000000000266454, 0.4375000000000310307, 0.4687500000000333067, 0.4843750000000344169, 0.5000000000000355271, 1.000000000000000000 ),
 .UNSPECIFIED. ) ;
#5320 = B_SPLINE_CURVE_WITH_KNOTS ( 'NONE', 3,
 ( #3218, #22895, #27404, #16465, #12079, #24780, #2933, #25225, #22743, #22599, #18512, #18070, #7005, #4819, #13697, #20552, #5252, #20707, #7999, #3765, #23864, #1315, #8135, #14418, #10025, #10157, #12484, #14818, #18806, #12626, #19077 ),
 .UNSPECIFIED., .F., .F.,
 ( 4, 2, 1, 1, 1, 2, 2, 2, 1, 1, 1, 2, 2, 2, 1, 1, 1, 2, 2, 4 ),
 ( 0.000000000000000000, 0.1250000000000331124, 0.1875000000000519307, 0.2187500000000589251, 0.2343750000000601463, 0.2421875000000630329, 0.2500000000000659472, 0.3750000000000856537, 0.4375000000000947020, 0.4687500000000999756, 0.4843750000001043055, 0.4921875000001044720, 0.5000000000001045830, 0.6250000000000885958, 0.6875000000000806022, 0.7187500000000779377, 0.7343750000000768274, 0.7421875000000747180, 0.7500000000000724976, 1.000000000000000000 ),
 .UNSPECIFIED. ) ;
#5321 = CARTESIAN_POINT ( 'NONE',  ( 6.946147887829999590, -101.6311724339999927, 14.42877099100000216 ) ) ;
#5322 = CARTESIAN_POINT ( 'NONE',  ( 47.19280574540000117, -74.66665734379999719, -1.149945984370000174 ) ) ;
#5323 = VECTOR ( 'NONE', #2324, 1000.000000000000000 ) ;
#5324 = EDGE_CURVE ( 'NONE', #19945, #25155, #14402, .T. ) ;
#5325 = CARTESIAN_POINT ( 'NONE',  ( -2.664535259099999805E-15, -72.00000000000000000, -3.552713678799999608E-15 ) ) ;
#5326 = FACE_OUTER_BOUND ( 'NONE', #12299, .T. ) ;
#5327 = CARTESIAN_POINT ( 'NONE',  ( 10.20110288159999890, -84.00000000000000000, 41.00000000000000000 ) ) ;
#5328 = DIRECTION ( 'NONE',  ( 0.000000000000000000, -1.000000000000000000, 0.000000000000000000 ) ) ;
#5329 = CARTESIAN_POINT ( 'NONE',  ( -20.15695820925639126, -93.11247489648164333, -20.71965102693426530 ) ) ;
#5330 = VECTOR ( 'NONE', #23160, 1000.000000000000000 ) ;
#5331 = LINE ( 'NONE', #20636, #14500 ) ;
#5332 = EDGE_LOOP ( 'NONE', ( #2430, #7969, #4855, #7432 ) ) ;
#5333 = AXIS2_PLACEMENT_3D ( 'NONE', #18484, #28557, #10757 ) ;
#5334 = DIRECTION ( 'NONE',  ( 0.000000000000000000, 1.000000000000000000, 0.000000000000000000 ) ) ;
#5335 = CARTESIAN_POINT ( 'NONE',  ( -40.77792552671823501, -63.24690319806511241, 2.469861454416400370 ) ) ;
#5336 = VERTEX_POINT ( 'NONE', #7176 ) ;
#5337 = FACE_OUTER_BOUND ( 'NONE', #15838, .T. ) ;
#5338 = CARTESIAN_POINT ( 'NONE',  ( 0.5980344247127714619, -100.4211561361990732, -16.95372977634908906 ) ) ;
#5339 = CARTESIAN_POINT ( 'NONE',  ( -7.185776204499999764, -73.64071409359999620, 38.99606912750000731 ) ) ;
#5340 = CARTESIAN_POINT ( 'NONE',  ( -40.00000000000000000, -65.84529946160000691, 0.000000000000000000 ) ) ;
#5341 = CARTESIAN_POINT ( 'NONE',  ( 25.07535757159999790, -74.22136841340000046, -30.21433045149999685 ) ) ;
#5342 = CARTESIAN_POINT ( 'NONE',  ( 9.226669613569999484, -71.28738307410000630, -26.41756239489999913 ) ) ;
#5343 = CARTESIAN_POINT ( 'NONE',  ( -13.46604720019999846, -19.89614183979999851, 20.40796202710000173 ) ) ;
#5344 = VECTOR ( 'NONE', #23415, 1000.000000000000000 ) ;
#5346 = ADVANCED_FACE ( 'NONE', ( #27135 ), #21826, .F. ) ;
#5345 = DIRECTION ( 'NONE',  ( 0.000000000000000000, -1.000000000000000000, 0.000000000000000000 ) ) ;
#5347 = DIRECTION ( 'NONE',  ( 1.000000000000000000, 0.000000000000000000, 0.000000000000000000 ) ) ;
#5348 = CARTESIAN_POINT ( 'NONE',  ( 10.33697414329999908, -72.00000000000000000, -28.69893982729999848 ) ) ;
#5349 = DIRECTION ( 'NONE',  ( 0.9842024174352067556, 0.000000000000000000, -0.1770468907230369482 ) ) ;
#5350 = VERTEX_POINT ( 'NONE', #9487 ) ;
#5351 = ADVANCED_FACE ( 'NONE', ( #22915 ), #25127, .T. ) ;
#5352 = DIRECTION ( 'NONE',  ( 1.000000000000000000, 0.000000000000000000, 0.000000000000000000 ) ) ;
#5353 = ADVANCED_BREP_SHAPE_REPRESENTATION ( '', ( #15528, #26433 ), #5053 ) ;
#5354 = AXIS2_PLACEMENT_3D ( 'NONE', #2241, #370, #7058 ) ;
#5355 = ORIENTED_EDGE ( 'NONE', *, *, #1193, .F. ) ;
#5356 = EDGE_CURVE ( 'NONE', #11676, #25229, #27895, .T. ) ;
#5357 = CARTESIAN_POINT ( 'NONE',  ( -0.8483992499709999136, -57.91738531389999878, -23.36308592830000208 ) ) ;
#5358 = CARTESIAN_POINT ( 'NONE',  ( 0.000000000000000000, -92.50000000000000000, 0.000000000000000000 ) ) ;
#5359 = CARTESIAN_POINT ( 'NONE',  ( 4.140575906510000515, -93.29998627720000570, 25.57099462040000049 ) ) ;
#5360 = ORIENTED_EDGE ( 'NONE', *, *, #18023, .T. ) ;
#5361 = CARTESIAN_POINT ( 'NONE',  ( -11.17102488801581650, -94.77696260184704613, -20.89251602398021035 ) ) ;
#5362 = CARTESIAN_POINT ( 'NONE',  ( -29.24808533433442648, -93.02765837721192099, 4.206566995128039999 ) ) ;
#5363 = CARTESIAN_POINT ( 'NONE',  ( 22.03428119550000019, -37.34495693419999185, -8.933655458900000568 ) ) ;
#5364 = CARTESIAN_POINT ( 'NONE',  ( 46.96755458150000351, -74.27975760209999123, -2.596029696810000065 ) ) ;
#5365 = ORIENTED_EDGE ( 'NONE', *, *, #11712, .T. ) ;
#5366 = DIRECTION ( 'NONE',  ( -0.8775825618903722036, 0.000000000000000000, 0.4794255386042041156 ) ) ;
#5367 = DIRECTION ( 'NONE',  ( 1.000000000000000000, 0.000000000000000000, 0.000000000000000000 ) ) ;
#5368 = ADVANCED_FACE ( 'NONE', ( #16041 ), #21378, .T. ) ;
#5369 = DIRECTION ( 'NONE',  ( 1.000000000000000000, 0.000000000000000000, 0.000000000000000000 ) ) ;
#5370 = CIRCLE ( 'NONE', #16046, 61.35000000000000142 ) ;
#5371 = CARTESIAN_POINT ( 'NONE',  ( -3.243670240720000209, -70.36214388629998950, -27.70857142859999911 ) ) ;
#5372 = CARTESIAN_POINT ( 'NONE',  ( -14.93352430010000020, -69.88459027950000291, 23.05437816310000088 ) ) ;
#5373 = ORIENTED_EDGE ( 'NONE', *, *, #861, .T. ) ;
#5374 = CARTESIAN_POINT ( 'NONE',  ( -14.65665288169999947, -79.50000000000000000, 36.94583914790000279 ) ) ;
#5375 = B_SPLINE_CURVE_WITH_KNOTS ( 'NONE', 5,
 ( #982, #22966, #18733, #19008, #16536, #16232, #5462, #7931, #27327 ),
 .UNSPECIFIED., .F., .F.,
 ( 6, 3, 6 ),
 ( 0.000000000000000000, 0.4480559759399665998, 1.000000000000000000 ),
 .UNSPECIFIED. ) ;
#5376 = CARTESIAN_POINT ( 'NONE',  ( -15.39899069939999876, -101.1262888790000005, 3.404061698440000061 ) ) ;
#5377 = CARTESIAN_POINT ( 'NONE',  ( 24.46716655439999855, -58.91551295370000219, 1.187497063919999984 ) ) ;
#5378 = CARTESIAN_POINT ( 'NONE',  ( 19.49373789020000203, -35.48172793740000230, -8.986332944369998188 ) ) ;
#5379 = ORIENTED_EDGE ( 'NONE', *, *, #3347, .T. ) ;
#5380 = DIRECTION ( 'NONE',  ( 0.000000000000000000, 1.000000000000000000, 0.000000000000000000 ) ) ;
#5381 = CARTESIAN_POINT ( 'NONE',  ( -2.776065240120000333, -18.86697026210000061, -23.72009294809999957 ) ) ;
#5382 = CARTESIAN_POINT ( 'NONE',  ( -7.900916432368809694, -99.99762666408553002, 15.39651926382340363 ) ) ;
#5383 = VERTEX_POINT ( 'NONE', #13860 ) ;
#5385 = EDGE_CURVE ( 'NONE', #20961, #23467, #14675, .T. ) ;
#5384 = CARTESIAN_POINT ( 'NONE',  ( -10.13149966729999818, -18.50000000000000000, 18.43352823549999897 ) ) ;
#5386 = CLOSED_SHELL ( 'NONE', ( #22330, #27929, #14692, #26645, #26893, #15039, #8994, #15195, #23394, #21803, #2739, #18801, #25258, #15430, #19, #17805, #6794, #3115, #3696, #2694, #26454, #1254, #3317, #5509, #1626, #16358, #15409, #11675, #26517, #27968, #9481, #8128, #18382, #5249, #27531, #28757, #4369, #7123, #2706, #23496, #24885 ) ) ;
#5387 = CARTESIAN_POINT ( 'NONE',  ( 22.43277176080000146, -36.00000000000000000, -11.31764183710000005 ) ) ;
#5388 = CARTESIAN_POINT ( 'NONE',  ( 16.00294200327352101, -100.9364580239705873, 4.239096016115913024 ) ) ;
#5389 = CARTESIAN_POINT ( 'NONE',  ( -3.967099564274365164, -72.37489743483658344, -28.45199697807708006 ) ) ;
#5390 = VERTEX_POINT ( 'NONE', #20573 ) ;
#5391 = ITEM_DEFINED_TRANSFORMATION ( 'NONE', 'NONE', #11059,  #26433 ) ;
#5392 = CARTESIAN_POINT ( 'NONE',  ( -12.45432576839999861, -65.00127508749999095, -21.87307312520000124 ) ) ;
#5393 = CARTESIAN_POINT ( 'NONE',  ( 24.54494471330000138, -66.27261548020000248, -9.685072589820000744 ) ) ;
#5394 = DIRECTION ( 'NONE',  ( 0.000000000000000000, 1.000000000000000000, 0.000000000000000000 ) ) ;
#5395 = VERTEX_POINT ( 'NONE', #25093 ) ;
#5396 = FACE_OUTER_BOUND ( 'NONE', #16286, .T. ) ;
#5397 = EDGE_LOOP ( 'NONE', ( #15207, #3040, #4793, #16185, #21265, #1792, #20713, #21293, #23823, #24151, #2363, #4560, #7405, #7400, #7676, #6927, #13790, #20899, #446, #20060, #124, #14419 ) ) ;
#5398 = CARTESIAN_POINT ( 'NONE',  ( -5.644564482089999835, -100.9763228559999959, 14.63128291989999852 ) ) ;
#5399 = ORIENTED_EDGE ( 'NONE', *, *, #17076, .F. ) ;
#5400 = DIRECTION ( 'NONE',  ( 0.4794255386042028944, 0.000000000000000000, -0.8775825618903727587 ) ) ;
#5401 = CARTESIAN_POINT ( 'NONE',  ( 26.77683864449999973, -15.80000000000000071, 49.01467436490000296 ) ) ;
#5402 = ADVANCED_FACE ( 'NONE', ( #5129 ), #21246, .T. ) ;
#5403 = ORIENTED_EDGE ( 'NONE', *, *, #21864, .T. ) ;
#5404 = FACE_OUTER_BOUND ( 'NONE', #13817, .T. ) ;
#5405 = LINE ( 'NONE', #18521, #5780 ) ;
#5406 = CARTESIAN_POINT ( 'NONE',  ( 13.12517053680000068, -93.00000000000000000, 27.53143473160000099 ) ) ;
#5407 = CARTESIAN_POINT ( 'NONE',  ( -11.65705697597267942, -61.40679450237151826, -22.99730055226696734 ) ) ;
#5408 = CARTESIAN_POINT ( 'NONE',  ( 47.19132921107751599, -79.33749027171297996, -1.164644976861414438 ) ) ;
#5409 = ORIENTED_EDGE ( 'NONE', *, *, #21080, .F. ) ;
#5410 = CARTESIAN_POINT ( 'NONE',  ( 12.43265749360000072, -93.67869433820000324, -21.69433720420000000 ) ) ;
#5411 = DIRECTION ( 'NONE',  ( 0.000000000000000000, 1.000000000000000000, 0.000000000000000000 ) ) ;
#5412 = CARTESIAN_POINT ( 'NONE',  ( -0.1723943457659999900, -101.6484611540000031, -15.49904126680000083 ) ) ;
#5413 = VERTEX_POINT ( 'NONE', #5048 ) ;
#5414 = CIRCLE ( 'NONE', #23545, 20.64285714289999873 ) ;
#5415 = CARTESIAN_POINT ( 'NONE',  ( 29.72661487340210229, -92.83160374581348151, 6.824835530513863269 ) ) ;
#5416 = CARTESIAN_POINT ( 'NONE',  ( -15.55828293390000105, -101.6484611540000031, 3.733608462140000306 ) ) ;
#5417 = ORIENTED_EDGE ( 'NONE', *, *, #17999, .F. ) ;
#5418 = DIRECTION ( 'NONE',  ( 0.09756097560976716154, 0.000000000000000000, -0.9952295494196655712 ) ) ;
#5419 = CARTESIAN_POINT ( 'NONE',  ( -19.24779671730000175, -32.69575302480000545, 13.93068917299999931 ) ) ;
#5420 = CARTESIAN_POINT ( 'NONE',  ( 27.68682485439999752, -24.80000000000000071, 50.68039294919999804 ) ) ;
#5421 = CARTESIAN_POINT ( 'NONE',  ( -38.20646596253030225, -65.72247384671339887, 1.295796974277947822 ) ) ;
#5422 = CARTESIAN_POINT ( 'NONE',  ( 22.18796890659999832, -59.03423364030000187, -7.691677767369998975 ) ) ;
#5423 = B_SPLINE_CURVE_WITH_KNOTS ( 'NONE', 3,
 ( #25467, #16859, #9996, #23557, #5498, #3323, #12454, #28071 ),
 .UNSPECIFIED., .F., .F.,
 ( 4, 2, 2, 4 ),
 ( 0.000000000000000000, 0.5000000000000066613, 0.7500000000000033307, 1.000000000000000000 ),
 .UNSPECIFIED. ) ;
#5424 = VERTEX_POINT ( 'NONE', #24872 ) ;
#5425 = B_SPLINE_CURVE_WITH_KNOTS ( 'NONE', 5,
 ( #17182, #17328, #6248, #5956, #3787, #19371, #26069, #3924, #12788 ),
 .UNSPECIFIED., .F., .F.,
 ( 6, 3, 6 ),
 ( 0.000000000000000000, 1.237573681340000009, 1.566718891470000097 ),
 .UNSPECIFIED. ) ;
#5426 = CARTESIAN_POINT ( 'NONE',  ( 8.681080848429999719, -37.64807918700000045, -21.92361636220000065 ) ) ;
#5427 = CARTESIAN_POINT ( 'NONE',  ( -19.73459501710000197, -19.50000000000000000, 14.41863426819999994 ) ) ;
#5428 = CARTESIAN_POINT ( 'NONE',  ( 21.61801161090000178, -37.04357994280000099, -8.573564459640000024 ) ) ;
#5429 = CARTESIAN_POINT ( 'NONE',  ( 19.83536304030000252, -94.71481430550001335, 14.13922876900000070 ) ) ;
#5430 = VERTEX_POINT ( 'NONE', #17877 ) ;
#5431 = DIRECTION ( 'NONE',  ( 0.000000000000000000, 1.000000000000000000, 0.000000000000000000 ) ) ;
#5432 = FACE_OUTER_BOUND ( 'NONE', #13858, .T. ) ;
#5433 = CARTESIAN_POINT ( 'NONE',  ( -17.11893731760000037, -92.49999999210000112, -23.95273848429999930 ) ) ;
#5434 = CARTESIAN_POINT ( 'NONE',  ( -7.720628919050000150, -100.8088109309999965, 14.63797111400000084 ) ) ;
#5435 = DIRECTION ( 'NONE',  ( 1.000000000000000000, 0.000000000000000000, 0.000000000000000000 ) ) ;
#5436 = DIRECTION ( 'NONE',  ( 1.000000000000000000, 0.000000000000000000, 0.000000000000000000 ) ) ;
#5437 = CARTESIAN_POINT ( 'NONE',  ( 7.594361522519999852, -101.6484612250000055, 14.08281941390000114 ) ) ;
#5438 = VERTEX_POINT ( 'NONE', #25013 ) ;
#5439 = EDGE_CURVE ( 'NONE', #7753, #13918, #15128, .T. ) ;
#5440 = CARTESIAN_POINT ( 'NONE',  ( -43.28930566789392032, -65.10053925468378111, 0.06637106439163820149 ) ) ;
#5441 = CARTESIAN_POINT ( 'NONE',  ( -40.65853658540000026, -84.00000000000000000, -6.717799458580000049 ) ) ;
#5442 = CARTESIAN_POINT ( 'NONE',  ( -13.15600360629633236, -19.48875933375592950, 19.82831268508771316 ) ) ;
#5443 = CARTESIAN_POINT ( 'NONE',  ( 11.11271058390000022, -96.95622423819999369, -17.69897580199999965 ) ) ;
#5444 = EDGE_LOOP ( 'NONE', ( #7006, #3460, #15268, #10356 ) ) ;
#5445 = B_SPLINE_CURVE_WITH_KNOTS ( 'NONE', 3,
 ( #6102, #1895, #10455, #3926 ),
 .UNSPECIFIED., .F., .F.,
 ( 4, 4 ),
 ( -4.007730545210000273, -3.491867373409999864 ),
 .UNSPECIFIED. ) ;
#5446 = CARTESIAN_POINT ( 'NONE',  ( 19.69582338720000081, -18.50000000000000000, -7.383548592259999488 ) ) ;
#5447 = ADVANCED_FACE ( 'NONE', ( #28781 ), #472, .T. ) ;
#5448 = FACE_OUTER_BOUND ( 'NONE', #12078, .T. ) ;
#5449 = CARTESIAN_POINT ( 'NONE',  ( -2.604257624009999716, -32.67314203990000010, -24.29262257289999738 ) ) ;
#5450 = CARTESIAN_POINT ( 'NONE',  ( 0.000000000000000000, -13.50000000000000000, 0.000000000000000000 ) ) ;
#5451 = EDGE_CURVE ( 'NONE', #3863, #5430, #15291, .T. ) ;
#5452 = CARTESIAN_POINT ( 'NONE',  ( -31.89935321680000158, -74.00000000000000000, -21.99985828019999801 ) ) ;
#5453 = CARTESIAN_POINT ( 'NONE',  ( 11.89727022614212615, -101.5620304352158314, -10.79529442988603272 ) ) ;
#5454 = CARTESIAN_POINT ( 'NONE',  ( 22.59227796120000065, -53.25913232239999928, -9.063833271410000947 ) ) ;
#5455 = CARTESIAN_POINT ( 'NONE',  ( 13.84987421219491921, -98.08323781429143651, 15.06242402452379636 ) ) ;
#5456 = CARTESIAN_POINT ( 'NONE',  ( 36.24656966590000451, -75.00000018780001199, -15.05817676390000059 ) ) ;
#5457 = ORIENTED_EDGE ( 'NONE', *, *, #11788, .T. ) ;
#5458 = CARTESIAN_POINT ( 'NONE',  ( 6.731493086280000426, -101.1411470200000053, 13.83935196010000013 ) ) ;
#5459 = DIRECTION ( 'NONE',  ( 0.000000000000000000, 1.000000000000000000, 0.000000000000000000 ) ) ;
#5460 = DIRECTION ( 'NONE',  ( 1.000000000000000000, 0.000000000000000000, 0.000000000000000000 ) ) ;
#5461 = CARTESIAN_POINT ( 'NONE',  ( 21.34788071859999903, -35.28814083279999636, -7.426814964410000108 ) ) ;
#5462 = CARTESIAN_POINT ( 'NONE',  ( 36.27185351749999853, -79.54415414250000538, -14.99731109350000047 ) ) ;
#5463 = CARTESIAN_POINT ( 'NONE',  ( 24.31651070795704683, -94.36683344927989481, -3.632850094172810795 ) ) ;
#5464 = DIRECTION ( 'NONE',  ( 1.000000000000000000, 0.000000000000000000, 0.000000000000000000 ) ) ;
#5465 = CARTESIAN_POINT ( 'NONE',  ( -11.35954001540000036, -79.50000000000000000, 47.25000000000000000 ) ) ;
#5466 = EDGE_LOOP ( 'NONE', ( #17632, #23870, #8907, #2180 ) ) ;
#5467 = CARTESIAN_POINT ( 'NONE',  ( -5.969238273050000210, -101.2530993000000024, 13.97222956270000083 ) ) ;
#5468 = FACE_OUTER_BOUND ( 'NONE', #6110, .T. ) ;
#5469 = EDGE_LOOP ( 'NONE', ( #3618, #13500, #604, #21670 ) ) ;
#5470 = LINE ( 'NONE', #7806, #27115 ) ;
#5471 = EDGE_LOOP ( 'NONE', ( #15527, #2597, #24869, #16148 ) ) ;
#5472 = ADVANCED_FACE ( 'NONE', ( #14374 ), #5621, .F. ) ;
#5473 = CARTESIAN_POINT ( 'NONE',  ( 0.6068588990009703421, -100.7538407677319583, -16.68821395358974158 ) ) ;
#5474 = CARTESIAN_POINT ( 'NONE',  ( 6.744238910220000882, -101.2530993010000060, 13.61507422070000040 ) ) ;
#5475 = CARTESIAN_POINT ( 'NONE',  ( 3.166345171159999694, -111.0000000000000000, -25.30265318609999881 ) ) ;
#5476 = CARTESIAN_POINT ( 'NONE',  ( -12.56240048859999803, -94.54647010769998872, -21.54391703350000142 ) ) ;
#5477 = AXIS2_PLACEMENT_3D ( 'NONE', #23785, #12688, #10631 ) ;
#5478 = EDGE_CURVE ( 'NONE', #7089, #22756, #20453, .T. ) ;
#5479 = FACE_OUTER_BOUND ( 'NONE', #13459, .T. ) ;
#5480 = CARTESIAN_POINT ( 'NONE',  ( 20.30102379280000235, -72.31415926540000783, -30.97095677779999789 ) ) ;
#5481 = ADVANCED_FACE ( 'NONE', ( #14505 ), #26970, .T. ) ;
#5482 = CARTESIAN_POINT ( 'NONE',  ( -21.23294764439999938, -65.91137168669999369, 14.52552031449999959 ) ) ;
#5483 = CARTESIAN_POINT ( 'NONE',  ( 12.82422680459999853, -94.98812477769999418, -19.93894967960000386 ) ) ;
#5484 = B_SPLINE_SURFACE_WITH_KNOTS ( 'NONE', 5, 5, ( 
 ( #14087, #5865, #9413, #19275, #3039, #10223, #23645, #13939, #21462 ),
 ( #22841, #20803, #2885, #27877, #11742, #18998, #20658, #9567, #857 ),
 ( #18466, #12408, #19135, #9701, #5729, #14615, #23517, #21320, #28024 ),
 ( #8322, #22179, #6288, #15154, #24064, #21602, #8469, #5998, #3826 ),
 ( #1658, #28707, #26266, #4403, #4103, #12973, #11062, #17225, #4252 ),
 ( #24362, #17664, #8747, #10923, #24218, #21886, #21739, #10777, #1789 ) ),
 .UNSPECIFIED., .F., .F., .F.,
 ( 6, 6 ),
 ( 6, 3, 6 ),
 ( 4.816191416749999732, 6.255250589900000158 ),
 ( 0.000000000000000000, 0.2500000000000000000, 0.5000000000000000000 ),
 .UNSPECIFIED. ) ;
#5485 = CARTESIAN_POINT ( 'NONE',  ( 0.000000000000000000, -23.00000000000000000, 0.000000000000000000 ) ) ;
#5486 = DIRECTION ( 'NONE',  ( 1.000000000000000000, 0.000000000000000000, 0.000000000000000000 ) ) ;
#5487 = CYLINDRICAL_SURFACE ( 'NONE', #8091, 3.749999999999996447 ) ;
#5488 = VERTEX_POINT ( 'NONE', #12025 ) ;
#5489 = CARTESIAN_POINT ( 'NONE',  ( -40.50000000000000000, -63.30468293320000583, -2.309401076760000393 ) ) ;
#5490 = ORIENTED_EDGE ( 'NONE', *, *, #10658, .T. ) ;
#5491 = CARTESIAN_POINT ( 'NONE',  ( -14.03261327740279896, -80.23900667062660830, 36.71350245345666252 ) ) ;
#5492 =( GEOMETRIC_REPRESENTATION_CONTEXT ( 3 ) GLOBAL_UNCERTAINTY_ASSIGNED_CONTEXT ( ( #25491 ) ) GLOBAL_UNIT_ASSIGNED_CONTEXT ( ( #18542, #22773, #9496 ) ) REPRESENTATION_CONTEXT ( 'NONE', 'WORKASPACE' ) );
#5493 = CARTESIAN_POINT ( 'NONE',  ( -28.52512532269999923, -92.54030566109999256, 3.253864596379999696 ) ) ;
#5494 = DIRECTION ( 'NONE',  ( -0.2414462220490755373, 0.000000000000000000, 0.9704142011833032377 ) ) ;
#5495 = ORIENTED_EDGE ( 'NONE', *, *, #8218, .T. ) ;
#5496 = CARTESIAN_POINT ( 'NONE',  ( -7.370698677632464779, -73.94611354405870429, 38.67409461690933625 ) ) ;
#5497 = ADVANCED_FACE ( 'NONE', ( #25169 ), #25731, .F. ) ;
#5498 = CARTESIAN_POINT ( 'NONE',  ( -7.479537002312467209, -74.09468416707295546, -39.31219897218396397 ) ) ;
#5499 = EDGE_LOOP ( 'NONE', ( #27834, #25020, #13822, #17521 ) ) ;
#5500 = CARTESIAN_POINT ( 'NONE',  ( 7.448284947614243201, -36.87977280728636487, -21.48523428999794760 ) ) ;
#5501 = CARTESIAN_POINT ( 'NONE',  ( -11.91368332737741831, -63.90944102351340916, 21.57903816910991779 ) ) ;
#5502 = EDGE_CURVE ( 'NONE', #15872, #14143, #23983, .T. ) ;
#5503 = AXIS2_PLACEMENT_3D ( 'NONE', #12322, #5771, #16568 ) ;
#5504 = CARTESIAN_POINT ( 'NONE',  ( -14.54237663339999997, -79.81382879129999708, 36.82469782859999441 ) ) ;
#5505 = VECTOR ( 'NONE', #23737, 1000.000000000000114 ) ;
#5506 = CARTESIAN_POINT ( 'NONE',  ( -3.778287650309999801, -69.97113394379999818, -28.14671785339999843 ) ) ;
#5507 = CARTESIAN_POINT ( 'NONE',  ( -13.83569956370000043, -69.21570870340001136, 23.22967513160000053 ) ) ;
#5508 = EDGE_LOOP ( 'NONE', ( #6566, #8171, #19223 ) ) ;
#5509 = ADVANCED_FACE ( 'NONE', ( #11740 ), #27504, .T. ) ;
#5510 = DIRECTION ( 'NONE',  ( 0.000000000000000000, 1.000000000000000000, 0.000000000000000000 ) ) ;
#5511 = CARTESIAN_POINT ( 'NONE',  ( -16.13804302950000036, -100.4011261050000030, 2.780960711030000088 ) ) ;
#5512 = CARTESIAN_POINT ( 'NONE',  ( 26.01008226429999937, -64.47176828549999072, 1.369137345940000028 ) ) ;
#5513 = CARTESIAN_POINT ( 'NONE',  ( -21.14183719079999690, -62.95300605010000083, 15.28077941859999989 ) ) ;
#5514 = ORIENTED_EDGE ( 'NONE', *, *, #21807, .F. ) ;
#5515 = AXIS2_PLACEMENT_3D ( 'NONE', #1902, #17923, #20102 ) ;
#5516 = CARTESIAN_POINT ( 'NONE',  ( -0.5268693940142937793, -39.36577620583297943, -22.72254148439001398 ) ) ;
#5517 = CARTESIAN_POINT ( 'NONE',  ( -7.282285323108220965, -73.99998672515624776, 39.66612828077759900 ) ) ;
#5518 = CARTESIAN_POINT ( 'NONE',  ( 36.38049338981862491, -74.01943097537444771, -13.95685178916381730 ) ) ;
#5519 = ORIENTED_EDGE ( 'NONE', *, *, #21645, .F. ) ;
#5520 = LINE ( 'NONE', #21254, #20990 ) ;
#5521 = CARTESIAN_POINT ( 'NONE',  ( -41.79927756528118721, -65.72601415636299294, -1.277196024497175175 ) ) ;
#5522 = CARTESIAN_POINT ( 'NONE',  ( 36.43808797039999803, -79.65546220359999552, -14.69303470340000040 ) ) ;
#5523 = CARTESIAN_POINT ( 'NONE',  ( 36.70830927769999619, -74.93175448689999030, -14.75000110549999910 ) ) ;
#5524 = ORIENTED_EDGE ( 'NONE', *, *, #18963, .T. ) ;
#5525 = CIRCLE ( 'NONE', #3647, 20.64285714289999873 ) ;
#5526 = CARTESIAN_POINT ( 'NONE',  ( -40.00000000000000000, -69.00000000000000000, 3.236300116779999679E-15 ) ) ;
#5527 = VERTEX_POINT ( 'NONE', #3171 ) ;
#5528 = CARTESIAN_POINT ( 'NONE',  ( -14.93121066289999987, -74.50000000000000000, 36.29905574720000061 ) ) ;
#5529 = LINE ( 'NONE', #1456, #18870 ) ;
#5530 = ORIENTED_EDGE ( 'NONE', *, *, #6133, .T. ) ;
#5531 = CARTESIAN_POINT ( 'NONE',  ( -11.00251064340000084, -27.06784995459999976, 19.39886944670000091 ) ) ;
#5532 = CARTESIAN_POINT ( 'NONE',  ( -6.058780266770000367, -101.6095085860000040, 14.84092105570000086 ) ) ;
#5533 = ORIENTED_EDGE ( 'NONE', *, *, #19654, .F. ) ;
#5534 = CARTESIAN_POINT ( 'NONE',  ( -2.580132123360000307, -54.50138674060000454, -25.16134040389999882 ) ) ;
#5535 = DIRECTION ( 'NONE',  ( 0.8775825618903722036, 0.000000000000000000, -0.4794255386042041156 ) ) ;
#5536 = EDGE_CURVE ( 'NONE', #22592, #3729, #4006, .T. ) ;
#5537 = CIRCLE ( 'NONE', #21361, 0.4999999999999983902 ) ;
#5538 = EDGE_CURVE ( 'NONE', #9851, #5109, #2137, .T. ) ;
#5539 = CARTESIAN_POINT ( 'NONE',  ( 39.03038279099999386, -74.00032110540000474, 7.562806955190000124 ) ) ;
#5540 = CARTESIAN_POINT ( 'NONE',  ( 0.000000000000000000, -34.10310889129999623, 0.000000000000000000 ) ) ;
#5541 = ADVANCED_FACE ( 'NONE', ( #18756 ), #21220, .F. ) ;
#5542 = DIRECTION ( 'NONE',  ( 0.000000000000000000, -1.000000000000000000, 0.000000000000000000 ) ) ;
#5543 = CARTESIAN_POINT ( 'NONE',  ( -10.35605037799999906, -12.64149019679999952, -18.95662306240000206 ) ) ;
#5544 = ORIENTED_EDGE ( 'NONE', *, *, #19790, .F. ) ;
#5545 = CIRCLE ( 'NONE', #12498, 9.099999999999999645 ) ;
#5546 = AXIS2_PLACEMENT_3D ( 'NONE', #10523, #12578, #21350 ) ;
#5547 = CARTESIAN_POINT ( 'NONE',  ( -32.68889462130000112, -80.00000031659999422, -22.56856178450000172 ) ) ;
#5548 = CARTESIAN_POINT ( 'NONE',  ( 10.08508256729999886, -64.24504434620000382, -24.78974309399999854 ) ) ;
#5549 = CIRCLE ( 'NONE', #6945, 3.499999999999999556 ) ;
#5550 = CARTESIAN_POINT ( 'NONE',  ( -20.41940881060000024, -94.07621218059999535, 14.28684394100000077 ) ) ;
#5551 = CARTESIAN_POINT ( 'NONE',  ( -34.11790219230000076, -79.50000000000000000, -24.21840725559999896 ) ) ;
#5552 = ORIENTED_EDGE ( 'NONE', *, *, #13996, .T. ) ;
#5553 = CIRCLE ( 'NONE', #7408, 0.4999999999999982236 ) ;
#5554 = CARTESIAN_POINT ( 'NONE',  ( 29.70837229499504772, -92.96960399592401814, 6.903811671076394596 ) ) ;
#5555 = VERTEX_POINT ( 'NONE', #9565 ) ;
#5556 = FACE_OUTER_BOUND ( 'NONE', #3180, .T. ) ;
#5557 = DIRECTION ( 'NONE',  ( 0.000000000000000000, 1.000000000000000000, 0.000000000000000000 ) ) ;
#5558 = CARTESIAN_POINT ( 'NONE',  ( -7.879410208250000380, -99.92967571559999840, 15.46934584979999983 ) ) ;
#5559 = CARTESIAN_POINT ( 'NONE',  ( -38.25000000000000000, -65.63577453799999262, 1.587713240270000048 ) ) ;
#5560 = DIRECTION ( 'NONE',  ( 0.000000000000000000, -1.000000000000000000, 0.000000000000000000 ) ) ;
#5561 = ADVANCED_FACE ( 'NONE', ( #25455 ), #23265, .F. ) ;
#5562 = DIRECTION ( 'NONE',  ( 0.000000000000000000, 0.000000000000000000, 1.000000000000000000 ) ) ;
#5563 = CARTESIAN_POINT ( 'NONE',  ( -10.90352314479999940, -18.50000000000000000, 18.09320272940000152 ) ) ;
#5564 = AXIS2_PLACEMENT_3D ( 'NONE', #28647, #13348, #24438 ) ;
#5565 = CIRCLE ( 'NONE', #9272, 6.750000000000002665 ) ;
#5566 = AXIS2_PLACEMENT_3D ( 'NONE', #6868, #10909, #19964 ) ;
#5567 = VERTEX_POINT ( 'NONE', #21087 ) ;
#5568 = DIRECTION ( 'NONE',  ( 1.000000000000000000, 0.000000000000000000, 0.000000000000000000 ) ) ;
#5569 = CARTESIAN_POINT ( 'NONE',  ( 20.10924407270000103, -35.62996179179999245, -8.973978175680001002 ) ) ;
#5570 = DIRECTION ( 'NONE',  ( -0.8476796612309128731, -0.2588190451029734884, -0.4630895095199519806 ) ) ;
#5571 = ORIENTED_EDGE ( 'NONE', *, *, #17538, .F. ) ;
#5572 = CARTESIAN_POINT ( 'NONE',  ( -13.14571786560000000, -100.8733988930000010, -8.628954981190000595 ) ) ;
#5573 = EDGE_CURVE ( 'NONE', #28180, #5596, #8178, .T. ) ;
#5574 = CARTESIAN_POINT ( 'NONE',  ( -16.01759400379999931, -69.30633957129998635, 23.18138418170000037 ) ) ;
#5575 = CARTESIAN_POINT ( 'NONE',  ( -7.722863872719999634, -100.5717442099999914, 14.38966742470000071 ) ) ;
#5576 = CARTESIAN_POINT ( 'NONE',  ( 40.00000000000000000, -82.25000000000000000, 0.000000000000000000 ) ) ;
#5577 = DIRECTION ( 'NONE',  ( 0.000000000000000000, 1.000000000000000000, 0.000000000000000000 ) ) ;
#5578 = CARTESIAN_POINT ( 'NONE',  ( 7.320076657800000497, -101.1409265030000029, 13.53711875870000192 ) ) ;
#5579 = ORIENTED_EDGE ( 'NONE', *, *, #17076, .T. ) ;
#5580 = CARTESIAN_POINT ( 'NONE',  ( -43.22668651970722209, -65.13491442161374323, -0.1557320299099214655 ) ) ;
#5581 = CARTESIAN_POINT ( 'NONE',  ( -27.06659278359999732, -93.14733690340000294, -4.203927835110000011 ) ) ;
#5582 = DIRECTION ( 'NONE',  ( 0.000000000000000000, -1.000000000000000000, 0.000000000000000000 ) ) ;
#5583 = ORIENTED_EDGE ( 'NONE', *, *, #19697, .T. ) ;
#5584 = CARTESIAN_POINT ( 'NONE',  ( 19.82501711970000002, -19.48264111129999776, -8.815784396710000692 ) ) ;
#5585 = CARTESIAN_POINT ( 'NONE',  ( 11.67565778989999892, -101.1292389600000092, -10.20417835260000139 ) ) ;
#5586 = CARTESIAN_POINT ( 'NONE',  ( -17.54428591559999973, -94.59275927410000406, 16.07756161280000029 ) ) ;
#5587 = DIRECTION ( 'NONE',  ( -1.836909530729999990E-16, 0.000000000000000000, 1.000000000000000000 ) ) ;
#5588 = AXIS2_PLACEMENT_3D ( 'NONE', #13392, #6714, #22452 ) ;
#5589 = AXIS2_PLACEMENT_3D ( 'NONE', #24592, #20361, #432 ) ;
#5590 = FACE_OUTER_BOUND ( 'NONE', #25541, .T. ) ;
#5591 = B_SPLINE_CURVE_WITH_KNOTS ( 'NONE', 5,
 ( #24838, #18430, #679, #9379, #16081, #12137, #5015, #974, #9814, #11704, #16527, #825 ),
 .UNSPECIFIED., .F., .F.,
 ( 6, 3, 3, 6 ),
 ( -7.896981424030000696, -6.690827956829999756, -5.319894352600000431, -3.365447998909999683 ),
 .UNSPECIFIED. ) ;
#5592 = CARTESIAN_POINT ( 'NONE',  ( 8.985156090609999424, -35.55399656489999671, -19.52064371570000034 ) ) ;
#5593 = CARTESIAN_POINT ( 'NONE',  ( 22.62696043789999933, -36.51121532250000001, -9.295214654749999639 ) ) ;
#5594 = CARTESIAN_POINT ( 'NONE',  ( 13.67893538235999529, -98.17437103743534976, 15.05775980708956219 ) ) ;
#5595 = CARTESIAN_POINT ( 'NONE',  ( -10.60846119319999836, -27.03158754559999721, -21.08535220339999938 ) ) ;
#5596 = VERTEX_POINT ( 'NONE', #9984 ) ;
#5597 = EDGE_CURVE ( 'NONE', #26341, #26269, #8647, .T. ) ;
#5598 = CARTESIAN_POINT ( 'NONE',  ( -32.72710940640000388, -74.40224539360001188, -22.12820698629999683 ) ) ;
#5599 = FACE_OUTER_BOUND ( 'NONE', #28204, .T. ) ;
#5600 = CARTESIAN_POINT ( 'NONE',  ( -11.73664997740000082, -94.54719592029999831, -20.76900810619999760 ) ) ;
#5601 = CARTESIAN_POINT ( 'NONE',  ( 8.973973756419999503, -35.62994960090000518, -20.10924160899999791 ) ) ;
#5602 = CARTESIAN_POINT ( 'NONE',  ( 6.019093083229999586, -92.50000000000000000, 29.30685818879999971 ) ) ;
#5603 = ADVANCED_FACE ( 'NONE', ( #7820 ), #5761, .T. ) ;
#5604 = CARTESIAN_POINT ( 'NONE',  ( 7.105427357599999217E-15, -74.50000000000000000, 3.552713678799999608E-15 ) ) ;
#5605 = TOROIDAL_SURFACE ( 'NONE', #18166, 38.75000000000000000, 0.5000000000000000000 ) ;
#5606 = CARTESIAN_POINT ( 'NONE',  ( -19.96485215072167563, -93.12686943432630926, -20.78016349561067599 ) ) ;
#5607 = VECTOR ( 'NONE', #2976, 1000.000000000000000 ) ;
#5608 = ORIENTED_EDGE ( 'NONE', *, *, #24373, .F. ) ;
#5609 = CARTESIAN_POINT ( 'NONE',  ( -5.774731795730000172, -101.2530993039999885, 14.05532693159999980 ) ) ;
#5610 = CARTESIAN_POINT ( 'NONE',  ( -12.17175180279999935, -57.47855601759999900, -19.93971687999999887 ) ) ;
#5611 = ORIENTED_EDGE ( 'NONE', *, *, #12604, .T. ) ;
#5612 = DIRECTION ( 'NONE',  ( 0.000000000000000000, 1.000000000000000000, 0.000000000000000000 ) ) ;
#5613 = CARTESIAN_POINT ( 'NONE',  ( 0.5718234277215632488, -100.9364580247160177, -16.54500244008519161 ) ) ;
#5614 = DIRECTION ( 'NONE',  ( 1.000000000000000000, 0.000000000000000000, 0.000000000000000000 ) ) ;
#5615 = CARTESIAN_POINT ( 'NONE',  ( 13.45309085318943687, -92.66191076889870715, 27.37276729370756101 ) ) ;
#5616 = CARTESIAN_POINT ( 'NONE',  ( 25.16314806569999973, -73.44383031769999093, -29.90446131310000055 ) ) ;
#5617 = CARTESIAN_POINT ( 'NONE',  ( 0.000000000000000000, -22.69689110870000093, 0.000000000000000000 ) ) ;
#5618 = CARTESIAN_POINT ( 'NONE',  ( 23.87439762153048761, -92.83865970264375278, -18.98059930716613408 ) ) ;
#5619 = DIRECTION ( 'NONE',  ( 1.000000000000000000, 0.000000000000000000, 0.000000000000000000 ) ) ;
#5620 = CARTESIAN_POINT ( 'NONE',  ( 8.528659902539999393, -19.44973803559999936, -20.19953053829999945 ) ) ;
#5621 = CYLINDRICAL_SURFACE ( 'NONE', #6962, 0.5000000000000025535 ) ;
#5622 = CARTESIAN_POINT ( 'NONE',  ( -41.61800135853595606, -63.05366291736181950, 2.876043459062908259 ) ) ;
#5623 = AXIS2_PLACEMENT_3D ( 'NONE', #11433, #557, #9402 ) ;
#5624 = ORIENTED_EDGE ( 'NONE', *, *, #15617, .T. ) ;
#5625 = AXIS2_PLACEMENT_3D ( 'NONE', #9053, #2374, #19834 ) ;
#5626 = DIRECTION ( 'NONE',  ( 0.4151946956541399669, 0.5000000000001689759, 0.7600087925152558821 ) ) ;
#5627 = AXIS2_PLACEMENT_3D ( 'NONE', #24435, #17447, #17149 ) ;
#5628 = VERTEX_POINT ( 'NONE', #17410 ) ;
#5629 = PRODUCT_RELATED_PRODUCT_CATEGORY ( 'part', '', ( #3620 ) ) ;
#5630 = EDGE_CURVE ( 'NONE', #24400, #20739, #25871, .T. ) ;
#5631 = CARTESIAN_POINT ( 'NONE',  ( -14.19188855770000046, -80.00000000000000000, 37.13021410070000883 ) ) ;
#5632 = EDGE_CURVE ( 'NONE', #28507, #24612, #6327, .T. ) ;
#5633 = CARTESIAN_POINT ( 'NONE',  ( -44.38791280949999418, -66.25000000000000000, -2.397127693020000283 ) ) ;
#5634 = DIRECTION ( 'NONE',  ( -0.4299718839438681495, 0.000000000000000000, 0.9028422780407223680 ) ) ;
#5635 = EDGE_CURVE ( 'NONE', #1856, #14426, #5847, .T. ) ;
#5636 = VERTEX_POINT ( 'NONE', #8645 ) ;
#5637 = DIRECTION ( 'NONE',  ( 0.000000000000000000, -1.000000000000000000, 0.000000000000000000 ) ) ;
#5638 = DIRECTION ( 'NONE',  ( 0.000000000000000000, 1.000000000000000000, 0.000000000000000000 ) ) ;
#5639 = ORIENTED_EDGE ( 'NONE', *, *, #1141, .T. ) ;
#5640 = CIRCLE ( 'NONE', #9355, 0.4999999999999993894 ) ;
#5641 = CARTESIAN_POINT ( 'NONE',  ( 8.034824971200507093, -66.63181019764634527, -24.57972119927973154 ) ) ;
#5642 = CARTESIAN_POINT ( 'NONE',  ( 7.461111551219999249, -36.92670964950000467, -21.48614944720000253 ) ) ;
#5643 = CIRCLE ( 'NONE', #1455, 16.00000000000000000 ) ;
#5644 = CARTESIAN_POINT ( 'NONE',  ( 21.98941332900000134, -49.11505549560000361, -6.974892859150000568 ) ) ;
#5645 = CARTESIAN_POINT ( 'NONE',  ( -40.00000000000000000, -67.00000000000000000, 0.000000000000000000 ) ) ;
#5646 = CARTESIAN_POINT ( 'NONE',  ( -22.10465418478271005, -74.05401792490640389, -32.32543926652451916 ) ) ;
#5647 = ORIENTED_EDGE ( 'NONE', *, *, #21146, .F. ) ;
#5648 = CARTESIAN_POINT ( 'NONE',  ( -14.79093856799999962, -101.1411468629999888, 4.252364208789999545 ) ) ;
#5649 = CARTESIAN_POINT ( 'NONE',  ( -16.73274653779999710, -100.1461833709999922, 3.179024074209999995 ) ) ;
#5650 = LINE ( 'NONE', #17140, #12716 ) ;
#5651 = CARTESIAN_POINT ( 'NONE',  ( 19.49202744680000166, -35.46335013489999710, -8.986408038590001368 ) ) ;
#5652 = B_SPLINE_SURFACE_WITH_KNOTS ( 'NONE', 5, 5, ( 
 ( #12388, #19387, #10334, #28265, #28001, #8038 ),
 ( #5842, #23621, #23905, #25950, #19522, #19250 ),
 ( #26090, #6119, #17058, #14859, #28408, #6266 ),
 ( #23762, #15131, #7011, #4517, #13394, #6861 ),
 ( #19949, #19806, #20111, #22298, #22455, #1910 ),
 ( #4379, #10754, #24192, #13546, #179, #13703 ) ),
 .UNSPECIFIED., .F., .F., .F.,
 ( 6, 6 ),
 ( 6, 6 ),
 ( 0.000000000000000000, 11.23209334890000122 ),
 ( 0.000000000000000000, 0.5000000000000000000 ),
 .UNSPECIFIED. ) ;
#5653 = ORIENTED_EDGE ( 'NONE', *, *, #3160, .T. ) ;
#5654 = DIRECTION ( 'NONE',  ( 1.000000000000000000, 0.000000000000000000, 0.000000000000000000 ) ) ;
#5655 = CARTESIAN_POINT ( 'NONE',  ( -3.024786108369999837, -18.62181730670000235, -23.68429331439999785 ) ) ;
#5656 = CARTESIAN_POINT ( 'NONE',  ( 36.74383121569999844, -74.66666669110000498, -14.69280905019999928 ) ) ;
#5657 = ORIENTED_EDGE ( 'NONE', *, *, #6406, .T. ) ;
#5658 = CARTESIAN_POINT ( 'NONE',  ( 36.24656994149999889, -79.00000000000000000, -15.05817610060000078 ) ) ;
#5659 = CARTESIAN_POINT ( 'NONE',  ( 14.05983645159999895, -99.53431386179998697, -10.27466725399999881 ) ) ;
#5660 = ORIENTED_EDGE ( 'NONE', *, *, #27726, .T. ) ;
#5661 = AXIS2_PLACEMENT_3D ( 'NONE', #12240, #21154, #9772 ) ;
#5662 = AXIS2_PLACEMENT_3D ( 'NONE', #24920, #20543, #9457 ) ;
#5663 = EDGE_CURVE ( 'NONE', #1700, #21528, #24960, .T. ) ;
#5664 = B_SPLINE_CURVE_WITH_KNOTS ( 'NONE', 5,
 ( #11651, #14000, #11807, #14151, #630, #26980 ),
 .UNSPECIFIED., .F., .F.,
 ( 6, 6 ),
 ( 0.000000000000000000, 1.000000000000000000 ),
 .UNSPECIFIED. ) ;
#5665 = CARTESIAN_POINT ( 'NONE',  ( 6.819379226960565532, -100.4166221066960816, 15.53723975361173082 ) ) ;
#5666 = CARTESIAN_POINT ( 'NONE',  ( -2.682509845957436134, -80.39326405337963877, 46.73547856321033578 ) ) ;
#5667 = EDGE_CURVE ( 'NONE', #4274, #11243, #18912, .T. ) ;
#5668 = VERTEX_POINT ( 'NONE', #9084 ) ;
#5669 = CARTESIAN_POINT ( 'NONE',  ( -18.29991037700670731, -98.29443223157012710, 5.167542575955573092 ) ) ;
#5670 = ORIENTED_EDGE ( 'NONE', *, *, #16717, .F. ) ;
#5671 = CARTESIAN_POINT ( 'NONE',  ( 29.52540666350000365, -92.92146929989999649, 7.168157270950000104 ) ) ;
#5672 = CARTESIAN_POINT ( 'NONE',  ( -6.091977122730000360, -101.1292389600000092, 14.25952507679999925 ) ) ;
#5673 = ORIENTED_EDGE ( 'NONE', *, *, #5439, .F. ) ;
#5674 = CARTESIAN_POINT ( 'NONE',  ( -41.74999999999813127, -63.33820666349189565, 1.401515418006119118 ) ) ;
#5675 = CARTESIAN_POINT ( 'NONE',  ( -17.94180966909999597, -19.50000000000000000, 18.81731824139999887 ) ) ;
#5676 = DIRECTION ( 'NONE',  ( 1.000000000000000000, 0.000000000000000000, 0.000000000000000000 ) ) ;
#5677 = DIRECTION ( 'NONE',  ( 0.000000000000000000, 1.000000000000000000, 0.000000000000000000 ) ) ;
#5678 = DIRECTION ( 'NONE',  ( 0.000000000000000000, 1.000000000000000000, 0.000000000000000000 ) ) ;
#5679 = CONICAL_SURFACE ( 'NONE', #7583, 55.67692378859999280, 1.047197551199999799 ) ;
#5680 = CARTESIAN_POINT ( 'NONE',  ( 46.55834487451462422, -79.96456861975623553, -3.902750372498239084 ) ) ;
#5681 = VERTEX_POINT ( 'NONE', #13756 ) ;
#5682 = CARTESIAN_POINT ( 'NONE',  ( -16.86248238029999769, -97.53592492889998766, -10.88383597820000048 ) ) ;
#5683 = CARTESIAN_POINT ( 'NONE',  ( 19.83108000150000194, -97.73638926309999420, 2.238875083469999971 ) ) ;
#5684 = CARTESIAN_POINT ( 'NONE',  ( -20.44007416299999846, -93.36538189280000211, 16.34753294749999952 ) ) ;
#5685 = CARTESIAN_POINT ( 'NONE',  ( 15.94061401059999916, -100.1275643909999928, 4.799433088389999824 ) ) ;
#5686 = CARTESIAN_POINT ( 'NONE',  ( -1.986940095230000036, -55.03616289790000593, -23.76239100950000349 ) ) ;
#5687 = CARTESIAN_POINT ( 'NONE',  ( -3.562216359109999786, -80.34292033629999708, 46.31451622120000167 ) ) ;
#5688 = CARTESIAN_POINT ( 'NONE',  ( 0.000000000000000000, -15.80000000000000071, 0.000000000000000000 ) ) ;
#5689 = VERTEX_POINT ( 'NONE', #19864 ) ;
#5690 = LINE ( 'NONE', #25390, #19752 ) ;
#5691 = CARTESIAN_POINT ( 'NONE',  ( 20.58461438809549193, -97.38870237790757756, 1.320766927699984938 ) ) ;
#5692 = CARTESIAN_POINT ( 'NONE',  ( 27.75394116159999669, -74.50000000000000000, -27.75394116159999669 ) ) ;
#5693 = DIRECTION ( 'NONE',  ( 1.000000000000000000, 0.000000000000000000, 0.000000000000000000 ) ) ;
#5694 = DIRECTION ( 'NONE',  ( -0.8775825618903722036, 0.000000000000000000, 0.4794255386042041156 ) ) ;
#5695 = ADVANCED_FACE ( 'NONE', ( #15334 ), #4725, .T. ) ;
#5696 = CIRCLE ( 'NONE', #21976, 18.64285714289999873 ) ;
#5697 =( LENGTH_UNIT ( ) NAMED_UNIT ( * ) SI_UNIT ( .MILLI., .METRE. ) );
#5698 = DIRECTION ( 'NONE',  ( 0.000000000000000000, -1.000000000000000000, 0.000000000000000000 ) ) ;
#5699 = ADVANCED_FACE ( 'NONE', ( #22657 ), #27026, .T. ) ;
#5700 = AXIS2_PLACEMENT_3D ( 'NONE', #948, #23344, #8232 ) ;
#5701 = ORIENTED_EDGE ( 'NONE', *, *, #10987, .T. ) ;
#5702 = CARTESIAN_POINT ( 'NONE',  ( -39.97648509736585964, -73.96150430845531787, -7.250349464191292448 ) ) ;
#5703 = CARTESIAN_POINT ( 'NONE',  ( 19.72731272460000085, -94.57749834670001121, 14.01461188380000067 ) ) ;
#5704 = ORIENTED_EDGE ( 'NONE', *, *, #28715, .F. ) ;
#5705 = CARTESIAN_POINT ( 'NONE',  ( -12.86848417080000040, -101.1499348409999897, -9.082804019830000186 ) ) ;
#5706 = PRODUCT_DEFINITION_SHAPE ( 'NONE', 'NONE',  #1029 ) ;
#5707 = CARTESIAN_POINT ( 'NONE',  ( -16.72250540970000188, -71.11599492770000097, 23.42677820880000183 ) ) ;
#5708 = ORIENTED_EDGE ( 'NONE', *, *, #8688, .F. ) ;
#5709 = CARTESIAN_POINT ( 'NONE',  ( -1.247128410550000011, -101.2306304600000004, -16.16540378150000024 ) ) ;
#5710 = CARTESIAN_POINT ( 'NONE',  ( 37.60355029590000697, -84.00000000000000000, -9.356041104380000917 ) ) ;
#5711 = CARTESIAN_POINT ( 'NONE',  ( 7.547750227499999909, -101.3256028069999957, 14.00193654699999968 ) ) ;
#5712 = ORIENTED_EDGE ( 'NONE', *, *, #12805, .T. ) ;
#5713 = CARTESIAN_POINT ( 'NONE',  ( -40.29089741864007834, -74.18137224046458300, 7.244162156032251332 ) ) ;
#5714 = EDGE_CURVE ( 'NONE', #4093, #20809, #17986, .T. ) ;
#5715 = CARTESIAN_POINT ( 'NONE',  ( 46.75000000000000000, -69.50000000000000000, 7.285566699530000990E-15 ) ) ;
#5716 = DIRECTION ( 'NONE',  ( 0.000000000000000000, -1.000000000000000000, 0.000000000000000000 ) ) ;
#5717 = VERTEX_POINT ( 'NONE', #4577 ) ;
#5718 = CARTESIAN_POINT ( 'NONE',  ( 20.46648349389999666, -19.16110312220000012, -8.147944065169999917 ) ) ;
#5719 = VECTOR ( 'NONE', #23042, 1000.000000000000000 ) ;
#5720 = CARTESIAN_POINT ( 'NONE',  ( 11.30123137200000016, -101.2530993039999885, -10.15784976960000030 ) ) ;
#5721 = CIRCLE ( 'NONE', #3848, 3.500000000000003109 ) ;
#5722 = CARTESIAN_POINT ( 'NONE',  ( -14.64093407760000076, -74.15747494800001505, 36.27438844899999992 ) ) ;
#5723 = CARTESIAN_POINT ( 'NONE',  ( -18.26810282299999955, -94.98812129370000434, 16.32728610020000204 ) ) ;
#5724 = CARTESIAN_POINT ( 'NONE',  ( 10.20110288159999890, -84.50000000000000000, -41.00000000000000000 ) ) ;
#5725 = VERTEX_POINT ( 'NONE', #18282 ) ;
#5726 = CARTESIAN_POINT ( 'NONE',  ( 14.28941763439999946, -101.1889999979999999, -3.575252188409999921 ) ) ;
#5727 = DIRECTION ( 'NONE',  ( 0.000000000000000000, 1.000000000000000000, 0.000000000000000000 ) ) ;
#5728 = CARTESIAN_POINT ( 'NONE',  ( 22.16162922080000186, -57.47158989559999753, -7.992697997670000554 ) ) ;
#5729 = CARTESIAN_POINT ( 'NONE',  ( 15.59036279620000087, -101.1042759770000004, 2.486817442600000039 ) ) ;
#5730 = CARTESIAN_POINT ( 'NONE',  ( 6.846103682120000755, -36.12241484350000320, -21.55427193710000111 ) ) ;
#5731 = LINE ( 'NONE', #28292, #20142 ) ;
#5732 = ORIENTED_EDGE ( 'NONE', *, *, #18953, .F. ) ;
#5733 = EDGE_CURVE ( 'NONE', #8975, #15620, #16574, .T. ) ;
#5734 = EDGE_CURVE ( 'NONE', #5266, #12283, #3019, .T. ) ;
#5735 = CARTESIAN_POINT ( 'NONE',  ( 6.228305304889999228, -100.7707614970000094, 14.58014589510000114 ) ) ;
#5736 = LINE ( 'NONE', #14620, #27138 ) ;
#5737 = AXIS2_PLACEMENT_3D ( 'NONE', #15960, #22830, #18456 ) ;
#5738 = CARTESIAN_POINT ( 'NONE',  ( 7.653117467020000397, -101.1929016639999901, 13.21760603179999904 ) ) ;
#5739 = CARTESIAN_POINT ( 'NONE',  ( -11.77049225210000039, -94.59276583640000524, -20.68202189790000034 ) ) ;
#5740 = CARTESIAN_POINT ( 'NONE',  ( 8.770435879989999961, -35.38531427019999853, -20.52569411800000054 ) ) ;
#5741 = CARTESIAN_POINT ( 'NONE',  ( 7.219194746714282296, -73.62392792451103674, 39.33235237968798259 ) ) ;
#5742 = B_SPLINE_CURVE_WITH_KNOTS ( 'NONE', 3,
 ( #950, #3259, #12112, #12523 ),
 .UNSPECIFIED., .F., .F.,
 ( 4, 4 ),
 ( -0.1274251584810000004, 0.000000000000000000 ),
 .UNSPECIFIED. ) ;
#5743 = CARTESIAN_POINT ( 'NONE',  ( 26.16322034310070421, -93.20709273739696243, -8.388943539576686703 ) ) ;
#5744 = AXIS2_PLACEMENT_3D ( 'NONE', #11650, #20560, #330 ) ;
#5745 = CARTESIAN_POINT ( 'NONE',  ( 7.694095999870000036, -93.61368346389998862, -24.10127357489999866 ) ) ;
#5746 = VERTEX_POINT ( 'NONE', #18864 ) ;
#5747 = CARTESIAN_POINT ( 'NONE',  ( -16.99294773969999994, -99.88067626670000720, 3.462731254189999941 ) ) ;
#5748 = ORIENTED_EDGE ( 'NONE', *, *, #19002, .F. ) ;
#5749 = CARTESIAN_POINT ( 'NONE',  ( -1.314504061159999897E-13, -19.46510050329999686, -1.119104808819999722E-13 ) ) ;
#5750 = ORIENTED_EDGE ( 'NONE', *, *, #12855, .T. ) ;
#5751 = CARTESIAN_POINT ( 'NONE',  ( 0.4754459893910686907, -101.1884902310534358, -16.35008640957526183 ) ) ;
#5752 = ADVANCED_FACE ( 'NONE', ( #14048 ), #4507, .T. ) ;
#5753 = CARTESIAN_POINT ( 'NONE',  ( 6.390838521760000113, -101.2010924020000004, 13.85940160760000062 ) ) ;
#5754 = VECTOR ( 'NONE', #3853, 1000.000000000000000 ) ;
#5755 = CARTESIAN_POINT ( 'NONE',  ( 13.32851355232033441, -92.72722989462353382, 27.43357149820718632 ) ) ;
#5756 = CARTESIAN_POINT ( 'NONE',  ( 40.00000000000000000, -73.00000000000000000, 2.433892081919999696E-15 ) ) ;
#5757 = CARTESIAN_POINT ( 'NONE',  ( 25.11727467239999712, -73.66811105200000043, -29.97254555069999782 ) ) ;
#5758 = CARTESIAN_POINT ( 'NONE',  ( -22.07768936720000141, -67.34374581909999335, 16.43776412940000142 ) ) ;
#5759 = CARTESIAN_POINT ( 'NONE',  ( 18.39097424218846299, -93.63284908709232468, 17.05711033620115558 ) ) ;
#5760 = CARTESIAN_POINT ( 'NONE',  ( -18.49356544879450581, -19.46625705890763669, 12.40291896993568699 ) ) ;
#5761 = CYLINDRICAL_SURFACE ( 'NONE', #19797, 0.7500000000000004441 ) ;
#5762 = CIRCLE ( 'NONE', #16460, 55.67692378859999991 ) ;
#5763 = DIRECTION ( 'NONE',  ( 1.836909530730000976E-16, 0.000000000000000000, -1.000000000000000000 ) ) ;
#5764 = ORIENTED_EDGE ( 'NONE', *, *, #7429, .F. ) ;
#5765 = CARTESIAN_POINT ( 'NONE',  ( -10.94986905363052543, -44.38603308081882659, 20.11695812405464068 ) ) ;
#5766 = ORIENTED_EDGE ( 'NONE', *, *, #18134, .F. ) ;
#5767 = AXIS2_PLACEMENT_3D ( 'NONE', #28250, #15113, #19646 ) ;
#5768 = CARTESIAN_POINT ( 'NONE',  ( -0.5578430832430000263, -60.34941021230000047, -23.62008496760000043 ) ) ;
#5769 = CIRCLE ( 'NONE', #25328, 38.75000000000000000 ) ;
#5770 = DIRECTION ( 'NONE',  ( 0.7175736280288005364, 0.000000000000000000, -0.6964826547428046855 ) ) ;
#5771 = DIRECTION ( 'NONE',  ( 0.000000000000000000, 1.000000000000000000, 0.000000000000000000 ) ) ;
#5772 = ORIENTED_EDGE ( 'NONE', *, *, #1133, .F. ) ;
#5773 = CARTESIAN_POINT ( 'NONE',  ( -15.00047198269999882, -74.50000000000000000, 39.16845525979999820 ) ) ;
#5774 = ORIENTED_EDGE ( 'NONE', *, *, #18225, .F. ) ;
#5775 = CONICAL_SURFACE ( 'NONE', #24864, 7.000000000000005329, 0.7853981633970000820 ) ;
#5776 = CARTESIAN_POINT ( 'NONE',  ( 9.718892398710000435, -111.0000000000000000, 28.91008700340000104 ) ) ;
#5777 = CARTESIAN_POINT ( 'NONE',  ( 7.532037665939999904, -37.10289230739999766, -21.49296857539999905 ) ) ;
#5778 = ORIENTED_EDGE ( 'NONE', *, *, #5282, .F. ) ;
#5779 = ADVANCED_FACE ( 'NONE', ( #19274 ), #14250, .F. ) ;
#5780 = VECTOR ( 'NONE', #13998, 999.9999999999998863 ) ;
#5781 = CARTESIAN_POINT ( 'NONE',  ( -17.73582829829999952, -18.50000000000000000, 11.34636642620000124 ) ) ;
#5782 = ORIENTED_EDGE ( 'NONE', *, *, #3942, .F. ) ;
#5783 = EDGE_CURVE ( 'NONE', #28456, #17366, #23644, .T. ) ;
#5784 = CARTESIAN_POINT ( 'NONE',  ( -22.24124310690000073, -94.63960343439998724, -8.291373264160000645 ) ) ;
#5785 = CARTESIAN_POINT ( 'NONE',  ( -15.54748971619999942, -100.8069964150000004, 2.643158339580000238 ) ) ;
#5786 = CARTESIAN_POINT ( 'NONE',  ( 23.55258138210000141, -57.47122622279999860, 0.3294346322440000474 ) ) ;
#5787 = CARTESIAN_POINT ( 'NONE',  ( -20.88233480739999948, -63.63883271309998690, 12.80551527529999944 ) ) ;
#5788 = ORIENTED_EDGE ( 'NONE', *, *, #12658, .T. ) ;
#5789 = AXIS2_PLACEMENT_3D ( 'NONE', #15072, #8809, #21656 ) ;
#5790 = CARTESIAN_POINT ( 'NONE',  ( 20.41153474230850051, -98.08323605630401687, -1.437002437402584043 ) ) ;
#5791 = CARTESIAN_POINT ( 'NONE',  ( 15.63748056140000209, -101.1889999979999999, 3.386620984279999913 ) ) ;
#5792 = EDGE_CURVE ( 'NONE', #1710, #17884, #25603, .T. ) ;
#5793 = CARTESIAN_POINT ( 'NONE',  ( -1.415652922210000053, -19.46458168450000059, -22.11082617310000131 ) ) ;
#5794 = CARTESIAN_POINT ( 'NONE',  ( -7.109209100094830980, -101.5526869446641456, 14.41623343727262352 ) ) ;
#5795 = ORIENTED_EDGE ( 'NONE', *, *, #10051, .F. ) ;
#5796 = ADVANCED_FACE ( 'NONE', ( #12827 ), #15168, .F. ) ;
#5797 = CARTESIAN_POINT ( 'NONE',  ( -41.72484683961315000, -65.10974319587182890, -2.782833434445878940 ) ) ;
#5798 = CARTESIAN_POINT ( 'NONE',  ( 8.987275428499998498, -35.25070440529999871, -19.47217453680000077 ) ) ;
#5799 = CARTESIAN_POINT ( 'NONE',  ( 36.36887067909999871, -79.22577739489999260, -14.85406736540000061 ) ) ;
#5800 = ORIENTED_EDGE ( 'NONE', *, *, #3428, .F. ) ;
#5801 = B_SPLINE_CURVE_WITH_KNOTS ( 'NONE', 3,
 ( #5052, #7251, #9122, #16118, #26781, #2737, #11593, #13942, #9416, #4912, #13791, #126, #18024, #13646, #22246, #15674, #4619, #20351, #20501, #4772, #18324, #572, #25019, #24579, #22555, #24877, #27213, #15826, #20208, #2296 ),
 .UNSPECIFIED., .F., .F.,
 ( 4, 1, 1, 1, 1, 2, 2, 1, 1, 1, 1, 2, 2, 2, 1, 1, 1, 1, 2, 2, 4 ),
 ( 0.000000000000000000, 0.1250000000000730249, 0.1875000000001089129, 0.2187500000001260103, 0.2343750000001336986, 0.2421875000001385003, 0.2500000000001432743, 0.3750000000001741385, 0.4375000000001877942, 0.4687500000001946221, 0.4843750000001973421, 0.4921875000001995071, 0.5000000000002016165, 0.6250000000002247091, 0.6875000000002352563, 0.7187500000002405853, 0.7343750000002452483, 0.7421875000002475797, 0.7460937500002480238, 0.7500000000002483569, 1.000000000000000000 ),
 .UNSPECIFIED. ) ;
#5802 = AXIS2_PLACEMENT_3D ( 'NONE', #22120, #22256, #28369 ) ;
#5803 = CARTESIAN_POINT ( 'NONE',  ( 6.977121519902694580, -100.1585711159146257, 15.69426428360687709 ) ) ;
#5804 = CARTESIAN_POINT ( 'NONE',  ( 11.56318970670437452, -101.1604341566338121, -10.10588458626208208 ) ) ;
#5805 = EDGE_LOOP ( 'NONE', ( #15435, #17846, #23210, #26823 ) ) ;
#5806 = CARTESIAN_POINT ( 'NONE',  ( -13.16183723299999997, -70.12921532840000793, -24.09258145020000086 ) ) ;
#5807 = CARTESIAN_POINT ( 'NONE',  ( -18.06240238254229880, -98.56362441878414415, 4.716205741958754416 ) ) ;
#5808 = ORIENTED_EDGE ( 'NONE', *, *, #4004, .T. ) ;
#5809 = AXIS2_PLACEMENT_3D ( 'NONE', #19269, #10079, #3277 ) ;
#5810 = CARTESIAN_POINT ( 'NONE',  ( 27.42310009790000080, -92.79907194240000479, 9.733922945540001592 ) ) ;
#5811 = CARTESIAN_POINT ( 'NONE',  ( 8.548167153169895727, -18.60777319252632012, -18.90116954123247339 ) ) ;
#5812 = EDGE_LOOP ( 'NONE', ( #12174, #24678, #22629, #4073, #25026 ) ) ;
#5813 = CARTESIAN_POINT ( 'NONE',  ( -42.08877555573144491, -63.33820092556624815, 0.8147708127840216363 ) ) ;
#5814 = CARTESIAN_POINT ( 'NONE',  ( 19.49544348199999888, -35.50000000000000000, -8.986258402430001624 ) ) ;
#5815 = ORIENTED_EDGE ( 'NONE', *, *, #9011, .F. ) ;
#5816 = CARTESIAN_POINT ( 'NONE',  ( 50.00000000000000000, -11.00000000000000000, 1.776356839399999922E-14 ) ) ;
#5817 = DIRECTION ( 'NONE',  ( 0.7071067811865475727, 0.000000000000000000, -0.7071067811865475727 ) ) ;
#5818 = DIRECTION ( 'NONE',  ( -0.5301416321220548955, 0.000000000000000000, -0.8479091047340887588 ) ) ;
#5819 = CARTESIAN_POINT ( 'NONE',  ( -1.558004792230000213, -18.50000000000000000, -21.15181860990000118 ) ) ;
#5820 = ORIENTED_EDGE ( 'NONE', *, *, #23270, .F. ) ;
#5821 = EDGE_CURVE ( 'NONE', #7330, #19526, #5414, .T. ) ;
#5822 = CARTESIAN_POINT ( 'NONE',  ( -15.14477094210000097, -98.93445099689999722, -10.94682493010000002 ) ) ;
#5823 = CARTESIAN_POINT ( 'NONE',  ( 15.82848316267510747, -101.5902664364219135, 2.618622591423955370 ) ) ;
#5824 = CARTESIAN_POINT ( 'NONE',  ( -20.21807458789999856, -92.87437404489999437, 18.51498583080000060 ) ) ;
#5825 = CARTESIAN_POINT ( 'NONE',  ( 24.80162329460000237, -92.90721294759998727, -13.73419815169999936 ) ) ;
#5826 = PLANE ( 'NONE',  #8154 ) ;
#5827 = CARTESIAN_POINT ( 'NONE',  ( 29.76318999973515034, -92.71619979446128923, 6.663522998223462501 ) ) ;
#5828 = CARTESIAN_POINT ( 'NONE',  ( -2.582000063019999736, -32.72519969599999712, -24.62603268980000237 ) ) ;
#5829 = VERTEX_POINT ( 'NONE', #11224 ) ;
#5830 = EDGE_CURVE ( 'NONE', #10454, #16409, #15138, .T. ) ;
#5831 = DIRECTION ( 'NONE',  ( 0.9952295494196653491, 0.000000000000000000, 0.09756097560976997873 ) ) ;
#5832 = B_SPLINE_CURVE_WITH_KNOTS ( 'NONE', 5,
 ( #23300, #7854, #16456, #5389, #3209, #756 ),
 .UNSPECIFIED., .F., .F.,
 ( 6, 6 ),
 ( 0.000000000000000000, 1.000000000000000000 ),
 .UNSPECIFIED. ) ;
#5833 = CARTESIAN_POINT ( 'NONE',  ( 29.08514934200000113, -20.00000000000000000, 53.24000875469999983 ) ) ;
#5834 = CARTESIAN_POINT ( 'NONE',  ( 21.25651707432598414, -96.89152197653719156, 0.6302383136284459564 ) ) ;
#5835 = CARTESIAN_POINT ( 'NONE',  ( 28.96803677850000369, -74.08474241140000061, -26.54391550880000139 ) ) ;
#5836 = CARTESIAN_POINT ( 'NONE',  ( -14.17623297788752801, -74.02548642939331103, 36.23315183394973360 ) ) ;
#5837 = EDGE_LOOP ( 'NONE', ( #13485, #24196, #13283, #9790 ) ) ;
#5838 = CARTESIAN_POINT ( 'NONE',  ( 6.831813925109999630, -11.50000000000000000, 12.50555150689999984 ) ) ;
#5839 = CARTESIAN_POINT ( 'NONE',  ( 20.55825494609999993, -36.03428657229999743, -8.976966250369997624 ) ) ;
#5840 = CARTESIAN_POINT ( 'NONE',  ( -22.03951503178797466, -79.50000008679997165, -32.70331798545759483 ) ) ;
#5841 = ORIENTED_EDGE ( 'NONE', *, *, #16811, .T. ) ;
#5842 = CARTESIAN_POINT ( 'NONE',  ( 10.74632799350000134, -97.93548434830000815, 16.80947664850000223 ) ) ;
#5843 = CARTESIAN_POINT ( 'NONE',  ( -15.10670588340000009, -93.09001853929999015, -23.64475874150000223 ) ) ;
#5844 = CARTESIAN_POINT ( 'NONE',  ( -8.064919287289999517, -99.61736775859999682, 15.35592295719999889 ) ) ;
#5845 = CARTESIAN_POINT ( 'NONE',  ( -2.773446675360000224, -99.97119183019999866, -17.69078287840000030 ) ) ;
#5846 = CARTESIAN_POINT ( 'NONE',  ( 21.21808891099999883, -34.59820414320000026, -7.670974023059999425 ) ) ;
#5847 = CIRCLE ( 'NONE', #10041, 53.75557630320000868 ) ;
#5848 = CARTESIAN_POINT ( 'NONE',  ( 7.361150943080000175, -101.1292390549999993, 13.64770487110000019 ) ) ;
#5849 = ORIENTED_EDGE ( 'NONE', *, *, #3428, .T. ) ;
#5850 = EDGE_CURVE ( 'NONE', #10833, #8141, #21235, .T. ) ;
#5851 = CARTESIAN_POINT ( 'NONE',  ( 13.27227242060828871, -100.9616911410478934, -9.861731524377153946 ) ) ;
#5852 = CARTESIAN_POINT ( 'NONE',  ( -25.52527845280000207, -93.36531860699999186, -5.788118625400000106 ) ) ;
#5853 = CARTESIAN_POINT ( 'NONE',  ( 27.11492820700000195, -72.00000000000000000, 10.50528228810000009 ) ) ;
#5854 = CARTESIAN_POINT ( 'NONE',  ( 38.81101221950712699, -73.50000015768026174, 7.152485405691547449 ) ) ;
#5855 = VERTEX_POINT ( 'NONE', #24657 ) ;
#5856 = CARTESIAN_POINT ( 'NONE',  ( 47.20527375670212678, -74.60741763389601999, -0.8389613764862925427 ) ) ;
#5857 = CARTESIAN_POINT ( 'NONE',  ( -14.86256651179999899, -74.31496036839999419, 36.29330022180000270 ) ) ;
#5858 = CARTESIAN_POINT ( 'NONE',  ( -2.667359241160000227, -19.40610837490000051, -23.95394751019999902 ) ) ;
#5859 = CARTESIAN_POINT ( 'NONE',  ( -18.51202076211952630, -92.49999999999998579, 24.23973938018714946 ) ) ;
#5860 = ORIENTED_EDGE ( 'NONE', *, *, #12172, .T. ) ;
#5861 = EDGE_CURVE ( 'NONE', #5636, #26524, #14685, .T. ) ;
#5862 = DIRECTION ( 'NONE',  ( 1.000000000000000000, 0.000000000000000000, 0.000000000000000000 ) ) ;
#5863 = CARTESIAN_POINT ( 'NONE',  ( 0.02056460011280000083, -101.1180794200000008, -15.51940904669999988 ) ) ;
#5864 = CARTESIAN_POINT ( 'NONE',  ( 8.904050045449999118, -63.43030842769999111, -23.33241554479999991 ) ) ;
#5865 = CARTESIAN_POINT ( 'NONE',  ( 16.03761573839999954, -101.2306315440000049, 2.381275335019999773 ) ) ;
#5866 = CARTESIAN_POINT ( 'NONE',  ( 21.09816162019999908, -57.90606206700000058, 10.50668310290000029 ) ) ;
#5867 = DIRECTION ( 'NONE',  ( 0.000000000000000000, 0.000000000000000000, 1.000000000000000000 ) ) ;
#5868 = ORIENTED_EDGE ( 'NONE', *, *, #15849, .F. ) ;
#5869 = CARTESIAN_POINT ( 'NONE',  ( 6.682224820120000075, -100.4071172650000108, 15.40394232580000100 ) ) ;
#5870 = CARTESIAN_POINT ( 'NONE',  ( 15.12572900610000026, -101.1180794200000008, 3.473442398169999557 ) ) ;
#5871 = CARTESIAN_POINT ( 'NONE',  ( -32.77174708219999388, -74.50000000000000000, -21.60034937629999874 ) ) ;
#5872 = CARTESIAN_POINT ( 'NONE',  ( 5.648478490313273426, -92.54687141712493315, -29.97239971131430636 ) ) ;
#5873 = APPLICATION_CONTEXT ( 'automotive_design' ) ;
#5874 = CARTESIAN_POINT ( 'NONE',  ( -6.520248143609999936, -97.93128678229999196, 18.90965181079999979 ) ) ;
#5875 = CYLINDRICAL_SURFACE ( 'NONE', #22712, 32.39999999999999858 ) ;
#5876 = CARTESIAN_POINT ( 'NONE',  ( 7.615531154710000195, -93.65023553240000354, -24.05380218500000211 ) ) ;
#5877 = B_SPLINE_CURVE_WITH_KNOTS ( 'NONE', 3,
 ( #24684, #11547, #9075, #6910, #27310, #4716, #2987, #524, #9371, #18273, #27166, #11849, #11399, #7351, #16369, #27459, #20760, #818, #14042, #16214, #27019, #9660, #13749, #9521, #22796, #18567, #7204, #25279, #4868, #5307, #2836, #14195, #7061, #23089 ),
 .UNSPECIFIED., .F., .F.,
 ( 4, 2, 2, 2, 1, 1, 2, 2, 2, 2, 1, 1, 2, 2, 2, 2, 2, 2, 4 ),
 ( 0.000000000000000000, 0.1250000000000807410, 0.1875000000001225964, 0.2187500000001417200, 0.2343750000001512956, 0.2421875000001560141, 0.2460937500001563749, 0.2500000000001567080, 0.3750000000001619260, 0.4375000000001644795, 0.4687500000001657008, 0.4843750000001652012, 0.4921875000001638689, 0.5000000000001625367, 0.6250000000001205702, 0.6875000000001005862, 0.7187500000000905942, 0.7500000000000804912, 1.000000000000000000 ),
 .UNSPECIFIED. ) ;
#5878 = B_SPLINE_SURFACE_WITH_KNOTS ( 'NONE', 5, 5, ( 
 ( #21073, #27900, #16832, #10243, #19528, #28413 ),
 ( #26316, #1990, #10684, #13027, #6341, #15206 ),
 ( #24119, #6792, #15655, #28765, #26459, #24557 ),
 ( #8951, #19881, #6492, #4452, #10832, #15351 ),
 ( #28628, #4596, #17862, #19456, #102, #13473 ),
 ( #13322, #28488, #17566, #19740, #26759, #22378 ) ),
 .UNSPECIFIED., .F., .F., .F.,
 ( 6, 6 ),
 ( 6, 6 ),
 ( 6.164978647489999068E-14, 3.318582256960000088 ),
 ( 0.000000000000000000, 0.5000000000000000000 ),
 .UNSPECIFIED. ) ;
#5879 = CARTESIAN_POINT ( 'NONE',  ( 21.68616571579999786, -36.53050720059999890, -9.276357967610000088 ) ) ;
#5880 = CARTESIAN_POINT ( 'NONE',  ( -6.950015043800000569, -101.6311724339999927, 14.42690866679999928 ) ) ;
#5881 = ORIENTED_EDGE ( 'NONE', *, *, #6007, .T. ) ;
#5882 =( NAMED_UNIT ( * ) SI_UNIT ( $, .STERADIAN. ) SOLID_ANGLE_UNIT ( ) );
#5883 = CARTESIAN_POINT ( 'NONE',  ( 0.000000000000000000, -20.00000000000000000, 0.000000000000000000 ) ) ;
#5884 = VERTEX_POINT ( 'NONE', #2218 ) ;
#5885 = EDGE_CURVE ( 'NONE', #27953, #10144, #17589, .T. ) ;
#5886 = ADVANCED_FACE ( 'NONE', ( #26847 ), #22623, .T. ) ;
#5887 = CARTESIAN_POINT ( 'NONE',  ( -1.271820802479999957, -100.9405348700000076, -15.89396400309999891 ) ) ;
#5888 = CARTESIAN_POINT ( 'NONE',  ( -7.309593153519999831, -74.20682108740001581, 39.90427328519999861 ) ) ;
#5889 = CARTESIAN_POINT ( 'NONE',  ( 36.74383121569999844, -74.66666669110000498, -14.69280905019999928 ) ) ;
#5890 = CARTESIAN_POINT ( 'NONE',  ( 0.000000000000000000, -65.07443093669999712, 0.000000000000000000 ) ) ;
#5891 = EDGE_CURVE ( 'NONE', #13332, #23505, #23827, .T. ) ;
#5892 = CARTESIAN_POINT ( 'NONE',  ( 20.30649716989999831, -72.92631715480000310, -31.15598209699999543 ) ) ;
#5893 = CARTESIAN_POINT ( 'NONE',  ( -22.62045161340000021, -72.18745079350000537, 17.95000703219999849 ) ) ;
#5894 = DIRECTION ( 'NONE',  ( 1.000000000000000000, 0.000000000000000000, 0.000000000000000000 ) ) ;
#5895 = CARTESIAN_POINT ( 'NONE',  ( -19.07003705186754772, -19.48618186053298729, 13.97615460328316850 ) ) ;
#5896 = CARTESIAN_POINT ( 'NONE',  ( 0.000000000000000000, -77.00000000000000000, 40.00000000000000000 ) ) ;
#5897 = CARTESIAN_POINT ( 'NONE',  ( 7.275524202149999731, -35.36119132620000016, -21.39448337560000013 ) ) ;
#5898 = CYLINDRICAL_SURFACE ( 'NONE', #21570, 1.000000000000000888 ) ;
#5899 = ORIENTED_EDGE ( 'NONE', *, *, #6622, .T. ) ;
#5900 = CARTESIAN_POINT ( 'NONE',  ( -39.66122444415238846, -63.33820092554161363, -2.216318100524186985 ) ) ;
#5901 = ORIENTED_EDGE ( 'NONE', *, *, #4208, .F. ) ;
#5902 = ADVANCED_FACE ( 'NONE', ( #27721 ), #935, .F. ) ;
#5903 = CARTESIAN_POINT ( 'NONE',  ( -0.8216735425519999803, -65.07443087359999367, -25.13632629549999820 ) ) ;
#5904 = DIRECTION ( 'NONE',  ( 1.000000000000000000, 0.000000000000000000, 0.000000000000000000 ) ) ;
#5905 = CARTESIAN_POINT ( 'NONE',  ( 9.015422770486624771, -94.52293547164840959, -22.16844695295810297 ) ) ;
#5906 = CARTESIAN_POINT ( 'NONE',  ( 40.50000000000000000, -15.00000000000000000, -4.500000000000000000 ) ) ;
#5907 = VERTEX_POINT ( 'NONE', #495 ) ;
#5908 = CARTESIAN_POINT ( 'NONE',  ( 21.52374314169999892, -36.14100892300000112, -6.944365564089999943 ) ) ;
#5909 = CYLINDRICAL_SURFACE ( 'NONE', #17635, 10.99999999999999822 ) ;
#5910 = ORIENTED_EDGE ( 'NONE', *, *, #14064, .F. ) ;
#5911 = CARTESIAN_POINT ( 'NONE',  ( 7.680736482459486147, -37.36815571398255287, -21.51429411660182112 ) ) ;
#5912 = SHAPE_REPRESENTATION ( 'Serpentine Belt Drive Pulley', ( #26433 ), #1786 ) ;
#5913 = EDGE_CURVE ( 'NONE', #18617, #22563, #16626, .T. ) ;
#5914 = CARTESIAN_POINT ( 'NONE',  ( -22.19754890820426141, -74.24418269597721576, -32.70460539598555272 ) ) ;
#5915 = AXIS2_PLACEMENT_3D ( 'NONE', #9650, #14032, #14460 ) ;
#5916 = CARTESIAN_POINT ( 'NONE',  ( 22.58213840700000219, -18.62337006899999992, 9.587758752840001009 ) ) ;
#5917 = DIRECTION ( 'NONE',  ( 0.000000000000000000, 1.000000000000000000, 0.000000000000000000 ) ) ;
#5918 = CARTESIAN_POINT ( 'NONE',  ( -20.69822367649999961, -60.21448500349999478, 14.94573686989999928 ) ) ;
#5919 = ORIENTED_EDGE ( 'NONE', *, *, #21438, .T. ) ;
#5920 = DIRECTION ( 'NONE',  ( 0.000000000000000000, 1.000000000000000000, 0.000000000000000000 ) ) ;
#5921 = CARTESIAN_POINT ( 'NONE',  ( -11.84587943579999880, -100.7776802639999971, -10.46823333549999901 ) ) ;
#5922 = CARTESIAN_POINT ( 'NONE',  ( -7.242462472455940770, -73.74610187082289769, 39.62162972294830610 ) ) ;
#5923 = CARTESIAN_POINT ( 'NONE',  ( 0.000000000000000000, -17.50000000000000000, 0.000000000000000000 ) ) ;
#5924 = VERTEX_POINT ( 'NONE', #14167 ) ;
#5925 = CARTESIAN_POINT ( 'NONE',  ( -41.50851755762869999, -65.12255024417927984, -2.880775255076511332 ) ) ;
#5926 = AXIS2_PLACEMENT_3D ( 'NONE', #18427, #27317, #13755 ) ;
#5927 = CARTESIAN_POINT ( 'NONE',  ( 36.90882362299999642, -79.77892039240001054, -14.42426562490000030 ) ) ;
#5928 = ORIENTED_EDGE ( 'NONE', *, *, #20134, .F. ) ;
#5929 = B_SPLINE_SURFACE_WITH_KNOTS ( 'NONE', 5, 5, ( 
 ( #17015, #19199, #1178, #3343, #3616, #12619 ),
 ( #18796, #25902, #10289, #27688, #7726, #21810 ),
 ( #14947, #26333, #4177, #23853, #3894, #24141 ),
 ( #13050, #13343, #127, #19760, #22110, #8823 ),
 ( #19621, #17739, #26041, #21668, #26624, #15223 ),
 ( #8675, #6663, #17587, #4328, #1718, #28505 ),
 ( #2151, #17448, #22248, #8545, #21961, #6066 ),
 ( #19472, #12757, #10558, #28361, #8392, #6359 ),
 ( #17298, #26190, #2010, #6221, #26476, #1864 ),
 ( #21057, #5598, #682, #16381, #16530, #18868 ),
 ( #5170, #1116, #23377, #22809, #827, #3419 ),
 ( #12284, #7663, #27177, #9816, #22961, #18581 ) ),
 .UNSPECIFIED., .F., .F., .F.,
 ( 6, 3, 3, 6 ),
 ( 6, 6 ),
 ( 1.571604936880000172E-14, 0.7090651247770000110, 1.217987177950000000, 1.662727347059999916 ),
 ( 0.000000000000000000, 0.5000000000000000000 ),
 .UNSPECIFIED. ) ;
#5930 = ADVANCED_FACE ( 'NONE', ( #16343 ), #7756, .T. ) ;
#5931 = CARTESIAN_POINT ( 'NONE',  ( 6.827177860526931319, -100.4010812938127231, 15.54740832690005625 ) ) ;
#5932 = CARTESIAN_POINT ( 'NONE',  ( -1.788420423618143573, -80.14911468510305781, 47.02595689713370319 ) ) ;
#5933 = EDGE_CURVE ( 'NONE', #18741, #19945, #25873, .T. ) ;
#5934 = ORIENTED_EDGE ( 'NONE', *, *, #21545, .F. ) ;
#5935 = AXIS2_PLACEMENT_3D ( 'NONE', #7733, #11935, #4815 ) ;
#5936 = CARTESIAN_POINT ( 'NONE',  ( -18.87175863199883707, -97.59429761047931606, 6.378058639867395740 ) ) ;
#5937 = EDGE_LOOP ( 'NONE', ( #28726, #20105, #21031 ) ) ;
#5938 = CARTESIAN_POINT ( 'NONE',  ( 28.52646387189999899, -92.76004106530000115, 8.498496893989999634 ) ) ;
#5939 = CARTESIAN_POINT ( 'NONE',  ( 7.215414233289999757, -74.50000000000000000, 40.70731707320000226 ) ) ;
#5940 = DIRECTION ( 'NONE',  ( 0.000000000000000000, -1.000000000000000000, 0.000000000000000000 ) ) ;
#5941 = EDGE_CURVE ( 'NONE', #9669, #11676, #6799, .T. ) ;
#5942 = EDGE_LOOP ( 'NONE', ( #6451, #8534, #17650, #11971 ) ) ;
#5943 = CARTESIAN_POINT ( 'NONE',  ( 14.05983645159999895, -99.53431386179998697, -10.27466725399999881 ) ) ;
#5944 = FACE_OUTER_BOUND ( 'NONE', #14968, .T. ) ;
#5945 = VECTOR ( 'NONE', #9955, 1000.000000000000000 ) ;
#5946 = CARTESIAN_POINT ( 'NONE',  ( -2.664535259099999805E-15, -72.00000000000000000, -3.552713678799999608E-15 ) ) ;
#5947 = CARTESIAN_POINT ( 'NONE',  ( -15.25169713729999899, -93.03108158919999937, 25.12655145109999921 ) ) ;
#5948 = ORIENTED_EDGE ( 'NONE', *, *, #7129, .T. ) ;
#5949 = FACE_OUTER_BOUND ( 'NONE', #2897, .T. ) ;
#5950 = CARTESIAN_POINT ( 'NONE',  ( 13.02419203620000054, -101.1191090859999946, -9.808337647929999292 ) ) ;
#5951 = CARTESIAN_POINT ( 'NONE',  ( 24.49010421493784406, -63.63799308313229375, -0.5178719358674350737 ) ) ;
#5952 = B_SPLINE_CURVE_WITH_KNOTS ( 'NONE', 5,
 ( #28555, #17493, #2499, #24337, #11354, #18075 ),
 .UNSPECIFIED., .F., .F.,
 ( 6, 6 ),
 ( 0.000000000000000000, 1.000000000000000000 ),
 .UNSPECIFIED. ) ;
#5953 = CARTESIAN_POINT ( 'NONE',  ( 24.74320438849999704, -92.87863185420000889, -15.37964689979999910 ) ) ;
#5954 = CARTESIAN_POINT ( 'NONE',  ( -0.8452062098810000368, -52.63280639840000674, -23.17863372589999926 ) ) ;
#5955 = CARTESIAN_POINT ( 'NONE',  ( -2.982732789429999976, -80.14658269599999585, 46.75678581369999876 ) ) ;
#5956 = CARTESIAN_POINT ( 'NONE',  ( -38.25000000000000000, -65.41419836839999391, -2.121055962329999822 ) ) ;
#5957 = VERTEX_POINT ( 'NONE', #27433 ) ;
#5958 = AXIS2_PLACEMENT_3D ( 'NONE', #4357, #6990, #4203 ) ;
#5959 = CARTESIAN_POINT ( 'NONE',  ( 0.000000000000000000, -15.49689110870000164, 0.000000000000000000 ) ) ;
#5960 = FACE_OUTER_BOUND ( 'NONE', #23476, .T. ) ;
#5961 = DIRECTION ( 'NONE',  ( 0.000000000000000000, 1.000000000000000000, 0.000000000000000000 ) ) ;
#5962 = CARTESIAN_POINT ( 'NONE',  ( 18.48933855830000184, -18.50000000000000000, 10.02928721039999971 ) ) ;
#5963 = CARTESIAN_POINT ( 'NONE',  ( -14.52092404085399480, -74.11005257168056914, 36.26393844516264409 ) ) ;
#5964 =( NAMED_UNIT ( * ) PLANE_ANGLE_UNIT ( ) SI_UNIT ( $, .RADIAN. ) );
#5965 = EDGE_CURVE ( 'NONE', #7778, #2153, #786, .T. ) ;
#5966 = EDGE_CURVE ( 'NONE', #17644, #6901, #11821, .T. ) ;
#5967 = ORIENTED_EDGE ( 'NONE', *, *, #13761, .T. ) ;
#5968 = CARTESIAN_POINT ( 'NONE',  ( -39.82679900524143335, -73.86845561502485680, -7.247933038825284058 ) ) ;
#5969 = EDGE_LOOP ( 'NONE', ( #11104, #6444, #18054, #28598 ) ) ;
#5970 = CARTESIAN_POINT ( 'NONE',  ( 20.13916512639999823, -35.75711592529999194, -8.969779973209998758 ) ) ;
#5971 = DIRECTION ( 'NONE',  ( -0.000000000000000000, 1.000000000000000000, 0.000000000000000000 ) ) ;
#5972 = EDGE_CURVE ( 'NONE', #27517, #3056, #24000, .T. ) ;
#5973 = ORIENTED_EDGE ( 'NONE', *, *, #9868, .F. ) ;
#5974 = CARTESIAN_POINT ( 'NONE',  ( -12.62850920960000067, -101.1292389529999980, -8.999250585949999603 ) ) ;
#5975 = EDGE_CURVE ( 'NONE', #15187, #3937, #9493, .T. ) ;
#5976 = AXIS2_PLACEMENT_3D ( 'NONE', #18926, #5920, #3606 ) ;
#5977 = LINE ( 'NONE', #10606, #22843 ) ;
#5978 = CARTESIAN_POINT ( 'NONE',  ( -8.306762876789999694, -99.70407914540000149, 15.05683357740000083 ) ) ;
#5979 = ORIENTED_EDGE ( 'NONE', *, *, #20948, .F. ) ;
#5980 = VECTOR ( 'NONE', #25647, 1000.000000000000000 ) ;
#5981 = CYLINDRICAL_SURFACE ( 'NONE', #21598, 57.74999999999999289 ) ;
#5982 = CARTESIAN_POINT ( 'NONE',  ( 9.030336851690002220, -49.07760086190000237, -22.46437391599999955 ) ) ;
#5983 = FACE_OUTER_BOUND ( 'NONE', #17671, .T. ) ;
#5984 = ORIENTED_EDGE ( 'NONE', *, *, #26451, .T. ) ;
#5985 = CARTESIAN_POINT ( 'NONE',  ( 13.32384360391719902, -100.8945630383305172, -9.880903774112189453 ) ) ;
#5986 = CARTESIAN_POINT ( 'NONE',  ( -23.86455928470000032, -93.85307999919999133, -7.129255525669999649 ) ) ;
#5987 = CARTESIAN_POINT ( 'NONE',  ( 39.82679900458370525, -73.86845561458682141, 7.247933038809558859 ) ) ;
#5988 = EDGE_LOOP ( 'NONE', ( #1957, #26836, #6921, #13735 ) ) ;
#5989 = CARTESIAN_POINT ( 'NONE',  ( -13.91698628299999996, -74.00000000000000000, 36.28539016370000070 ) ) ;
#5990 = CARTESIAN_POINT ( 'NONE',  ( -14.59449648670000066, -74.30694342880001102, 36.46277468150000090 ) ) ;
#5991 = CARTESIAN_POINT ( 'NONE',  ( -0.9323766011660000741, -19.46563609400000061, -22.01671729150000090 ) ) ;
#5992 = DIRECTION ( 'NONE',  ( 0.000000000000000000, 1.000000000000000000, 0.000000000000000000 ) ) ;
#5993 = ORIENTED_EDGE ( 'NONE', *, *, #18441, .T. ) ;
#5994 = DIRECTION ( 'NONE',  ( 0.8775825618903722036, 0.000000000000000000, -0.4794255386042041156 ) ) ;
#5995 = CIRCLE ( 'NONE', #7427, 0.5000000000000004441 ) ;
#5996 = CARTESIAN_POINT ( 'NONE',  ( 41.00000000000000000, -84.00000000000000000, 10.20110288159999890 ) ) ;
#5997 = CARTESIAN_POINT ( 'NONE',  ( 9.592815379950000221, -63.15675378939999973, -23.84803803759999852 ) ) ;
#5998 = CARTESIAN_POINT ( 'NONE',  ( 15.14287553800000019, -101.1516803200000112, 2.366416619579999825 ) ) ;
#5999 = CARTESIAN_POINT ( 'NONE',  ( 23.16843193700000114, -58.19955223950000089, 10.39065333399999957 ) ) ;
#6000 = CARTESIAN_POINT ( 'NONE',  ( -10.66143851719999880, -19.46147658920000012, -19.56664533329999855 ) ) ;
#6001 = VERTEX_POINT ( 'NONE', #11668 ) ;
#6002 = AXIS2_PLACEMENT_3D ( 'NONE', #14365, #26798, #6830 ) ;
#6003 = CIRCLE ( 'NONE', #14408, 3.750000000000000000 ) ;
#6004 = CARTESIAN_POINT ( 'NONE',  ( 6.850256061619999670, -100.3063911739999980, 15.61955539839999929 ) ) ;
#6005 = CARTESIAN_POINT ( 'NONE',  ( 15.54628162380000056, -101.3256027139999986, 3.366869961439999948 ) ) ;
#6006 = EDGE_CURVE ( 'NONE', #19985, #11556, #10889, .T. ) ;
#6007 = EDGE_CURVE ( 'NONE', #17600, #767, #1687, .T. ) ;
#6008 = CARTESIAN_POINT ( 'NONE',  ( -40.18318593513492232, -65.73348302056557202, -2.187882697783523955 ) ) ;
#6009 = CARTESIAN_POINT ( 'NONE',  ( 23.61771397852908905, -61.89519144020896135, 10.58390714728316517 ) ) ;
#6010 = CARTESIAN_POINT ( 'NONE',  ( -12.97028186550000051, -64.93834961630000180, 21.65804104839999766 ) ) ;
#6011 = ORIENTED_EDGE ( 'NONE', *, *, #20744, .F. ) ;
#6012 = CARTESIAN_POINT ( 'NONE',  ( 8.990098085549998785, -94.64125147560000073, -23.28616752739999995 ) ) ;
#6013 = ADVANCED_FACE ( 'NONE', ( #18690 ), #2960, .F. ) ;
#6014 = DIRECTION ( 'NONE',  ( 0.000000000000000000, 1.000000000000000000, 0.000000000000000000 ) ) ;
#6015 = CARTESIAN_POINT ( 'NONE',  ( -6.477090623329999630, -101.1848541609999899, 13.84155909140000063 ) ) ;
#6016 = ORIENTED_EDGE ( 'NONE', *, *, #8795, .T. ) ;
#6017 = DIRECTION ( 'NONE',  ( 1.000000000000000000, 0.000000000000000000, 0.000000000000000000 ) ) ;
#6018 = CARTESIAN_POINT ( 'NONE',  ( -5.298192075760000286, -100.9197081840000010, 14.69882727599999939 ) ) ;
#6019 = VERTEX_POINT ( 'NONE', #27141 ) ;
#6020 = AXIS2_PLACEMENT_3D ( 'NONE', #24705, #5328, #27039 ) ;
#6021 = CARTESIAN_POINT ( 'NONE',  ( -1.034434536250000036, -101.3350617309999961, -15.98868234950000300 ) ) ;
#6022 = CARTESIAN_POINT ( 'NONE',  ( -43.25473555329831754, -63.06504043304213525, -0.1318650859683790921 ) ) ;
#6023 = CARTESIAN_POINT ( 'NONE',  ( -17.12548553040000243, -99.53431416519998720, 3.156821174210000081 ) ) ;
#6024 = DIRECTION ( 'NONE',  ( 0.000000000000000000, -1.000000000000000000, 0.000000000000000000 ) ) ;
#6025 = CARTESIAN_POINT ( 'NONE',  ( 19.43005615430000077, -18.50000000000000000, -7.795798979470000667 ) ) ;
#6026 = DIRECTION ( 'NONE',  ( -0.8775825618903722036, 0.000000000000000000, 0.4794255386042041156 ) ) ;
#6027 = CARTESIAN_POINT ( 'NONE',  ( -15.42268960139999834, -101.6484611540000031, 4.259183661159999801 ) ) ;
#6028 = CARTESIAN_POINT ( 'NONE',  ( -19.03017963434894355, -19.48524588021119897, 13.93486461670488019 ) ) ;
#6029 = DIRECTION ( 'NONE',  ( 1.000000000000000000, 0.000000000000000000, 0.000000000000000000 ) ) ;
#6030 = ORIENTED_EDGE ( 'NONE', *, *, #10677, .F. ) ;
#6031 = CARTESIAN_POINT ( 'NONE',  ( 8.242644157730001808, -18.61945111320000024, -19.92601236959999866 ) ) ;
#6032 = VERTEX_POINT ( 'NONE', #7181 ) ;
#6033 = CARTESIAN_POINT ( 'NONE',  ( 22.45851445570000138, -37.35781404580000498, -9.270563969170000362 ) ) ;
#6034 = TOROIDAL_SURFACE ( 'NONE', #27480, 55.85192378860000417, 0.3499999999999999778 ) ;
#6035 = AXIS2_PLACEMENT_3D ( 'NONE', #23869, #21401, #22223 ) ;
#6036 = ADVANCED_FACE ( 'NONE', ( #25251 ), #11431, .T. ) ;
#6037 = CARTESIAN_POINT ( 'NONE',  ( -1.246792988649999989, -63.98660223360000288, -24.68432187749999684 ) ) ;
#6038 = CARTESIAN_POINT ( 'NONE',  ( -28.92127267589999917, -92.49999926799999628, 4.832872623250000110 ) ) ;
#6039 = EDGE_CURVE ( 'NONE', #16955, #4550, #2811, .T. ) ;
#6040 = LINE ( 'NONE', #27926, #10564 ) ;
#6041 = CARTESIAN_POINT ( 'NONE',  ( -10.20110288159999890, -82.25000000000000000, 41.00000000000000000 ) ) ;
#6042 = EDGE_CURVE ( 'NONE', #54, #24400, #20309, .T. ) ;
#6043 = DIRECTION ( 'NONE',  ( 1.000000000000000000, 0.000000000000000000, 0.000000000000000000 ) ) ;
#6044 = ORIENTED_EDGE ( 'NONE', *, *, #16592, .F. ) ;
#6045 = CARTESIAN_POINT ( 'NONE',  ( 21.43032141470000340, -35.85552704899999554, -7.415723140210000786 ) ) ;
#6046 = CARTESIAN_POINT ( 'NONE',  ( -13.24460949609980176, -57.44036993108258571, 20.55651328139954970 ) ) ;
#6047 = EDGE_LOOP ( 'NONE', ( #16082, #11663, #8791, #23195 ) ) ;
#6048 = DIRECTION ( 'NONE',  ( 0.000000000000000000, 1.000000000000000000, 0.000000000000000000 ) ) ;
#6049 = ORIENTED_EDGE ( 'NONE', *, *, #17536, .T. ) ;
#6050 = CARTESIAN_POINT ( 'NONE',  ( -14.48711453910000024, -79.93770852559998730, 37.01826959139999929 ) ) ;
#6051 = AXIS2_PLACEMENT_3D ( 'NONE', #14639, #25723, #1266 ) ;
#6052 = CARTESIAN_POINT ( 'NONE',  ( -18.17465718120000062, -18.50000000000000000, 14.49293709880000058 ) ) ;
#6053 = AXIS2_PLACEMENT_3D ( 'NONE', #621, #18941, #27824 ) ;
#6054 = TOROIDAL_SURFACE ( 'NONE', #22844, 55.85192378860000417, 0.3499999999999999778 ) ;
#6055 = CARTESIAN_POINT ( 'NONE',  ( -14.77445022520000073, -101.2530993010000060, 3.545507728200000042 ) ) ;
#6056 = CARTESIAN_POINT ( 'NONE',  ( -32.83566817743611210, -74.45672837283663625, -22.22906645946389403 ) ) ;
#6057 = CARTESIAN_POINT ( 'NONE',  ( -19.94071978170000392, -58.91580639759999372, 14.22745801819999834 ) ) ;
#6058 = EDGE_CURVE ( 'NONE', #18617, #11029, #6105, .T. ) ;
#6059 = ORIENTED_EDGE ( 'NONE', *, *, #7944, .F. ) ;
#6060 = FACE_OUTER_BOUND ( 'NONE', #4398, .T. ) ;
#6061 = CARTESIAN_POINT ( 'NONE',  ( -12.47865851810000137, -101.3852859389999992, -10.00366179029999891 ) ) ;
#6062 = CARTESIAN_POINT ( 'NONE',  ( -0.5819109535500001096, -18.85523519099999845, -21.88665078049999835 ) ) ;
#6063 = DIRECTION ( 'NONE',  ( 0.000000000000000000, 1.000000000000000000, 0.000000000000000000 ) ) ;
#6064 = EDGE_LOOP ( 'NONE', ( #3763, #680, #23058, #14391, #26968, #10930, #875, #19809, #25627 ) ) ;
#6065 = PLANE ( 'NONE',  #5627 ) ;
#6066 = CARTESIAN_POINT ( 'NONE',  ( -32.53182592119999583, -74.14930846740000447, -21.71085396679999846 ) ) ;
#6067 = CARTESIAN_POINT ( 'NONE',  ( 36.59060436630000623, -79.00000000000000000, -14.75000000000000000 ) ) ;
#6068 = EDGE_LOOP ( 'NONE', ( #28569, #17466, #8081, #2714 ) ) ;
#6069 = EDGE_CURVE ( 'NONE', #11541, #21210, #13345, .T. ) ;
#6070 = CARTESIAN_POINT ( 'NONE',  ( 36.80498107454818069, -79.53797605812111726, -14.59361009559306588 ) ) ;
#6071 = CARTESIAN_POINT ( 'NONE',  ( 6.663898719022744110, -101.1742791179282648, 14.95015922851185586 ) ) ;
#6072 = AXIS2_PLACEMENT_3D ( 'NONE', #13634, #16251, #18607 ) ;
#6073 = CARTESIAN_POINT ( 'NONE',  ( -3.562216332169999777, -80.49999996399999702, 46.31451619710000500 ) ) ;
#6074 = CIRCLE ( 'NONE', #21445, 57.75000000000000000 ) ;
#6075 = ORIENTED_EDGE ( 'NONE', *, *, #17561, .T. ) ;
#6076 = EDGE_CURVE ( 'NONE', #8673, #25599, #22394, .T. ) ;
#6077 = VECTOR ( 'NONE', #2546, 1000.000000000000000 ) ;
#6078 = FACE_OUTER_BOUND ( 'NONE', #24803, .T. ) ;
#6079 = EDGE_LOOP ( 'NONE', ( #26468, #24749, #5044, #21907 ) ) ;
#6080 = B_SPLINE_CURVE_WITH_KNOTS ( 'NONE', 5,
 ( #21575, #24037, #8296, #28263, #23760, #23903, #19804, #28684, #1631, #24335, #1762, #19662 ),
 .UNSPECIFIED., .F., .F.,
 ( 6, 3, 3, 6 ),
 ( 0.000000000000000000, 0.5344641413661697094, 0.6876411154090131816, 0.9548616571615552440 ),
 .UNSPECIFIED. ) ;
#6081 = CARTESIAN_POINT ( 'NONE',  ( 29.24515378159999912, -92.51542729400000553, 6.970541694669999622 ) ) ;
#6082 = CARTESIAN_POINT ( 'NONE',  ( -38.25000000000810729, -63.07120704560290392, 2.719973428241237112 ) ) ;
#6083 = DIRECTION ( 'NONE',  ( 0.000000000000000000, -1.000000000000000000, 0.000000000000000000 ) ) ;
#6084 = ORIENTED_EDGE ( 'NONE', *, *, #16719, .T. ) ;
#6085 = DIRECTION ( 'NONE',  ( -0.8479091047340884257, 0.000000000000000000, 0.5301416321220554506 ) ) ;
#6086 = CARTESIAN_POINT ( 'NONE',  ( -10.20110288159999890, -80.50000000000000000, 41.00000000000000000 ) ) ;
#6087 = CARTESIAN_POINT ( 'NONE',  ( -42.25000000000000000, -63.30468293320000583, 0.7216878364880000563 ) ) ;
#6088 = CARTESIAN_POINT ( 'NONE',  ( -22.03785038180000200, -92.91851489729999969, -20.07776381180000058 ) ) ;
#6089 = CARTESIAN_POINT ( 'NONE',  ( -2.934623177220000212, -18.50000000000000000, -22.07839963489999846 ) ) ;
#6090 = ORIENTED_EDGE ( 'NONE', *, *, #18097, .T. ) ;
#6091 = CARTESIAN_POINT ( 'NONE',  ( -16.93606078800000247, -97.83383802270000729, -10.57851684799999958 ) ) ;
#6092 = CARTESIAN_POINT ( 'NONE',  ( 13.68838860480000186, -100.0496341300000154, -9.933239034620001462 ) ) ;
#6093 = DIRECTION ( 'NONE',  ( 1.000000000000000000, 0.000000000000000000, 0.000000000000000000 ) ) ;
#6094 = EDGE_CURVE ( 'NONE', #5668, #3611, #18968, .T. ) ;
#6095 = CARTESIAN_POINT ( 'NONE',  ( 24.85836157880000030, -93.07693985719998864, -13.75204276130000025 ) ) ;
#6096 = ORIENTED_EDGE ( 'NONE', *, *, #21080, .T. ) ;
#6097 = AXIS2_PLACEMENT_3D ( 'NONE', #9043, #2807, #7316 ) ;
#6098 = CARTESIAN_POINT ( 'NONE',  ( 10.84021880913943292, -72.51523419968246742, -26.83307298900866655 ) ) ;
#6099 = CARTESIAN_POINT ( 'NONE',  ( -12.41807177957389641, -68.06111460909730226, -23.59935023276523225 ) ) ;
#6100 = ORIENTED_EDGE ( 'NONE', *, *, #25179, .T. ) ;
#6101 = AXIS2_PLACEMENT_3D ( 'NONE', #1314, #1593, #15232 ) ;
#6102 = CARTESIAN_POINT ( 'NONE',  ( 21.92880676370000259, -37.95796630400000282, -8.677144394200000832 ) ) ;
#6103 = CIRCLE ( 'NONE', #20071, 9.500000000000001776 ) ;
#6104 = DIRECTION ( 'NONE',  ( 1.000000000000000000, 0.000000000000000000, 0.000000000000000000 ) ) ;
#6105 = LINE ( 'NONE', #12650, #803 ) ;
#6106 = CARTESIAN_POINT ( 'NONE',  ( 40.00000000000000000, -74.50000000000000000, 2.433892081919999696E-15 ) ) ;
#6107 = ADVANCED_FACE ( 'NONE', ( #27844 ), #16168, .F. ) ;
#6108 = CARTESIAN_POINT ( 'NONE',  ( -14.43041715065195163, -70.42331188428948963, 23.51227004908529139 ) ) ;
#6109 = SHAPE_REPRESENTATION_RELATIONSHIP ( 'NONE' , 'NONE' ,  #10734, #4297 ) ;
#6110 = EDGE_LOOP ( 'NONE', ( #27556, #1357, #19911, #9408 ) ) ;
#6111 = VECTOR ( 'NONE', #1286, 1000.000000000000000 ) ;
#6112 = CARTESIAN_POINT ( 'NONE',  ( -40.38463872098324003, -74.25043946812532170, -7.240437622411593388 ) ) ;
#6113 = ORIENTED_EDGE ( 'NONE', *, *, #11570, .F. ) ;
#6114 = AXIS2_PLACEMENT_3D ( 'NONE', #19425, #6159, #21755 ) ;
#6115 = CARTESIAN_POINT ( 'NONE',  ( 20.91612140590000024, -35.95760432899999870, -8.563236930080000420 ) ) ;
#6116 = CARTESIAN_POINT ( 'NONE',  ( 0.000000000000000000, -32.30000000000000426, 0.000000000000000000 ) ) ;
#6117 = ORIENTED_EDGE ( 'NONE', *, *, #3041, .F. ) ;
#6118 = CIRCLE ( 'NONE', #104, 30.50000000000000000 ) ;
#6119 = CARTESIAN_POINT ( 'NONE',  ( 12.10964400579999811, -97.08998106820000373, 17.02756156720000291 ) ) ;
#6120 = CARTESIAN_POINT ( 'NONE',  ( -13.12430390699999982, -92.94830164210000589, -23.71756087949999880 ) ) ;
#6121 = CARTESIAN_POINT ( 'NONE',  ( -8.158623819759998952, -99.55609327400000552, 15.35276792370000010 ) ) ;
#6122 = CARTESIAN_POINT ( 'NONE',  ( -2.925413340589999578, -99.61199057899999332, -17.15801633579999930 ) ) ;
#6123 = CARTESIAN_POINT ( 'NONE',  ( 7.019998623859999398, -53.29680639659999741, -22.12830645909999916 ) ) ;
#6124 = CARTESIAN_POINT ( 'NONE',  ( -29.73766983855969315, -92.80442066020916059, 6.776535763705393123 ) ) ;
#6125 = CARTESIAN_POINT ( 'NONE',  ( -39.90716760802018115, -65.74136842489099308, 2.178498173436029361 ) ) ;
#6126 = EDGE_LOOP ( 'NONE', ( #28719, #6610, #7619, #27446 ) ) ;
#6127 = CARTESIAN_POINT ( 'NONE',  ( 0.000000000000000000, -40.00000000000000000, 0.000000000000000000 ) ) ;
#6128 = CARTESIAN_POINT ( 'NONE',  ( 23.55258117300000009, -57.47122623430000488, 0.3294352490589999571 ) ) ;
#6129 = CARTESIAN_POINT ( 'NONE',  ( 24.48314189319999912, -69.76823842119999597, 12.05682714019999935 ) ) ;
#6130 = PLANE ( 'NONE',  #24719 ) ;
#6131 = ORIENTED_EDGE ( 'NONE', *, *, #25001, .T. ) ;
#6132 = CARTESIAN_POINT ( 'NONE',  ( -40.00100507770000036, -74.03378462380000258, 7.261004788019999268 ) ) ;
#6133 = EDGE_CURVE ( 'NONE', #16270, #2022, #9168, .T. ) ;
#6134 = CARTESIAN_POINT ( 'NONE',  ( -38.25000000000000000, -63.07912966450000880, -2.684678751729999480 ) ) ;
#6135 = CARTESIAN_POINT ( 'NONE',  ( -17.74112986619999788, -94.52292883270000345, 16.06143330240000111 ) ) ;
#6136 = CARTESIAN_POINT ( 'NONE',  ( 27.23269985219999967, -92.50000000000000000, -12.38957130830000075 ) ) ;
#6137 = EDGE_LOOP ( 'NONE', ( #11922, #693, #25964, #11121 ) ) ;
#6138 = EDGE_CURVE ( 'NONE', #23662, #13129, #25547, .T. ) ;
#6139 = CARTESIAN_POINT ( 'NONE',  ( 28.91458732679999954, -72.00000191859999177, 3.086547544710000146 ) ) ;
#6140 = DIRECTION ( 'NONE',  ( -0.9952295494196655712, 0.000000000000000000, 0.09756097560976655092 ) ) ;
#6141 = CARTESIAN_POINT ( 'NONE',  ( 9.320354432040000248, -58.88647179320000191, -23.00258203210000119 ) ) ;
#6142 = CARTESIAN_POINT ( 'NONE',  ( -12.09194248459999876, -69.13468671140000765, -24.96157070200000305 ) ) ;
#6143 = ADVANCED_FACE ( 'NONE', ( #28252 ), #14307, .T. ) ;
#6144 = DIRECTION ( 'NONE',  ( 0.1708373792999891283, 0.000000000000000000, 0.9852992387259373874 ) ) ;
#6145 = CARTESIAN_POINT ( 'NONE',  ( -37.75000000000000000, -65.63577453799999262, 0.7216878364859999895 ) ) ;
#6146 = TOROIDAL_SURFACE ( 'NONE', #22454, 15.50000000000000000, 0.5000000000000000000 ) ;
#6147 = EDGE_LOOP ( 'NONE', ( #19033, #10645, #25910, #19569 ) ) ;
#6148 = EDGE_CURVE ( 'NONE', #22871, #25977, #168, .T. ) ;
#6149 = CARTESIAN_POINT ( 'NONE',  ( 6.634569963610000620, -99.72202992580000114, 15.83960876509999949 ) ) ;
#6150 = CARTESIAN_POINT ( 'NONE',  ( 14.82033914870000046, -101.2010924020000004, 3.644636806539999885 ) ) ;
#6151 = CARTESIAN_POINT ( 'NONE',  ( -3.451442281954444802, -95.36087493701890594, 22.97937161173546272 ) ) ;
#6152 = CARTESIAN_POINT ( 'NONE',  ( -15.39089091200000148, -74.00000000000000000, 40.15260594389999937 ) ) ;
#6153 = CARTESIAN_POINT ( 'NONE',  ( 5.719937426361796362, -92.53708507728568122, -29.95886813200712595 ) ) ;
#6154 = CARTESIAN_POINT ( 'NONE',  ( -37.60355029590000697, -74.50000000000000000, 9.356041104380000917 ) ) ;
#6155 = EDGE_LOOP ( 'NONE', ( #4378, #10226, #2498, #28763 ) ) ;
#6156 = CARTESIAN_POINT ( 'NONE',  ( 1.896867888589999884, -92.62399497440000573, -29.61563552290000345 ) ) ;
#6157 = CARTESIAN_POINT ( 'NONE',  ( 19.24185463459999923, -28.60070551269999939, -8.999622039089999248 ) ) ;
#6158 = DIRECTION ( 'NONE',  ( 0.000000000000000000, 1.000000000000000000, 0.000000000000000000 ) ) ;
#6159 = DIRECTION ( 'NONE',  ( 1.665334536939999828E-16, 0.000000000000000000, 1.000000000000000000 ) ) ;
#6160 = ORIENTED_EDGE ( 'NONE', *, *, #7631, .T. ) ;
#6161 = DIRECTION ( 'NONE',  ( 0.000000000000000000, 1.000000000000000000, 0.000000000000000000 ) ) ;
#6162 = CIRCLE ( 'NONE', #24328, 5.000000000000000888 ) ;
#6163 = CARTESIAN_POINT ( 'NONE',  ( 0.000000000000000000, -89.00000000000000000, 0.000000000000000000 ) ) ;
#6164 = ORIENTED_EDGE ( 'NONE', *, *, #287, .T. ) ;
#6165 = CIRCLE ( 'NONE', #26183, 0.5000000000000004441 ) ;
#6166 = CARTESIAN_POINT ( 'NONE',  ( 0.7331063123750001242, -99.53431386179998697, -17.39857302659999760 ) ) ;
#6167 = VERTEX_POINT ( 'NONE', #3519 ) ;
#6168 = CARTESIAN_POINT ( 'NONE',  ( 10.30088935743342127, -93.33134965530122429, -24.92783432923098630 ) ) ;
#6169 = CARTESIAN_POINT ( 'NONE',  ( 21.64387302759999798, -18.61794787939999907, -0.4555542569220000226 ) ) ;
#6170 = CARTESIAN_POINT ( 'NONE',  ( 0.000000000000000000, -33.79999999999999716, 0.000000000000000000 ) ) ;
#6171 = CARTESIAN_POINT ( 'NONE',  ( 12.94734957360000038, -94.70873790539999959, -19.84316983170000270 ) ) ;
#6172 = CARTESIAN_POINT ( 'NONE',  ( 15.18880477729999967, -100.8685038539999965, 4.097255861100000729 ) ) ;
#6173 = CARTESIAN_POINT ( 'NONE',  ( 19.11795961949999878, -18.50000000000000000, -7.980821806519998951 ) ) ;
#6174 = EDGE_CURVE ( 'NONE', #5109, #9851, #1299, .T. ) ;
#6175 = CARTESIAN_POINT ( 'NONE',  ( -23.04876999539999716, -71.79380085219999330, 16.27051555959999973 ) ) ;
#6176 = PRODUCT_DEFINITION_SHAPE ( 'NONE', 'NONE',  #11298 ) ;
#6177 = AXIS2_PLACEMENT_3D ( 'NONE', #11377, #7323, #9634 ) ;
#6178 = CARTESIAN_POINT ( 'NONE',  ( 9.476129726560001743, -36.00000000000000000, -20.06309461059999677 ) ) ;
#6179 = CARTESIAN_POINT ( 'NONE',  ( -11.32307664120000013, -93.00000000000000000, 9.421136869679999748 ) ) ;
#6180 = DIRECTION ( 'NONE',  ( -0.4740167705367956952, 0.000000000000000000, -0.8805158154456209640 ) ) ;
#6181 = CARTESIAN_POINT ( 'NONE',  ( 7.415722487370000060, -35.85552663179999655, -21.43032142309999699 ) ) ;
#6182 = CARTESIAN_POINT ( 'NONE',  ( 0.000000000000000000, -35.29999999999999716, 0.000000000000000000 ) ) ;
#6183 = EDGE_LOOP ( 'NONE', ( #9626, #9764, #17749, #6573 ) ) ;
#6184 = EDGE_CURVE ( 'NONE', #24319, #3448, #10099, .T. ) ;
#6185 = CARTESIAN_POINT ( 'NONE',  ( 8.147944900010001490, -19.16110315519999929, -20.46648291129999819 ) ) ;
#6186 = VECTOR ( 'NONE', #23423, 1000.000000000000114 ) ;
#6187 = VERTEX_POINT ( 'NONE', #21283 ) ;
#6188 = CARTESIAN_POINT ( 'NONE',  ( 21.41593371060000095, -36.06062539690000790, -10.16216188949999832 ) ) ;
#6189 = CIRCLE ( 'NONE', #27160, 3.000000000000002665 ) ;
#6190 = ORIENTED_EDGE ( 'NONE', *, *, #23181, .T. ) ;
#6191 = FACE_OUTER_BOUND ( 'NONE', #1096, .T. ) ;
#6192 = CARTESIAN_POINT ( 'NONE',  ( 0.000000000000000000, -2.000000000000000000, 0.000000000000000000 ) ) ;
#6193 = CARTESIAN_POINT ( 'NONE',  ( -19.55068289229999934, -53.82492386869999734, 13.58563889210000042 ) ) ;
#6194 = DIRECTION ( 'NONE',  ( 0.000000000000000000, 1.000000000000000000, 0.000000000000000000 ) ) ;
#6195 = EDGE_LOOP ( 'NONE', ( #14617, #18627, #10127, #15577 ) ) ;
#6196 = AXIS2_PLACEMENT_3D ( 'NONE', #1235, #27743, #23507 ) ;
#6197 = B_SPLINE_CURVE_WITH_KNOTS ( 'NONE', 3,
 ( #3182, #14661, #5496, #23280, #27668, #9995 ),
 .UNSPECIFIED., .F., .F.,
 ( 4, 2, 4 ),
 ( 0.000000000000000000, 0.5000000000000000000, 1.000000000000000000 ),
 .UNSPECIFIED. ) ;
#6198 = DIRECTION ( 'NONE',  ( 0.3687499999999814260, 0.000000000000000000, -0.9295286103719527793 ) ) ;
#6199 = DIRECTION ( 'NONE',  ( 0.000000000000000000, -1.000000000000000000, 0.000000000000000000 ) ) ;
#6200 = ORIENTED_EDGE ( 'NONE', *, *, #7382, .T. ) ;
#6201 = CARTESIAN_POINT ( 'NONE',  ( -37.75000000000000000, -63.00000000000000000, 0.7216878364859999895 ) ) ;
#6202 = ORIENTED_EDGE ( 'NONE', *, *, #7160, .T. ) ;
#6203 = CARTESIAN_POINT ( 'NONE',  ( -50.00000000000000000, -13.00000000000000000, -4.500000000000000000 ) ) ;
#6204 = EDGE_CURVE ( 'NONE', #7778, #23820, #24530, .T. ) ;
#6205 = CIRCLE ( 'NONE', #4344, 2.000000000000000000 ) ;
#6206 = CARTESIAN_POINT ( 'NONE',  ( 40.35498444582718491, -74.39270540192882208, 7.250043397140349732 ) ) ;
#6207 = EDGE_CURVE ( 'NONE', #26488, #16504, #4690, .T. ) ;
#6208 = CARTESIAN_POINT ( 'NONE',  ( -15.55828293380000105, -101.6484611540000031, 3.733608462300000319 ) ) ;
#6209 = CARTESIAN_POINT ( 'NONE',  ( -14.95416558133042173, -99.82487968003415801, -8.244819971624391286 ) ) ;
#6210 = CARTESIAN_POINT ( 'NONE',  ( -39.66125204418437278, -63.33820666349190986, 2.216302165637858312 ) ) ;
#6211 = ORIENTED_EDGE ( 'NONE', *, *, #5972, .F. ) ;
#6212 = DIRECTION ( 'NONE',  ( 0.000000000000000000, 0.000000000000000000, -1.000000000000000000 ) ) ;
#6213 = CARTESIAN_POINT ( 'NONE',  ( -12.01041538379999984, -101.0151300849999814, -10.01510942600000043 ) ) ;
#6214 = EDGE_CURVE ( 'NONE', #17152, #23549, #23128, .T. ) ;
#6215 = PLANE ( 'NONE',  #213 ) ;
#6216 = CARTESIAN_POINT ( 'NONE',  ( -7.191796251969473808, -101.5026031440308287, 14.41852686845345133 ) ) ;
#6217 = ORIENTED_EDGE ( 'NONE', *, *, #6361, .T. ) ;
#6218 = ADVANCED_FACE ( 'NONE', ( #4652 ), #26403, .F. ) ;
#6219 = AXIS2_PLACEMENT_3D ( 'NONE', #20247, #15862, #13529 ) ;
#6220 = DIRECTION ( 'NONE',  ( 1.000000000000000000, 0.000000000000000000, 0.000000000000000000 ) ) ;
#6221 = CARTESIAN_POINT ( 'NONE',  ( -32.63918253220000310, -74.37556698459998472, -21.86237412950000092 ) ) ;
#6222 = CARTESIAN_POINT ( 'NONE',  ( -22.32000499276877648, -79.78861691627724895, -32.79741325785565209 ) ) ;
#6223 = ORIENTED_EDGE ( 'NONE', *, *, #11601, .T. ) ;
#6224 = CARTESIAN_POINT ( 'NONE',  ( 6.678222761480453684, -101.2637735885552104, 14.86716957882814683 ) ) ;
#6225 = CARTESIAN_POINT ( 'NONE',  ( -22.43272078519999724, -80.50000000000000000, -32.20769377289999369 ) ) ;
#6226 = ORIENTED_EDGE ( 'NONE', *, *, #21230, .T. ) ;
#6227 = CARTESIAN_POINT ( 'NONE',  ( -19.26257329162280385, -97.05447415508082543, 7.349808109310738580 ) ) ;
#6228 = ORIENTED_EDGE ( 'NONE', *, *, #20978, .T. ) ;
#6229 = CARTESIAN_POINT ( 'NONE',  ( 22.22712039270000162, -56.22908209860000284, 10.11290092780000194 ) ) ;
#6230 = CARTESIAN_POINT ( 'NONE',  ( -7.215414233289999757, -82.25000000000000000, -40.70731707320000226 ) ) ;
#6231 = CYLINDRICAL_SURFACE ( 'NONE', #23730, 0.7499999999999997780 ) ;
#6232 = ORIENTED_EDGE ( 'NONE', *, *, #11565, .T. ) ;
#6233 = CARTESIAN_POINT ( 'NONE',  ( -42.08349140526518539, -65.70258710782505318, 0.8420150274644456756 ) ) ;
#6234 = DIRECTION ( 'NONE',  ( 1.000000000000000000, 0.000000000000000000, 0.000000000000000000 ) ) ;
#6235 = B_SPLINE_CURVE_WITH_KNOTS ( 'NONE', 5,
 ( #8289, #16628, #14717, #12104, #8025, #1484 ),
 .UNSPECIFIED., .F., .F.,
 ( 6, 6 ),
 ( 0.000000000000000000, 1.000000000000000000 ),
 .UNSPECIFIED. ) ;
#6236 = VECTOR ( 'NONE', #2431, 1000.000000000000114 ) ;
#6237 = CARTESIAN_POINT ( 'NONE',  ( 8.838003463759999789, -36.72346566359999542, -21.71672433710000050 ) ) ;
#6238 = CARTESIAN_POINT ( 'NONE',  ( -20.48397077079999917, -92.79907188619999658, -20.66839783129999830 ) ) ;
#6239 = CARTESIAN_POINT ( 'NONE',  ( 25.58518446212841368, -68.16673579364382363, 10.86874726639485900 ) ) ;
#6240 = ORIENTED_EDGE ( 'NONE', *, *, #12300, .T. ) ;
#6241 = EDGE_CURVE ( 'NONE', #17271, #11391, #28236, .T. ) ;
#6242 = CARTESIAN_POINT ( 'NONE',  ( -13.32814101110000138, -99.92967428129999519, -11.12411402770000102 ) ) ;
#6243 = EDGE_CURVE ( 'NONE', #25155, #19419, #21291, .T. ) ;
#6244 = CARTESIAN_POINT ( 'NONE',  ( 13.67037274660000001, -100.1981337080000003, -10.07712178240000078 ) ) ;
#6245 = DIRECTION ( 'NONE',  ( 1.000000000000000000, 0.000000000000000000, 0.000000000000000000 ) ) ;
#6246 = CARTESIAN_POINT ( 'NONE',  ( -4.362772401299999991, -17.50000000000000000, -7.986001313199998286 ) ) ;
#6247 = CARTESIAN_POINT ( 'NONE',  ( 29.76435817172988152, -92.71346081468161060, 6.658302562895561216 ) ) ;
#6248 = CARTESIAN_POINT ( 'NONE',  ( -38.25000000000000000, -65.49083508809999898, -1.947031612740000028 ) ) ;
#6249 = ORIENTED_EDGE ( 'NONE', *, *, #27637, .F. ) ;
#6250 = DIRECTION ( 'NONE',  ( 0.4794255386042041156, 0.000000000000000000, 0.8775825618903722036 ) ) ;
#6251 = DIRECTION ( 'NONE',  ( 0.4794255386042036715, 0.000000000000000000, 0.8775825618903724257 ) ) ;
#6252 = DIRECTION ( 'NONE',  ( 0.000000000000000000, 1.000000000000000000, 0.000000000000000000 ) ) ;
#6253 = DIRECTION ( 'NONE',  ( -0.004337301922959033856, 0.000000000000000000, -0.9999905938617769108 ) ) ;
#6254 = CARTESIAN_POINT ( 'NONE',  ( -0.5088921683643864435, -92.58347372262090857, -30.49575523020497769 ) ) ;
#6255 = APPLICATION_PROTOCOL_DEFINITION ( 'draft international standard', 'automotive_design', 1998, #18916 ) ;
#6256 = DIRECTION ( 'NONE',  ( 0.000000000000000000, -1.000000000000000000, 0.000000000000000000 ) ) ;
#6257 = ORIENTED_EDGE ( 'NONE', *, *, #27562, .T. ) ;
#6258 = B_SPLINE_CURVE_WITH_KNOTS ( 'NONE', 3,
 ( #23962, #15485, #6773, #1972, #3995, #21774, #12856, #10668, #10816, #8643, #17548, #26439, #19393, #24049, #23632, #12814, #28565, #21871, #1774, #6417, #28420, #21586, #23501, #26100, #12957, #10764, #19533, #25829, #5985, #12532, #10480, #28275, #17503, #21307, #5851, #15000, #19120, #19258, #8308, #8600, #8454, #17357, #14733, #28010, #21724, #3671, #26388, #1505, #3540, #14864, #12395, #23914, #10617, #16937, #1358, #3951, #1644, #12675, #17209, #10207 ),
 .UNSPECIFIED., .F., .F.,
 ( 4, 2, 1, 1, 2, 2, 2, 2, 1, 1, 2, 2, 2, 2, 2, 2, 2, 1, 1, 2, 2, 2, 2, 1, 2, 2, 2, 1, 2, 2, 2, 2, 2, 4 ),
 ( 0.000000000000000000, 0.06249999999994744482, 0.09374999999992050803, 0.1093749999999064221, 0.1171874999998935712, 0.1249999999998807343, 0.1874999999997902789, 0.2187499999997453703, 0.2343749999997233602, 0.2421874999997184474, 0.2460937499997155331, 0.2499999999997126465, 0.3124999999998161471, 0.3437499999998687716, 0.3749999999999213407, 0.4375000000000253131, 0.4687500000000772715, 0.4843750000001035283, 0.4921875000001249001, 0.4960937500001271760, 0.5000000000001294520, 0.5625000000001711964, 0.5937500000001925127, 0.6093750000002039480, 0.6171875000002032818, 0.6250000000002027267, 0.6875000000001446621, 0.7187500000001210143, 0.7343750000001157963, 0.7500000000001104672, 0.8125000000000816014, 0.8437500000000671685, 0.8750000000000528466, 1.000000000000000000 ),
 .UNSPECIFIED. ) ;
#6259 = ADVANCED_FACE ( 'NONE', ( #4062 ), #12930, .F. ) ;
#6260 = FACE_OUTER_BOUND ( 'NONE', #28547, .T. ) ;
#6261 = CARTESIAN_POINT ( 'NONE',  ( 24.53235143598864809, -18.49999964046002532, 2.185477904151989392 ) ) ;
#6262 = EDGE_LOOP ( 'NONE', ( #18955, #25239, #15732, #4925 ) ) ;
#6263 = CARTESIAN_POINT ( 'NONE',  ( 20.15567332630000053, -35.83134904089999395, -9.008831785180001717 ) ) ;
#6264 = LINE ( 'NONE', #4376, #21405 ) ;
#6265 = ORIENTED_EDGE ( 'NONE', *, *, #896, .F. ) ;
#6266 = CARTESIAN_POINT ( 'NONE',  ( 11.93184982500000046, -96.79176330629999825, 17.27990385200000034 ) ) ;
#6267 = CARTESIAN_POINT ( 'NONE',  ( -2.955163290202864612, -65.70113804361405130, -26.82187320845386935 ) ) ;
#6268 = TOROIDAL_SURFACE ( 'NONE', #10429, 3.500000000000000000, 0.5000000000000000000 ) ;
#6269 = LINE ( 'NONE', #23495, #2548 ) ;
#6270 = CARTESIAN_POINT ( 'NONE',  ( -13.16183723299999997, -70.12921532840000793, -24.09258145020000086 ) ) ;
#6271 = CARTESIAN_POINT ( 'NONE',  ( 9.272014655150000451, -53.24879282989999751, -22.83553957720000227 ) ) ;
#6272 = CARTESIAN_POINT ( 'NONE',  ( -29.62499822415610851, -92.59055325464531450, 7.253245202836821726 ) ) ;
#6273 = CARTESIAN_POINT ( 'NONE',  ( 27.35691629450000306, -72.00000000000000000, -11.81987123310000065 ) ) ;
#6274 = ORIENTED_EDGE ( 'NONE', *, *, #25423, .T. ) ;
#6275 = CARTESIAN_POINT ( 'NONE',  ( 0.000000000000000000, -84.00000000000000000, 40.00000000000000000 ) ) ;
#6276 = CARTESIAN_POINT ( 'NONE',  ( 23.36166334209999818, -57.47815921199999423, -0.2645295228999999804 ) ) ;
#6277 = CARTESIAN_POINT ( 'NONE',  ( 23.24950849600000069, -64.69849383090000572, 10.72429619139999879 ) ) ;
#6278 = CARTESIAN_POINT ( 'NONE',  ( -16.65233384409999928, -100.4382163219999882, 3.162646594119999932 ) ) ;
#6279 = ORIENTED_EDGE ( 'NONE', *, *, #26164, .F. ) ;
#6280 = CARTESIAN_POINT ( 'NONE',  ( 0.000000000000000000, -11.00000000000000000, 0.000000000000000000 ) ) ;
#6281 = CARTESIAN_POINT ( 'NONE',  ( -1.348884344130889978, -65.00127109658718894, -25.13406902656907960 ) ) ;
#6282 = CARTESIAN_POINT ( 'NONE',  ( -17.71931456970000340, -93.56364925920000530, 19.41824640629999621 ) ) ;
#6283 = DIRECTION ( 'NONE',  ( -0.6321469351840500739, 0.000000000000000000, -0.7748485350940611527 ) ) ;
#6284 = EDGE_LOOP ( 'NONE', ( #10363, #5054, #20349, #5143 ) ) ;
#6285 = DIRECTION ( 'NONE',  ( 1.000000000000000000, 0.000000000000000000, 0.000000000000000000 ) ) ;
#6286 = CARTESIAN_POINT ( 'NONE',  ( 0.6147020776099999528, -100.8685038539999965, -15.71971493089999861 ) ) ;
#6287 = CARTESIAN_POINT ( 'NONE',  ( 9.808844109879998996, -64.48635843210000473, -24.34110466499999959 ) ) ;
#6288 = CARTESIAN_POINT ( 'NONE',  ( 15.76529576789999965, -101.3957169669999985, 2.649641455589999861 ) ) ;
#6289 = CARTESIAN_POINT ( 'NONE',  ( 22.91820467009999618, -58.62494694620000502, 10.26923006039999997 ) ) ;
#6290 = CARTESIAN_POINT ( 'NONE',  ( -11.09892319740000133, -42.21394486799999868, -22.03407446800000002 ) ) ;
#6291 = ORIENTED_EDGE ( 'NONE', *, *, #8795, .F. ) ;
#6292 = CARTESIAN_POINT ( 'NONE',  ( 6.278326372410000467, -101.0403179300000005, 14.13892092110000043 ) ) ;
#6293 = CARTESIAN_POINT ( 'NONE',  ( 15.15499494600000041, -101.1292389600000092, 3.282128709870000272 ) ) ;
#6294 = B_SPLINE_CURVE_WITH_KNOTS ( 'NONE', 5,
 ( #7971, #7708, #26027, #16861, #5641, #23559 ),
 .UNSPECIFIED., .F., .F.,
 ( 6, 6 ),
 ( 0.000000000000000000, 1.000000000000000000 ),
 .UNSPECIFIED. ) ;
#6295 = ORIENTED_EDGE ( 'NONE', *, *, #4977, .F. ) ;
#6296 = EDGE_CURVE ( 'NONE', #23549, #4293, #28708, .T. ) ;
#6297 = CARTESIAN_POINT ( 'NONE',  ( -39.84007938994317044, -65.73345158628970353, -2.188026723677208629 ) ) ;
#6298 = CARTESIAN_POINT ( 'NONE',  ( 21.03406691489999858, -18.50000000000000000, -0.2329208952929999743 ) ) ;
#6299 = CARTESIAN_POINT ( 'NONE',  ( -5.860729663480000795, -96.53848370209999530, 20.54377699719999839 ) ) ;
#6300 = VERTEX_POINT ( 'NONE', #24177 ) ;
#6301 = CARTESIAN_POINT ( 'NONE',  ( 4.670288045889999573, -92.76550115769998683, -27.85728039249999810 ) ) ;
#6302 = ADVANCED_FACE ( 'NONE', ( #4210 ), #20096, .F. ) ;
#6303 = CARTESIAN_POINT ( 'NONE',  ( 20.19953095279999999, -19.44973810689999993, -8.528659567000000052 ) ) ;
#6304 = DIRECTION ( 'NONE',  ( 1.000000000000000000, 0.000000000000000000, 0.000000000000000000 ) ) ;
#6305 = DIRECTION ( 'NONE',  ( 0.000000000000000000, 1.000000000000000000, 0.000000000000000000 ) ) ;
#6306 = ORIENTED_EDGE ( 'NONE', *, *, #17528, .T. ) ;
#6307 = CARTESIAN_POINT ( 'NONE',  ( -11.74920108874028202, -34.67040743928694013, -19.26451607462440663 ) ) ;
#6308 = DIRECTION ( 'NONE',  ( 0.4794255386042059475, 0.000000000000000000, 0.8775825618903710934 ) ) ;
#6309 = ORIENTED_EDGE ( 'NONE', *, *, #26379, .T. ) ;
#6310 = CARTESIAN_POINT ( 'NONE',  ( 8.988129812000000385, -35.79614491170000434, -20.14651233290000221 ) ) ;
#6311 = EDGE_CURVE ( 'NONE', #584, #8975, #11930, .T. ) ;
#6312 = CARTESIAN_POINT ( 'NONE',  ( 23.58655530659999755, -94.70873790539999959, -2.249368515490000053 ) ) ;
#6313 = EDGE_CURVE ( 'NONE', #25599, #1700, #4319, .T. ) ;
#6314 = EDGE_LOOP ( 'NONE', ( #4513, #3087, #24947, #11967 ) ) ;
#6315 = CARTESIAN_POINT ( 'NONE',  ( -1.228311966399999955, -101.1461874320000049, -16.11255545180000226 ) ) ;
#6316 = CARTESIAN_POINT ( 'NONE',  ( 22.71729720029999910, -18.50000000000000000, 2.301109238659999612 ) ) ;
#6317 = CARTESIAN_POINT ( 'NONE',  ( 19.97576656849999921, -36.00000000000000000, -19.97576656849999921 ) ) ;
#6318 = CARTESIAN_POINT ( 'NONE',  ( -20.37063303559435212, -92.65976904082468479, -22.69994848242665242 ) ) ;
#6319 = EDGE_LOOP ( 'NONE', ( #839, #8749, #13182, #14553, #17759, #858 ) ) ;
#6320 = CARTESIAN_POINT ( 'NONE',  ( -43.10000000000000142, -65.00000000000000000, -4.511807594199999947E-13 ) ) ;
#6321 = CARTESIAN_POINT ( 'NONE',  ( -6.851093861369999871, -101.2010924020000004, 13.63775431790000070 ) ) ;
#6322 = CARTESIAN_POINT ( 'NONE',  ( 6.717799458580000049, -84.00000000000000000, 40.65853658540000026 ) ) ;
#6323 = B_SPLINE_CURVE_WITH_KNOTS ( 'NONE', 5,
 ( #15457, #12983, #6441, #24665, #20140, #24814, #11381, #10787, #10931, #21893, #15307, #17815, #350, #24224, #27004 ),
 .UNSPECIFIED., .F., .F.,
 ( 6, 3, 3, 3, 6 ),
 ( -72.86859331460000533, -71.60123715040001002, -63.48927009810000044, -56.91038232380000039, -54.97253517989999949 ),
 .UNSPECIFIED. ) ;
#6324 = DIRECTION ( 'NONE',  ( 1.000000000000000000, 0.000000000000000000, 0.000000000000000000 ) ) ;
#6325 = CARTESIAN_POINT ( 'NONE',  ( -18.91794663875353422, -19.48260761092758386, 13.81468008931694591 ) ) ;
#6326 = CARTESIAN_POINT ( 'NONE',  ( 24.62113160253329269, -93.59825775071381315, -11.14135564786052335 ) ) ;
#6327 = CIRCLE ( 'NONE', #3998, 7.250000000000000000 ) ;
#6328 = CARTESIAN_POINT ( 'NONE',  ( -11.11735237159999912, -18.50000000000000000, 18.07942598360000019 ) ) ;
#6329 = ORIENTED_EDGE ( 'NONE', *, *, #24003, .F. ) ;
#6330 = CARTESIAN_POINT ( 'NONE',  ( -38.71640881029999548, -73.50000064450000536, -7.135467304789999687 ) ) ;
#6331 = CARTESIAN_POINT ( 'NONE',  ( 0.000000000000000000, -30.20000000000000284, 0.000000000000000000 ) ) ;
#6332 = CARTESIAN_POINT ( 'NONE',  ( -2.379621828269999906, -63.61851004920001174, -25.36216796620000125 ) ) ;
#6333 = CARTESIAN_POINT ( 'NONE',  ( 9.858088328779999188, -36.06031159439999811, -21.09473900560000104 ) ) ;
#6334 = CARTESIAN_POINT ( 'NONE',  ( -25.28414760490000290, -93.59856727289999867, -2.205049167689999923 ) ) ;
#6335 = CARTESIAN_POINT ( 'NONE',  ( -19.75976373869999847, -56.26681992150000156, 12.38608856119999935 ) ) ;
#6336 = CARTESIAN_POINT ( 'NONE',  ( -16.49390888960000368, -74.00000000000000000, 44.28897684009999836 ) ) ;
#6337 = EDGE_CURVE ( 'NONE', #24581, #11515, #25717, .T. ) ;
#6338 = CARTESIAN_POINT ( 'NONE',  ( -12.07243358760000085, -67.46050599719998786, -24.77970463289999969 ) ) ;
#6339 = ORIENTED_EDGE ( 'NONE', *, *, #6042, .T. ) ;
#6340 = FACE_OUTER_BOUND ( 'NONE', #23932, .T. ) ;
#6341 = CARTESIAN_POINT ( 'NONE',  ( 7.255206491240000055, -74.34472676620001153, -40.30310653799999443 ) ) ;
#6342 = VERTEX_POINT ( 'NONE', #19200 ) ;
#6343 = EDGE_CURVE ( 'NONE', #26105, #27046, #16873, .T. ) ;
#6344 = FACE_OUTER_BOUND ( 'NONE', #17753, .T. ) ;
#6345 = EDGE_CURVE ( 'NONE', #5383, #25644, #18587, .T. ) ;
#6346 = CARTESIAN_POINT ( 'NONE',  ( -10.54884365010000025, -18.50000000000000000, -18.22394246889999891 ) ) ;
#6347 = FACE_OUTER_BOUND ( 'NONE', #7109, .T. ) ;
#6348 = CARTESIAN_POINT ( 'NONE',  ( 20.83731409940000034, -18.50000000000000000, 8.681372653689999552 ) ) ;
#6349 = CARTESIAN_POINT ( 'NONE',  ( -32.83566817450000030, -79.50000000000000000, -22.22906645670000003 ) ) ;
#6350 = CARTESIAN_POINT ( 'NONE',  ( -13.31136913029999924, -101.0685849509999912, -9.042834681369999572 ) ) ;
#6351 = B_SPLINE_SURFACE_WITH_KNOTS ( 'NONE', 5, 5, ( 
 ( #9365, #13887, #20296, #22789, #2829, #11690, #20601, #661, #16208 ),
 ( #25120, #14036, #16362, #3398, #14187, #25272, #25408, #9653, #25540 ),
 ( #7644, #27861, #27453, #8045, #7909, #16792, #25827, #7773, #16511 ),
 ( #27604, #25686, #7499, #5301, #11980, #12265, #5578, #14595, #22941 ),
 ( #5437, #2982, #23083, #5711, #21174, #5848, #14322, #23498, #14462 ),
 ( #3126, #27737, #10204, #20894, #3266, #12120, #1095, #10067, #3537 ) ),
 .UNSPECIFIED., .F., .F., .F.,
 ( 6, 6 ),
 ( 6, 3, 6 ),
 ( 0.000000000000000000, 0.1274251584810000004 ),
 ( 0.000000000000000000, 0.2500000000000000000, 0.5000000000000000000 ),
 .UNSPECIFIED. ) ;
#6352 = ORIENTED_EDGE ( 'NONE', *, *, #19347, .T. ) ;
#6353 = LINE ( 'NONE', #4024, #9711 ) ;
#6354 = CARTESIAN_POINT ( 'NONE',  ( -12.21857400070000033, -100.8455998110000138, -10.39687837159999972 ) ) ;
#6355 =( LENGTH_UNIT ( ) NAMED_UNIT ( * ) SI_UNIT ( .MILLI., .METRE. ) );
#6356 = CARTESIAN_POINT ( 'NONE',  ( -7.823320741682010748, -100.6644468684844327, 14.83362164074870648 ) ) ;
#6357 = VERTEX_POINT ( 'NONE', #25903 ) ;
#6358 = CARTESIAN_POINT ( 'NONE',  ( 8.543355817900000204, -37.95349900170000268, -21.83354978650000078 ) ) ;
#6359 = CARTESIAN_POINT ( 'NONE',  ( -32.63800352850000053, -74.22019266179999875, -21.66201587429999975 ) ) ;
#6360 = ORIENTED_EDGE ( 'NONE', *, *, #7841, .T. ) ;
#6361 = EDGE_CURVE ( 'NONE', #26131, #19846, #26042, .T. ) ;
#6362 = CARTESIAN_POINT ( 'NONE',  ( 19.72252123670000401, -35.98036830730000446, -9.327645202300001159 ) ) ;
#6363 = CARTESIAN_POINT ( 'NONE',  ( 12.80450062669999944, -92.92146214120000991, 27.55316299560000104 ) ) ;
#6364 = VERTEX_POINT ( 'NONE', #28089 ) ;
#6365 = ADVANCED_FACE ( 'NONE', ( #25488 ), #1486, .T. ) ;
#6366 = CARTESIAN_POINT ( 'NONE',  ( -17.50873242076130509, -93.40025063778267622, -21.36494869218120840 ) ) ;
#6367 = VERTEX_POINT ( 'NONE', #7076 ) ;
#6368 = CARTESIAN_POINT ( 'NONE',  ( 24.26105873420000236, -93.48569624599998917, 12.29345215780000089 ) ) ;
#6369 = CARTESIAN_POINT ( 'NONE',  ( 46.13218886749999825, -73.50000000000000000, -3.897659475159999776 ) ) ;
#6370 = ORIENTED_EDGE ( 'NONE', *, *, #21230, .F. ) ;
#6371 = CARTESIAN_POINT ( 'NONE',  ( -42.13021597025726095, -65.68577269143236208, 0.8025312888707835102 ) ) ;
#6372 = CARTESIAN_POINT ( 'NONE',  ( -21.60034899049999879, -79.50000026560000776, -32.77174743160000503 ) ) ;
#6373 = TOROIDAL_SURFACE ( 'NONE', #6877, 57.54999999999999716, 1.000000000000000000 ) ;
#6374 = ADVANCED_FACE ( 'NONE', ( #15224 ), #142, .F. ) ;
#6375 = AXIS2_PLACEMENT_3D ( 'NONE', #20598, #12117, #25537 ) ;
#6376 = ORIENTED_EDGE ( 'NONE', *, *, #23951, .T. ) ;
#6377 = CARTESIAN_POINT ( 'NONE',  ( -17.94180966909999597, -19.50000000000000000, 18.81731824139999887 ) ) ;
#6378 = CARTESIAN_POINT ( 'NONE',  ( -21.84411882930000104, -92.49537389370000540, -19.67291967990000146 ) ) ;
#6379 = AXIS2_PLACEMENT_3D ( 'NONE', #3649, #23480, #26074 ) ;
#6380 = CARTESIAN_POINT ( 'NONE',  ( -18.01708526109999653, -94.13770192399999814, 18.41653692539999909 ) ) ;
#6381 = VERTEX_POINT ( 'NONE', #2702 ) ;
#6382 = CARTESIAN_POINT ( 'NONE',  ( -42.63274768570000361, -94.00000000000000000, -1.438276615809999992 ) ) ;
#6383 = CARTESIAN_POINT ( 'NONE',  ( 13.07785959079999927, -101.1976625110000043, -9.812318318510000026 ) ) ;
#6384 = CYLINDRICAL_SURFACE ( 'NONE', #19009, 57.74999999999999289 ) ;
#6385 = CYLINDRICAL_SURFACE ( 'NONE', #11406, 9.500000000000001776 ) ;
#6386 = AXIS2_PLACEMENT_3D ( 'NONE', #16524, #11701, #14336 ) ;
#6387 = CARTESIAN_POINT ( 'NONE',  ( 9.901441303826389984, -72.79609598216572408, -26.91377043562950178 ) ) ;
#6388 = FACE_OUTER_BOUND ( 'NONE', #5499, .T. ) ;
#6389 = ORIENTED_EDGE ( 'NONE', *, *, #12891, .T. ) ;
#6390 = CARTESIAN_POINT ( 'NONE',  ( 8.873743607898822106, -64.92653621548541309, -23.73262392692488021 ) ) ;
#6391 = DIRECTION ( 'NONE',  ( 1.000000000000000000, 0.000000000000000000, 0.000000000000000000 ) ) ;
#6392 = CARTESIAN_POINT ( 'NONE',  ( 0.2284267155709999997, -92.50000000000000000, -29.91770779450000362 ) ) ;
#6393 = CARTESIAN_POINT ( 'NONE',  ( 19.60237952920000026, -18.50000000000000000, 8.863026849229999726 ) ) ;
#6394 = CARTESIAN_POINT ( 'NONE',  ( -39.03811165380000148, -65.41419836839999391, 2.576072437790000169 ) ) ;
#6395 = AXIS2_PLACEMENT_3D ( 'NONE', #9992, #19321, #5634 ) ;
#6396 = DIRECTION ( 'NONE',  ( 0.000000000000000000, 0.000000000000000000, 1.000000000000000000 ) ) ;
#6397 = FACE_OUTER_BOUND ( 'NONE', #1745, .T. ) ;
#6398 = VERTEX_POINT ( 'NONE', #6515 ) ;
#6399 = EDGE_CURVE ( 'NONE', #6381, #8240, #27629, .T. ) ;
#6400 = CARTESIAN_POINT ( 'NONE',  ( 22.60964169310000216, -96.07623048240000685, -4.342433871829999070 ) ) ;
#6401 = ORIENTED_EDGE ( 'NONE', *, *, #2956, .F. ) ;
#6402 = CARTESIAN_POINT ( 'NONE',  ( -42.25000000000000000, -65.63577453799999262, -0.7216878364880000563 ) ) ;
#6403 = ORIENTED_EDGE ( 'NONE', *, *, #27600, .F. ) ;
#6404 = EDGE_CURVE ( 'NONE', #8764, #27709, #1533, .T. ) ;
#6405 = CARTESIAN_POINT ( 'NONE',  ( 15.77847589470000145, -100.9405348700000076, 2.296806114620000283 ) ) ;
#6406 = EDGE_CURVE ( 'NONE', #17438, #18837, #20711, .T. ) ;
#6407 = CARTESIAN_POINT ( 'NONE',  ( 8.036479196959999201E-15, -69.00000000000000000, -43.75000000000000000 ) ) ;
#6408 = CARTESIAN_POINT ( 'NONE',  ( -7.984177743680001882, -99.69348480060000384, 15.37172668299999856 ) ) ;
#6409 = CARTESIAN_POINT ( 'NONE',  ( -6.697057311400000046, -97.13885494210001070, -19.48988624889999954 ) ) ;
#6410 = VECTOR ( 'NONE', #5211, 1000.000000000000114 ) ;
#6411 = DIRECTION ( 'NONE',  ( 0.000000000000000000, 1.000000000000000000, 0.000000000000000000 ) ) ;
#6412 = CARTESIAN_POINT ( 'NONE',  ( -20.43934827010000177, -94.59274571439999590, 12.18706707989999849 ) ) ;
#6413 = CARTESIAN_POINT ( 'NONE',  ( -10.66687304220000065, -18.85531889179999965, -19.32093941720000174 ) ) ;
#6414 = DIRECTION ( 'NONE',  ( 0.9999792992113794021, 0.000000000000000000, 0.006434372441712415611 ) ) ;
#6415 = EDGE_LOOP ( 'NONE', ( #22091, #8020, #14355, #23311 ) ) ;
#6416 = TOROIDAL_SURFACE ( 'NONE', #5958, 6.750000000000000000, 0.5000000000000000000 ) ;
#6417 = CARTESIAN_POINT ( 'NONE',  ( 13.61208627270031535, -100.4507315469313653, -10.08440332799037265 ) ) ;
#6418 = CARTESIAN_POINT ( 'NONE',  ( 22.55812702580000106, -34.66943697789999845, -0.5428458454240000508 ) ) ;
#6419 = CARTESIAN_POINT ( 'NONE',  ( 12.04737265770000043, -111.0000000000000000, -10.52904611289999970 ) ) ;
#6420 = CARTESIAN_POINT ( 'NONE',  ( -17.00715350810000004, -99.92967601899998442, 3.484608414699999823 ) ) ;
#6421 = VERTEX_POINT ( 'NONE', #18582 ) ;
#6422 = AXIS2_PLACEMENT_3D ( 'NONE', #2175, #6539, #15399 ) ;
#6423 = DIRECTION ( 'NONE',  ( -1.836909530730000236E-16, 0.000000000000000000, 1.000000000000000000 ) ) ;
#6424 = CARTESIAN_POINT ( 'NONE',  ( -13.18661255610000183, -92.50000050529999385, 26.85581263849999800 ) ) ;
#6425 = CARTESIAN_POINT ( 'NONE',  ( -10.17458377400000025, -18.50000000000000000, -22.50859265919999785 ) ) ;
#6426 = VERTEX_POINT ( 'NONE', #23102 ) ;
#6427 = CARTESIAN_POINT ( 'NONE',  ( -38.25000000000000000, -65.00000000000000000, -2.684678751729999480 ) ) ;
#6428 = EDGE_CURVE ( 'NONE', #8977, #17600, #9817, .T. ) ;
#6429 = CARTESIAN_POINT ( 'NONE',  ( 0.4405410860649999760, -101.0405520670000072, -16.24120667380000071 ) ) ;
#6430 = CARTESIAN_POINT ( 'NONE',  ( 24.28331883913842404, -74.17350752487904231, -30.68182624356128585 ) ) ;
#6431 = CARTESIAN_POINT ( 'NONE',  ( -12.04650979770000063, -69.29982785389999833, -25.46956491610000128 ) ) ;
#6432 = DIRECTION ( 'NONE',  ( 0.000000000000000000, 1.000000000000000000, 0.000000000000000000 ) ) ;
#6433 = CARTESIAN_POINT ( 'NONE',  ( -11.22052832319999816, -34.66889731630000426, -19.66680200659999755 ) ) ;
#6434 = ORIENTED_EDGE ( 'NONE', *, *, #26155, .F. ) ;
#6435 = DIRECTION ( 'NONE',  ( 0.000000000000000000, 1.000000000000000000, 0.000000000000000000 ) ) ;
#6436 = CARTESIAN_POINT ( 'NONE',  ( -15.94967535902879696, -92.55895609343200192, -24.01911116337151597 ) ) ;
#6437 = CIRCLE ( 'NONE', #26955, 1.000000000000000888 ) ;
#6438 = ORIENTED_EDGE ( 'NONE', *, *, #7784, .F. ) ;
#6439 = EDGE_CURVE ( 'NONE', #1612, #3048, #8139, .T. ) ;
#6440 = TOROIDAL_SURFACE ( 'NONE', #22761, 3.500000000000000000, 0.5000000000000000000 ) ;
#6441 = CARTESIAN_POINT ( 'NONE',  ( -13.41727642240000051, -92.50059758980000879, 26.58634259119999754 ) ) ;
#6442 = CARTESIAN_POINT ( 'NONE',  ( 4.581687752772167777, -92.77481473406787416, -30.15399321906782859 ) ) ;
#6443 = CARTESIAN_POINT ( 'NONE',  ( -3.134349734139999732, -94.63960162979999780, 23.52861365520000092 ) ) ;
#6444 = ORIENTED_EDGE ( 'NONE', *, *, #9972, .T. ) ;
#6445 = CARTESIAN_POINT ( 'NONE',  ( 9.396859518459999450, -94.80026553589999594, -22.54656200069999983 ) ) ;
#6446 = CARTESIAN_POINT ( 'NONE',  ( 40.00000000000000000, -69.00000000000000000, 5.456746166030000766E-15 ) ) ;
#6447 = DIRECTION ( 'NONE',  ( -0.8660254037838959196, 0.000000000000000000, 0.5000000000009399148 ) ) ;
#6448 = VERTEX_POINT ( 'NONE', #3004 ) ;
#6449 = CARTESIAN_POINT ( 'NONE',  ( 27.35691629450000306, -72.00000000000000000, -11.81987123310000065 ) ) ;
#6450 = DIRECTION ( 'NONE',  ( 0.7071067811865475727, 0.000000000000000000, 0.7071067811865475727 ) ) ;
#6451 = ORIENTED_EDGE ( 'NONE', *, *, #5635, .F. ) ;
#6452 = DIRECTION ( 'NONE',  ( 0.000000000000000000, 0.000000000000000000, -1.000000000000000000 ) ) ;
#6453 = CARTESIAN_POINT ( 'NONE',  ( 6.717799458580000049, -84.00000000000000000, -40.65853658540000026 ) ) ;
#6454 = ORIENTED_EDGE ( 'NONE', *, *, #3806, .T. ) ;
#6455 = CARTESIAN_POINT ( 'NONE',  ( -1.396721017910000029, -100.9938510739999913, -15.46647101679999992 ) ) ;
#6456 = DIRECTION ( 'NONE',  ( 0.09756097560976667582, 0.000000000000000000, 0.9952295494196654602 ) ) ;
#6457 = DIRECTION ( 'NONE',  ( 0.000000000000000000, 1.000000000000000000, 0.000000000000000000 ) ) ;
#6458 = AXIS2_PLACEMENT_3D ( 'NONE', #21681, #17310, #26203 ) ;
#6459 = DIRECTION ( 'NONE',  ( 0.000000000000000000, 1.000000000000000000, 0.000000000000000000 ) ) ;
#6460 = ORIENTED_EDGE ( 'NONE', *, *, #26020, .F. ) ;
#6461 = CARTESIAN_POINT ( 'NONE',  ( -14.57802700750000113, -101.2141579089999937, 4.464741364610000041 ) ) ;
#6462 = CARTESIAN_POINT ( 'NONE',  ( 28.28064714961420378, -69.93672243438709302, 2.457583639001003295 ) ) ;
#6463 = CARTESIAN_POINT ( 'NONE',  ( -7.177518981630000461, -101.0875971110000080, 13.63542055629999972 ) ) ;
#6464 = CIRCLE ( 'NONE', #23234, 16.00000000000000000 ) ;
#6465 = CONICAL_SURFACE ( 'NONE', #3252, 55.67692378859999280, 1.047197551199999799 ) ;
#6466 = CARTESIAN_POINT ( 'NONE',  ( -36.77200237156692708, -65.13413837703032527, -0.1570406424484263597 ) ) ;
#6467 = B_SPLINE_CURVE_WITH_KNOTS ( 'NONE', 5,
 ( #21004, #18822, #27711, #7750, #14563, #27977 ),
 .UNSPECIFIED., .F., .F.,
 ( 6, 6 ),
 ( 0.000000000000000000, 1.000000000000000000 ),
 .UNSPECIFIED. ) ;
#6468 = EDGE_CURVE ( 'NONE', #21056, #27454, #2961, .T. ) ;
#6469 = CIRCLE ( 'NONE', #26482, 60.66666666670000296 ) ;
#6470 = EDGE_CURVE ( 'NONE', #21012, #15974, #11272, .T. ) ;
#6471 = CARTESIAN_POINT ( 'NONE',  ( 26.37317065237687430, -92.86910576385687932, 13.16124730488680683 ) ) ;
#6472 = CYLINDRICAL_SURFACE ( 'NONE', #11499, 2.999999999999996447 ) ;
#6473 = CARTESIAN_POINT ( 'NONE',  ( -38.25178884604896723, -65.13491442161021894, -2.716526481159466488 ) ) ;
#6474 =( LENGTH_UNIT ( ) NAMED_UNIT ( * ) SI_UNIT ( .MILLI., .METRE. ) );
#6475 = CARTESIAN_POINT ( 'NONE',  ( 20.39090231782646612, -94.79128788299946962, 14.04608546598787910 ) ) ;
#6476 = VERTEX_POINT ( 'NONE', #14210 ) ;
#6477 = CARTESIAN_POINT ( 'NONE',  ( 8.654032102250001302, -18.62337004359999781, -18.91112466639999923 ) ) ;
#6478 = CARTESIAN_POINT ( 'NONE',  ( 22.18469061490000271, -36.06131723480000062, -10.59598294889999970 ) ) ;
#6479 = ADVANCED_FACE ( 'NONE', ( #18434 ), #828, .F. ) ;
#6480 = ORIENTED_EDGE ( 'NONE', *, *, #9377, .T. ) ;
#6481 = CARTESIAN_POINT ( 'NONE',  ( -13.78316409329999814, -60.27285653700000267, 21.13754188760000119 ) ) ;
#6482 = AXIS2_PLACEMENT_3D ( 'NONE', #1001, #7694, #1272 ) ;
#6483 = CARTESIAN_POINT ( 'NONE',  ( 8.887092021739999126, -37.65454143339999860, -22.08144368150000147 ) ) ;
#6484 = CARTESIAN_POINT ( 'NONE',  ( -24.61280144410000048, -93.91547326130000783, -2.656926711870000180 ) ) ;
#6485 = DIRECTION ( 'NONE',  ( 0.000000000000000000, 1.000000000000000000, 0.000000000000000000 ) ) ;
#6486 = CARTESIAN_POINT ( 'NONE',  ( 4.534235129290000123E-15, -79.00000000000000000, -36.25000000000000000 ) ) ;
#6487 = CIRCLE ( 'NONE', #18127, 0.5000000000000004441 ) ;
#6488 = AXIS2_PLACEMENT_3D ( 'NONE', #1033, #5229, #20526 ) ;
#6489 = CARTESIAN_POINT ( 'NONE',  ( 15.50655985760000100, -100.4792519539999915, 4.667916574389999518 ) ) ;
#6490 = EDGE_LOOP ( 'NONE', ( #3090, #7374 ) ) ;
#6491 = CARTESIAN_POINT ( 'NONE',  ( -13.32816333360000094, -99.92967571559999840, -11.12411022969999941 ) ) ;
#6492 = CARTESIAN_POINT ( 'NONE',  ( 7.279149876880000036, -73.90055525929999192, -39.59129699409999859 ) ) ;
#6493 = ORIENTED_EDGE ( 'NONE', *, *, #15750, .T. ) ;
#6494 = CARTESIAN_POINT ( 'NONE',  ( 27.68682485439999752, -32.30000000000000426, 50.68039294919999804 ) ) ;
#6495 = EDGE_LOOP ( 'NONE', ( #15601, #16614, #4734, #1298 ) ) ;
#6496 = DIRECTION ( 'NONE',  ( 0.000000000000000000, 1.000000000000000000, 0.000000000000000000 ) ) ;
#6497 = B_SPLINE_CURVE_WITH_KNOTS ( 'NONE', 5,
 ( #3815, #17212, #16941, #8457, #21589, #1647 ),
 .UNSPECIFIED., .F., .F.,
 ( 6, 6 ),
 ( 0.000000000000000000, 1.000000000000000000 ),
 .UNSPECIFIED. ) ;
#6498 = CARTESIAN_POINT ( 'NONE',  ( -42.41335204520000701, -63.20096189429999356, -1.318420231159999956 ) ) ;
#6499 = CARTESIAN_POINT ( 'NONE',  ( -7.851152467529999512, -74.00000000000000000, 38.40621260480000387 ) ) ;
#6500 = CARTESIAN_POINT ( 'NONE',  ( -14.96437297340000150, -101.1411470200000053, 3.591084556139999773 ) ) ;
#6501 = CARTESIAN_POINT ( 'NONE',  ( 9.975420127400001391, -67.81624775490000445, -25.13735964720000027 ) ) ;
#6502 = CARTESIAN_POINT ( 'NONE',  ( -19.68647263579999773, -57.47571016759999907, 12.70082573810000071 ) ) ;
#6503 = EDGE_LOOP ( 'NONE', ( #1057, #28231, #20214, #23176 ) ) ;
#6504 = CARTESIAN_POINT ( 'NONE',  ( -13.80673513442132183, -68.20222041995040740, 22.71145971957957244 ) ) ;
#6505 = DIRECTION ( 'NONE',  ( -0.9704142011833034598, 0.000000000000000000, -0.2414462220490750932 ) ) ;
#6506 = CARTESIAN_POINT ( 'NONE',  ( -12.35404653890000048, -101.0640712160000021, -10.32358696690000066 ) ) ;
#6507 = ADVANCED_FACE ( 'NONE', ( #5599 ), #979, .F. ) ;
#6508 = CARTESIAN_POINT ( 'NONE',  ( -7.227556247458971406, -73.66327267196029993, 39.42995888277184235 ) ) ;
#6509 = CARTESIAN_POINT ( 'NONE',  ( -40.70731707320000226, -74.50000000000000000, -7.215414233289999757 ) ) ;
#6510 = EDGE_LOOP ( 'NONE', ( #26235, #2459, #7791, #10040, #23414 ) ) ;
#6512 = EDGE_CURVE ( 'NONE', #8949, #19113, #3958, .T. ) ;
#6511 = VECTOR ( 'NONE', #9025, 1000.000000000000000 ) ;
#6513 = AXIS2_PLACEMENT_3D ( 'NONE', #5773, #6198, #17278 ) ;
#6514 = DIRECTION ( 'NONE',  ( 0.7778035323410003032, 0.000000000000000000, 0.6285074900730003300 ) ) ;
#6515 = CARTESIAN_POINT ( 'NONE',  ( 24.39713799250000292, -19.50000027030000282, 1.459766484860000046 ) ) ;
#6516 = VERTEX_POINT ( 'NONE', #18869 ) ;
#6517 = EDGE_CURVE ( 'NONE', #23865, #3774, #11746, .T. ) ;
#6518 = EDGE_CURVE ( 'NONE', #20862, #13903, #5736, .T. ) ;
#6519 = DIRECTION ( 'NONE',  ( 0.000000000000000000, 1.000000000000000000, 0.000000000000000000 ) ) ;
#6520 = FACE_OUTER_BOUND ( 'NONE', #26283, .T. ) ;
#6521 = CARTESIAN_POINT ( 'NONE',  ( 12.77500000340000064, -92.50000200359998814, 27.05403400520000190 ) ) ;
#6522 = EDGE_LOOP ( 'NONE', ( #13192, #9087, #8604, #9743, #10318, #21769 ) ) ;
#6523 = CARTESIAN_POINT ( 'NONE',  ( -41.45000000000000284, -65.14977478849999670, 2.857883832489999776 ) ) ;
#6524 = CARTESIAN_POINT ( 'NONE',  ( -14.03104053434696930, -94.16483583410587244, -21.61783809625667274 ) ) ;
#6525 = VERTEX_POINT ( 'NONE', #20625 ) ;
#6526 = CARTESIAN_POINT ( 'NONE',  ( 19.89027466199999949, -94.80026553589999594, 14.17834266530000065 ) ) ;
#6527 = CARTESIAN_POINT ( 'NONE',  ( -6.717799458580000049, -84.00000000000000000, 40.65853658540000026 ) ) ;
#6528 = ORIENTED_EDGE ( 'NONE', *, *, #26610, .T. ) ;
#6529 = AXIS2_PLACEMENT_3D ( 'NONE', #27339, #3025, #25159 ) ;
#6530 = CARTESIAN_POINT ( 'NONE',  ( -41.79245735104326087, -65.72204893722175711, 1.298727208254003784 ) ) ;
#6531 = DIRECTION ( 'NONE',  ( 0.000000000000000000, 0.000000000000000000, -1.000000000000000000 ) ) ;
#6532 = CIRCLE ( 'NONE', #17704, 6.999999999999999112 ) ;
#6533 = AXIS2_PLACEMENT_3D ( 'NONE', #22109, #17297, #26475 ) ;
#6534 = DIRECTION ( 'NONE',  ( -0.5000000000001900702, 0.000000000000000000, 0.8660254037843290176 ) ) ;
#6535 = DIRECTION ( 'NONE',  ( 1.000000000000000000, 0.000000000000000000, 0.000000000000000000 ) ) ;
#6536 = DIRECTION ( 'NONE',  ( 0.000000000000000000, 1.000000000000000000, 0.000000000000000000 ) ) ;
#6537 = DIRECTION ( 'NONE',  ( 0.000000000000000000, 1.000000000000000000, 0.000000000000000000 ) ) ;
#6538 = CARTESIAN_POINT ( 'NONE',  ( 12.47562891269999952, -101.2902355740000075, -9.903343504470001335 ) ) ;
#6539 = DIRECTION ( 'NONE',  ( -0.000000000000000000, 1.000000000000000000, 0.000000000000000000 ) ) ;
#6540 = CARTESIAN_POINT ( 'NONE',  ( -11.77049175740000209, -94.59276292389999696, -20.68200892780000189 ) ) ;
#6541 = FACE_OUTER_BOUND ( 'NONE', #13499, .T. ) ;
#6542 = CARTESIAN_POINT ( 'NONE',  ( 29.81958713258436688, -92.61393927540532900, 6.406587609757409041 ) ) ;
#6543 = CARTESIAN_POINT ( 'NONE',  ( -17.64372670299999868, -18.50000000000000000, 13.83547606110000139 ) ) ;
#6544 = ORIENTED_EDGE ( 'NONE', *, *, #23044, .T. ) ;
#6545 = EDGE_CURVE ( 'NONE', #10101, #17438, #9893, .T. ) ;
#6546 = CARTESIAN_POINT ( 'NONE',  ( -38.25000000000000000, -63.30468293320000583, 1.587713240270000048 ) ) ;
#6547 = CARTESIAN_POINT ( 'NONE',  ( -16.57262063419999976, -111.0000000000000000, 13.26958147880000105 ) ) ;
#6548 = CARTESIAN_POINT ( 'NONE',  ( -23.82443726134325956, -92.82709422631620555, -19.04327167594423287 ) ) ;
#6549 = DIRECTION ( 'NONE',  ( 0.000000000000000000, 1.000000000000000000, 0.000000000000000000 ) ) ;
#6550 = CARTESIAN_POINT ( 'NONE',  ( 16.79922297439999923, -99.53431386179998697, 4.586272525910000120 ) ) ;
#6551 = AXIS2_PLACEMENT_3D ( 'NONE', #22200, #11251, #2834 ) ;
#6552 = LINE ( 'NONE', #18062, #15408 ) ;
#6553 = AXIS2_PLACEMENT_3D ( 'NONE', #3386, #18967, #7894 ) ;
#6554 = ADVANCED_FACE ( 'NONE', ( #19695 ), #25893, .T. ) ;
#6555 = AXIS2_PLACEMENT_3D ( 'NONE', #35, #19817, #10765 ) ;
#6556 = DIRECTION ( 'NONE',  ( 0.3957342950827466566, 0.000000000000000000, 0.9183650514339936066 ) ) ;
#6557 = DIRECTION ( 'NONE',  ( 0.000000000000000000, 1.000000000000000000, 0.000000000000000000 ) ) ;
#6558 = DIRECTION ( 'NONE',  ( 0.4794255386042041156, 0.000000000000000000, 0.8775825618903720926 ) ) ;
#6559 = EDGE_LOOP ( 'NONE', ( #14882, #16570, #23326 ) ) ;
#6560 = CARTESIAN_POINT ( 'NONE',  ( 21.95870570019999946, -95.72998413979999555, -4.498066912960000607 ) ) ;
#6561 = ORIENTED_EDGE ( 'NONE', *, *, #22702, .T. ) ;
#6562 = CARTESIAN_POINT ( 'NONE',  ( 28.76419640220090912, -72.15620615179069830, 2.906284881040829937 ) ) ;
#6563 = FACE_OUTER_BOUND ( 'NONE', #6818, .T. ) ;
#6564 = ORIENTED_EDGE ( 'NONE', *, *, #19034, .T. ) ;
#6565 = FACE_OUTER_BOUND ( 'NONE', #17245, .T. ) ;
#6566 = ORIENTED_EDGE ( 'NONE', *, *, #25804, .T. ) ;
#6567 = CARTESIAN_POINT ( 'NONE',  ( -11.18835985219999962, -94.77533619469998882, -20.78534805609999836 ) ) ;
#6568 = DIRECTION ( 'NONE',  ( 0.000000000000000000, 1.000000000000000000, 0.000000000000000000 ) ) ;
#6569 = DIRECTION ( 'NONE',  ( -0.000000000000000000, 1.000000000000000000, 0.000000000000000000 ) ) ;
#6570 = CARTESIAN_POINT ( 'NONE',  ( -10.89815230080000141, -18.50000000000000000, -17.99090062400000178 ) ) ;
#6571 = VECTOR ( 'NONE', #9807, 1000.000000000000000 ) ;
#6572 = CARTESIAN_POINT ( 'NONE',  ( 11.60714335010259290, -98.09459568849395339, -16.83342208755517078 ) ) ;
#6573 = ORIENTED_EDGE ( 'NONE', *, *, #9195, .T. ) ;
#6574 = AXIS2_PLACEMENT_3D ( 'NONE', #11075, #4554, #25940 ) ;
#6575 = CARTESIAN_POINT ( 'NONE',  ( -38.55000000000000426, -65.00000000000000000, 2.857883832489999776 ) ) ;
#6576 = VECTOR ( 'NONE', #27650, 999.9999999999998863 ) ;
#6577 = CARTESIAN_POINT ( 'NONE',  ( 23.56468125250000156, -27.03158754569999900, 1.355479213289999985 ) ) ;
#6578 = CARTESIAN_POINT ( 'NONE',  ( 25.14778840239999980, -69.33908554340000308, 11.07326088209999959 ) ) ;
#6579 = CARTESIAN_POINT ( 'NONE',  ( 40.28633210762483685, -74.17816432815648398, 7.244343739438153129 ) ) ;
#6580 = ORIENTED_EDGE ( 'NONE', *, *, #5206, .F. ) ;
#6581 = DIRECTION ( 'NONE',  ( 1.000000000000000000, 0.000000000000000000, 0.000000000000000000 ) ) ;
#6582 = CARTESIAN_POINT ( 'NONE',  ( -14.94824859369999892, -92.53413156150000418, 24.89531834309999780 ) ) ;
#6583 = CARTESIAN_POINT ( 'NONE',  ( -23.24818410940000035, -92.50000000000000000, -18.83197690249999923 ) ) ;
#6584 = ORIENTED_EDGE ( 'NONE', *, *, #1875, .F. ) ;
#6585 = ADVANCED_FACE ( 'NONE', ( #98 ), #2572, .T. ) ;
#6586 = CARTESIAN_POINT ( 'NONE',  ( 0.000000000000000000, -65.07443093669999712, 0.000000000000000000 ) ) ;
#6587 = CARTESIAN_POINT ( 'NONE',  ( 0.7986093652169999890, -100.7776802639999971, -15.78831820859999802 ) ) ;
#6588 = DIRECTION ( 'NONE',  ( 0.000000000000000000, -1.000000000000000000, 0.000000000000000000 ) ) ;
#6589 = CARTESIAN_POINT ( 'NONE',  ( -12.05824332719999958, -67.66818001709999919, -24.37626866669999970 ) ) ;
#6590 = CARTESIAN_POINT ( 'NONE',  ( 24.34110602900000231, -64.48636181450000038, -9.808841899269999942 ) ) ;
#6591 = ORIENTED_EDGE ( 'NONE', *, *, #626, .T. ) ;
#6592 = EDGE_CURVE ( 'NONE', #26789, #10004, #7085, .T. ) ;
#6593 = DIRECTION ( 'NONE',  ( 0.000000000000000000, 1.000000000000000000, 0.000000000000000000 ) ) ;
#6594 = CARTESIAN_POINT ( 'NONE',  ( -11.18243144779999909, -57.47855601759999900, 20.51090144570000007 ) ) ;
#6595 = CARTESIAN_POINT ( 'NONE',  ( 37.60355029590000697, -74.00000000000000000, -9.356041104380000917 ) ) ;
#6596 = AXIS2_PLACEMENT_3D ( 'NONE', #2520, #9633, #11376 ) ;
#6597 = AXIS2_PLACEMENT_3D ( 'NONE', #17189, #3931, #3522 ) ;
#6598 = VERTEX_POINT ( 'NONE', #24853 ) ;
#6599 = CARTESIAN_POINT ( 'NONE',  ( 27.96402436456293117, -92.54687141712491893, 12.17634571817241529 ) ) ;
#6600 = CARTESIAN_POINT ( 'NONE',  ( 16.48132342839999964, -111.0000000000000000, 2.988055897779999803 ) ) ;
#6601 = CARTESIAN_POINT ( 'NONE',  ( -2.934901053329999954, -94.89196973819998959, 23.49669094599999752 ) ) ;
#6602 = CARTESIAN_POINT ( 'NONE',  ( 22.56214152920000160, -93.14733690350000472, 15.53136258500000011 ) ) ;
#6603 = B_SPLINE_SURFACE_WITH_KNOTS ( 'NONE', 5, 5, ( 
 ( #16481, #21414, #1472, #21149, #8015, #25512 ),
 ( #25795, #20865, #10313, #16617, #19226, #5550 ),
 ( #25654, #3511, #3371, #3100, #5684, #1204 ),
 ( #925, #16905, #21275, #5824, #14706, #3641 ),
 ( #5269, #25242, #10448, #26355, #8278, #19367 ),
 ( #3781, #19641, #28242, #28531, #19502, #17178 ) ),
 .UNSPECIFIED., .F., .F., .F.,
 ( 6, 6 ),
 ( 6, 6 ),
 ( 53.49743275559999489, 69.76497130679999259 ),
 ( 0.000000000000000000, 0.5000000000000000000 ),
 .UNSPECIFIED. ) ;
#6604 = EDGE_CURVE ( 'NONE', #24784, #11872, #27311, .T. ) ;
#6605 = DIRECTION ( 'NONE',  ( 1.000000000000000000, 0.000000000000000000, 0.000000000000000000 ) ) ;
#6606 = CARTESIAN_POINT ( 'NONE',  ( -6.850910565599999558, -101.0956037589999994, 13.95379404589999872 ) ) ;
#6607 = VERTEX_POINT ( 'NONE', #546 ) ;
#6608 = CARTESIAN_POINT ( 'NONE',  ( -3.807886452449999570, -80.00000000000000000, 46.75000000000000000 ) ) ;
#6609 = CARTESIAN_POINT ( 'NONE',  ( -13.16293296443088678, -100.0863963178061056, -11.12354968663382238 ) ) ;
#6610 = ORIENTED_EDGE ( 'NONE', *, *, #9903, .F. ) ;
#6611 = CARTESIAN_POINT ( 'NONE',  ( -17.94180966909999597, -19.50000000000000000, 18.81731824139999887 ) ) ;
#6612 = CARTESIAN_POINT ( 'NONE',  ( 21.56931447779999900, -36.56979901409999911, -6.850353625240000355 ) ) ;
#6613 = CARTESIAN_POINT ( 'NONE',  ( 7.007938636740000504, -99.64579651319999698, 15.84020959899999959 ) ) ;
#6614 = AXIS2_PLACEMENT_3D ( 'NONE', #13324, #17429, #105 ) ;
#6615 = LINE ( 'NONE', #22350, #10236 ) ;
#6616 = CARTESIAN_POINT ( 'NONE',  ( -43.23055058677169171, -63.07121106306891534, -0.1555666912528072821 ) ) ;
#6617 = CARTESIAN_POINT ( 'NONE',  ( -19.43609242099999790, -92.50000000000000000, -23.50506990850000122 ) ) ;
#6618 = CARTESIAN_POINT ( 'NONE',  ( 0.000000000000000000, -80.50000000000000000, 0.000000000000000000 ) ) ;
#6619 = CIRCLE ( 'NONE', #2450, 7.249999999999999112 ) ;
#6620 = FACE_OUTER_BOUND ( 'NONE', #13862, .T. ) ;
#6621 = CARTESIAN_POINT ( 'NONE',  ( -8.226221597980000411, -100.1275643909999928, 14.47297520289999895 ) ) ;
#6622 = EDGE_CURVE ( 'NONE', #4330, #24784, #14090, .T. ) ;
#6623 = CARTESIAN_POINT ( 'NONE',  ( -40.00000000000000000, -74.50000000000000000, 2.464695114669999848E-15 ) ) ;
#6624 = LINE ( 'NONE', #19862, #15253 ) ;
#6625 = CARTESIAN_POINT ( 'NONE',  ( -11.98644653210000044, -66.39602363730000434, -23.89227711550000066 ) ) ;
#6626 = CARTESIAN_POINT ( 'NONE',  ( -38.28924667970461826, -65.10052340105359292, -2.810420613934208944 ) ) ;
#6627 = CARTESIAN_POINT ( 'NONE',  ( 15.07154978059999983, -101.2141467319999890, 2.302521054160000080 ) ) ;
#6628 = CARTESIAN_POINT ( 'NONE',  ( 21.46597110810399656, -94.35876167800067549, 13.63254091422909298 ) ) ;
#6629 = ORIENTED_EDGE ( 'NONE', *, *, #18939, .T. ) ;
#6630 = CARTESIAN_POINT ( 'NONE',  ( 8.028473304129999377, -18.50000000000000000, -18.85230009969999898 ) ) ;
#6631 = FACE_OUTER_BOUND ( 'NONE', #14070, .T. ) ;
#6632 = EDGE_LOOP ( 'NONE', ( #20254, #25747, #14340, #26601 ) ) ;
#6633 = CIRCLE ( 'NONE', #2932, 11.00000000000000000 ) ;
#6634 = CARTESIAN_POINT ( 'NONE',  ( -14.19074604640000103, -64.47177095450000195, 21.84081649480000209 ) ) ;
#6635 = DIRECTION ( 'NONE',  ( 1.000000000000000000, 0.000000000000000000, 0.000000000000000000 ) ) ;
#6636 = CARTESIAN_POINT ( 'NONE',  ( -23.69409928740000026, -94.52419443349998573, -3.934983043100000355 ) ) ;
#6637 = AXIS2_PLACEMENT_3D ( 'NONE', #8760, #14457, #21033 ) ;
#6638 = DIRECTION ( 'NONE',  ( 1.000000000000000000, 0.000000000000000000, 0.000000000000000000 ) ) ;
#6639 = DIRECTION ( 'NONE',  ( 0.000000000000000000, -1.000000000000000000, 0.000000000000000000 ) ) ;
#6640 = EDGE_CURVE ( 'NONE', #5430, #19506, #12222, .T. ) ;
#6641 = ORIENTED_EDGE ( 'NONE', *, *, #26296, .F. ) ;
#6642 = DIRECTION ( 'NONE',  ( 0.000000000000000000, 1.000000000000000000, 0.000000000000000000 ) ) ;
#6643 = CARTESIAN_POINT ( 'NONE',  ( -13.41619510559999995, -101.2306310700000012, -9.103917256129998137 ) ) ;
#6644 = ORIENTED_EDGE ( 'NONE', *, *, #3971, .T. ) ;
#6645 = CARTESIAN_POINT ( 'NONE',  ( 7.845180177321567250, -92.53708507728565280, 29.47379534260642586 ) ) ;
#6646 = FACE_OUTER_BOUND ( 'NONE', #10732, .T. ) ;
#6647 = CIRCLE ( 'NONE', #21100, 21.14285714289999873 ) ;
#6648 = CARTESIAN_POINT ( 'NONE',  ( 20.14180068619999631, -45.99906616869999709, 11.02192007709999899 ) ) ;
#6649 = DIRECTION ( 'NONE',  ( 0.000000000000000000, 1.000000000000000000, 0.000000000000000000 ) ) ;
#6650 = CARTESIAN_POINT ( 'NONE',  ( 23.75537003280000192, -92.54628605920001405, -18.53955413979999989 ) ) ;
#6651 = CARTESIAN_POINT ( 'NONE',  ( 19.26420165869999934, -18.61776472269999871, 9.888281526900000173 ) ) ;
#6652 = CARTESIAN_POINT ( 'NONE',  ( 8.558198341779998941, -66.59066310410000256, -24.38877182639999930 ) ) ;
#6653 = CARTESIAN_POINT ( 'NONE',  ( -16.65305080357083867, -98.39905935350182631, 8.896395905759751699 ) ) ;
#6654 = ORIENTED_EDGE ( 'NONE', *, *, #7098, .F. ) ;
#6655 = CIRCLE ( 'NONE', #143, 53.35000000000000142 ) ;
#6656 = CARTESIAN_POINT ( 'NONE',  ( 27.03296752710000206, -72.21526977780000323, -11.52669541869999925 ) ) ;
#6657 = CARTESIAN_POINT ( 'NONE',  ( -12.79195022560000083, -100.5229262450000078, -11.01668120969999976 ) ) ;
#6658 = VECTOR ( 'NONE', #20963, 1000.000000000000000 ) ;
#6659 = CARTESIAN_POINT ( 'NONE',  ( 0.000000000000000000, -108.5000000000000000, 0.000000000000000000 ) ) ;
#6660 = FACE_OUTER_BOUND ( 'NONE', #5508, .T. ) ;
#6661 = ORIENTED_EDGE ( 'NONE', *, *, #3456, .T. ) ;
#6662 = PLANE ( 'NONE',  #9341 ) ;
#6663 = CARTESIAN_POINT ( 'NONE',  ( -32.48735602109999832, -74.14773635299999910, -22.07522367249999817 ) ) ;
#6664 = VERTEX_POINT ( 'NONE', #3429 ) ;
#6665 = CARTESIAN_POINT ( 'NONE',  ( -10.59381889375850960, -19.48875964712268782, -21.30758956286935302 ) ) ;
#6666 = CIRCLE ( 'NONE', #3421, 3.000000000000000000 ) ;
#6667 = CARTESIAN_POINT ( 'NONE',  ( 24.99717791306386161, -43.98373191176955999, 1.386805645287898292 ) ) ;
#6668 = CARTESIAN_POINT ( 'NONE',  ( 12.80450063680000028, -93.00000194650000651, 27.55316300550000008 ) ) ;
#6669 = B_SPLINE_CURVE_WITH_KNOTS ( 'NONE', 5,
 ( #11874, #20786, #25307, #841, #7536, #23111 ),
 .UNSPECIFIED., .F., .F.,
 ( 6, 6 ),
 ( 0.000000000000000000, 1.000000000000000000 ),
 .UNSPECIFIED. ) ;
#6670 = ORIENTED_EDGE ( 'NONE', *, *, #6892, .F. ) ;
#6671 = DIRECTION ( 'NONE',  ( 0.000000000000000000, 1.000000000000000000, 0.000000000000000000 ) ) ;
#6672 = CARTESIAN_POINT ( 'NONE',  ( -19.37994895511149451, -96.88257430336904008, 7.664418457435713705 ) ) ;
#6673 = ORIENTED_EDGE ( 'NONE', *, *, #7253, .T. ) ;
#6674 = CARTESIAN_POINT ( 'NONE',  ( -22.92366483370072672, -71.08353289282860032, 15.88272241998541290 ) ) ;
#6675 = CARTESIAN_POINT ( 'NONE',  ( -12.84659744679999882, -72.82938648530000592, -25.64625568420000334 ) ) ;
#6676 = DIRECTION ( 'NONE',  ( 1.000000000000000000, 0.000000000000000000, 0.000000000000000000 ) ) ;
#6677 = ORIENTED_EDGE ( 'NONE', *, *, #25362, .T. ) ;
#6678 = VECTOR ( 'NONE', #22314, 1000.000000000000000 ) ;
#6679 = CARTESIAN_POINT ( 'NONE',  ( -42.21358016755470288, -65.65208897057404158, 0.7427148365544418152 ) ) ;
#6680 = LINE ( 'NONE', #26493, #28522 ) ;
#6681 = EDGE_CURVE ( 'NONE', #7956, #27080, #13121, .T. ) ;
#6682 = LINE ( 'NONE', #4487, #10838 ) ;
#6683 = EDGE_CURVE ( 'NONE', #25457, #3331, #24304, .T. ) ;
#6684 = MANIFOLD_SOLID_BREP ( 'Rotational Bodies', #21651 ) ;
#6685 = CARTESIAN_POINT ( 'NONE',  ( -16.36167018629999959, -93.01125874779999947, -20.97227418339999971 ) ) ;
#6686 = CARTESIAN_POINT ( 'NONE',  ( 0.000000000000000000, -19.40000000000000213, 0.000000000000000000 ) ) ;
#6687 = ORIENTED_EDGE ( 'NONE', *, *, #13481, .T. ) ;
#6688 = EDGE_CURVE ( 'NONE', #22989, #26789, #4721, .T. ) ;
#6689 = CARTESIAN_POINT ( 'NONE',  ( -6.075137112332721578, -101.5902664364218708, 14.84893169810246327 ) ) ;
#6690 = AXIS2_PLACEMENT_3D ( 'NONE', #18496, #2630, #455 ) ;
#6691 = CARTESIAN_POINT ( 'NONE',  ( 13.77551190490000188, -100.0482783049999966, -10.29143743870000094 ) ) ;
#6692 = CARTESIAN_POINT ( 'NONE',  ( -22.11992770129999997, -74.33689811570000927, -32.70527315500000043 ) ) ;
#6693 = CARTESIAN_POINT ( 'NONE',  ( -1.156001381979999909, -57.47571038090000428, -23.39939166179999930 ) ) ;
#6694 = AXIS2_PLACEMENT_3D ( 'NONE', #5475, #16975, #1267 ) ;
#6695 = CARTESIAN_POINT ( 'NONE',  ( 23.96368475870000125, -111.0000000000000000, 8.717328305520000598 ) ) ;
#6696 = CARTESIAN_POINT ( 'NONE',  ( -38.25000000000000000, -65.14977478849999670, 2.684678751729999480 ) ) ;
#6697 = CARTESIAN_POINT ( 'NONE',  ( 7.479534728624448903, -74.09469053464687249, -39.31221710977964534 ) ) ;
#6698 = EDGE_LOOP ( 'NONE', ( #6591, #9773, #27075, #6211 ) ) ;
#6699 = CARTESIAN_POINT ( 'NONE',  ( 27.11492913210000211, -72.00000000000000000, 10.50528373760000100 ) ) ;
#6700 = DIRECTION ( 'NONE',  ( 0.000000000000000000, 1.000000000000000000, 0.000000000000000000 ) ) ;
#6701 = CARTESIAN_POINT ( 'NONE',  ( -23.86210134984825615, -92.77521214514680992, -18.99609179358898103 ) ) ;
#6702 = PLANE ( 'NONE',  #20985 ) ;
#6703 = CARTESIAN_POINT ( 'NONE',  ( 0.1200718050890000055, -93.00000000000000000, -30.49976365090000030 ) ) ;
#6704 = CARTESIAN_POINT ( 'NONE',  ( -14.74973743588710207, -100.9709810896216027, 4.950683569343071966 ) ) ;
#6705 = APPLICATION_PROTOCOL_DEFINITION ( 'draft international standard', 'automotive_design', 1998, #12005 ) ;
#6706 = CARTESIAN_POINT ( 'NONE',  ( 23.55258138210000141, -57.47122622279999860, 0.3294346322440000474 ) ) ;
#6707 = DIRECTION ( 'NONE',  ( 0.000000000000000000, 0.000000000000000000, -1.000000000000000000 ) ) ;
#6708 = ORIENTED_EDGE ( 'NONE', *, *, #16774, .T. ) ;
#6709 = AXIS2_PLACEMENT_3D ( 'NONE', #17988, #2558, #26442 ) ;
#6710 = CARTESIAN_POINT ( 'NONE',  ( 23.25684308690000179, -94.57749834670001121, -6.685466565999999666 ) ) ;
#6711 = ORIENTED_EDGE ( 'NONE', *, *, #21645, .T. ) ;
#6712 = AXIS2_PLACEMENT_3D ( 'NONE', #14800, #3745, #8382 ) ;
#6713 = CARTESIAN_POINT ( 'NONE',  ( 28.56383486739311550, -72.59720960093795838, 2.210274403918753183 ) ) ;
#6714 = DIRECTION ( 'NONE',  ( 0.000000000000000000, -1.000000000000000000, 0.000000000000000000 ) ) ;
#6715 = EDGE_LOOP ( 'NONE', ( #21260, #21368, #16200, #8715, #20667, #28477 ) ) ;
#6716 = FACE_OUTER_BOUND ( 'NONE', #18420, .T. ) ;
#6717 = EDGE_CURVE ( 'NONE', #18911, #26338, #25574, .T. ) ;
#6718 = CARTESIAN_POINT ( 'NONE',  ( -4.790709198910000133, -98.40794110039999509, -18.33800208579999946 ) ) ;
#6719 = CARTESIAN_POINT ( 'NONE',  ( 7.257715839349999420, -101.2520799100000062, 13.34996420839999942 ) ) ;
#6720 = CARTESIAN_POINT ( 'NONE',  ( -35.88566914520000495, -80.00000000000000000, -26.69328098980000163 ) ) ;
#6721 = CARTESIAN_POINT ( 'NONE',  ( -17.12546904050000052, -99.53431416519998720, 3.156803742540000179 ) ) ;
#6722 = AXIS2_PLACEMENT_3D ( 'NONE', #11858, #27750, #1242 ) ;
#6723 = DIRECTION ( 'NONE',  ( 0.7071067811865474617, 0.000000000000000000, 0.7071067811865474617 ) ) ;
#6724 = CARTESIAN_POINT ( 'NONE',  ( 9.374849361280000792, -94.98812477599999227, -22.63660904189999812 ) ) ;
#6725 = ORIENTED_EDGE ( 'NONE', *, *, #15743, .T. ) ;
#6726 = EDGE_CURVE ( 'NONE', #3127, #17492, #28439, .T. ) ;
#6727 = CARTESIAN_POINT ( 'NONE',  ( 12.19843450850000011, -94.07620464490000245, -21.73166345290000123 ) ) ;
#6728 = DIRECTION ( 'NONE',  ( 0.000000000000000000, 1.000000000000000000, 0.000000000000000000 ) ) ;
#6729 = CARTESIAN_POINT ( 'NONE',  ( -14.93121078260000090, -79.49999975080000070, 36.29905569799999654 ) ) ;
#6730 = CARTESIAN_POINT ( 'NONE',  ( -12.88144346130615148, -92.61393927531646852, 27.64634796700016750 ) ) ;
#6731 = ORIENTED_EDGE ( 'NONE', *, *, #9124, .F. ) ;
#6732 = AXIS2_PLACEMENT_3D ( 'NONE', #7930, #16818, #19145 ) ;
#6733 = CARTESIAN_POINT ( 'NONE',  ( -20.56018235820000228, -57.40875686090000585, 14.85415984670000000 ) ) ;
#6734 = CARTESIAN_POINT ( 'NONE',  ( -15.94773428150000250, -93.01843633099998954, 23.99750656370000002 ) ) ;
#6735 = DIRECTION ( 'NONE',  ( 1.000000000000000000, 0.000000000000000000, 0.000000000000000000 ) ) ;
#6736 = VERTEX_POINT ( 'NONE', #11871 ) ;
#6737 = CARTESIAN_POINT ( 'NONE',  ( 28.37123197869999913, -70.21789636049999217, 2.505359212729999729 ) ) ;
#6738 = AXIS2_PLACEMENT_3D ( 'NONE', #10382, #8496, #15175 ) ;
#6739 = CARTESIAN_POINT ( 'NONE',  ( 1.131980963049999955, -100.1275643909999928, -16.60892386949999988 ) ) ;
#6740 = CARTESIAN_POINT ( 'NONE',  ( 26.04734495227661739, -74.32587665817413836, -29.31966643403540829 ) ) ;
#6741 = FACE_OUTER_BOUND ( 'NONE', #15949, .T. ) ;
#6742 = CARTESIAN_POINT ( 'NONE',  ( 23.88371843180000198, -64.81171329779999724, -9.133376755849999640 ) ) ;
#6743 = CYLINDRICAL_SURFACE ( 'NONE', #17109, 7.250000000000004441 ) ;
#6744 = ORIENTED_EDGE ( 'NONE', *, *, #17538, .T. ) ;
#6745 = CARTESIAN_POINT ( 'NONE',  ( 28.44395825459533711, -92.82334897395243445, 11.00868981448089023 ) ) ;
#6746 = CARTESIAN_POINT ( 'NONE',  ( -11.32307664120000013, -111.0000000000000000, 9.421136869679999748 ) ) ;
#6747 = VECTOR ( 'NONE', #16235, 1000.000000000000000 ) ;
#6748 = EDGE_CURVE ( 'NONE', #26131, #25637, #21997, .T. ) ;
#6749 = CARTESIAN_POINT ( 'NONE',  ( 7.215414233289999757, -74.50000000000000000, 40.70731707320000226 ) ) ;
#6750 = ORIENTED_EDGE ( 'NONE', *, *, #18102, .F. ) ;
#6751 = CARTESIAN_POINT ( 'NONE',  ( 23.56161414842587121, -92.59735406120951495, -19.36752225149772499 ) ) ;
#6752 = DIRECTION ( 'NONE',  ( 1.000000000000000000, 0.000000000000000000, 0.000000000000000000 ) ) ;
#6753 = DIRECTION ( 'NONE',  ( 1.000000000000000000, 0.000000000000000000, 0.000000000000000000 ) ) ;
#6754 = ADVANCED_FACE ( 'NONE', ( #20783 ), #7937, .T. ) ;
#6755 = CARTESIAN_POINT ( 'NONE',  ( 22.73895411410159184, -19.47261671706005970, 1.022399396795566906 ) ) ;
#6756 = ORIENTED_EDGE ( 'NONE', *, *, #23539, .F. ) ;
#6757 = VECTOR ( 'NONE', #7646, 1000.000000000000000 ) ;
#6758 = CARTESIAN_POINT ( 'NONE',  ( 26.80994437584741164, -72.64395437913957210, -10.47635535423811604 ) ) ;
#6759 = DIRECTION ( 'NONE',  ( 0.000000000000000000, -1.000000000000000000, 0.000000000000000000 ) ) ;
#6760 = CARTESIAN_POINT ( 'NONE',  ( 8.371797148759998919, -37.28113868359999827, -21.64024904569999919 ) ) ;
#6761 = CARTESIAN_POINT ( 'NONE',  ( 21.44781821315665837, -35.39811109517434318, -7.092598482907919610 ) ) ;
#6762 = ORIENTED_EDGE ( 'NONE', *, *, #23979, .F. ) ;
#6763 = EDGE_CURVE ( 'NONE', #7139, #9479, #5209, .T. ) ;
#6764 = CARTESIAN_POINT ( 'NONE',  ( 9.335817441729998833, -98.58684426249999433, 16.46450815360000064 ) ) ;
#6765 = B_SPLINE_CURVE_WITH_KNOTS ( 'NONE', 3,
 ( #27064, #24283, #20205, #7108 ),
 .UNSPECIFIED., .F., .F.,
 ( 4, 4 ),
 ( 0.000000000000000000, 1.000000000000000000 ),
 .UNSPECIFIED. ) ;
#6766 = CARTESIAN_POINT ( 'NONE',  ( 40.00000000000000000, -84.00000000000000000, 0.000000000000000000 ) ) ;
#6767 = CYLINDRICAL_SURFACE ( 'NONE', #17261, 4.749999999999999112 ) ;
#6768 = CARTESIAN_POINT ( 'NONE',  ( -19.91159696475570939, -92.54687141712489051, -23.10364386895400912 ) ) ;
#6769 = EDGE_LOOP ( 'NONE', ( #19257, #1673, #19762, #12759 ) ) ;
#6770 = CARTESIAN_POINT ( 'NONE',  ( -15.38634734859999931, -101.2489796309999974, 4.678841008770000975 ) ) ;
#6771 = DIRECTION ( 'NONE',  ( -0.9487039977520664857, 0.000000000000000000, 0.3161656601360223195 ) ) ;
#6772 = CARTESIAN_POINT ( 'NONE',  ( 15.96495049010557565, -94.81439201244758408, 17.25884178542835556 ) ) ;
#6773 = CARTESIAN_POINT ( 'NONE',  ( 13.79877908105553530, -99.99762666413948864, -10.44370536661393878 ) ) ;
#6774 = CARTESIAN_POINT ( 'NONE',  ( -13.15060416100000040, -67.65187322490000099, -22.80468052719999861 ) ) ;
#6775 = CARTESIAN_POINT ( 'NONE',  ( -38.49205360668217679, -65.12158389261927027, -2.883084786666632482 ) ) ;
#6776 = CARTESIAN_POINT ( 'NONE',  ( 24.68551128330313205, -93.11247489649196041, -15.04102508485111578 ) ) ;
#6777 = CARTESIAN_POINT ( 'NONE',  ( 27.46738388089225680, -93.08494709829906810, 9.611772595438951683 ) ) ;
#6778 = ORIENTED_EDGE ( 'NONE', *, *, #8336, .F. ) ;
#6779 = CARTESIAN_POINT ( 'NONE',  ( 36.36887047860000166, -75.00000017930000240, -14.85406792070000037 ) ) ;
#6780 = VERTEX_POINT ( 'NONE', #9680 ) ;
#6781 = CARTESIAN_POINT ( 'NONE',  ( -14.45912934149999884, -67.24379409739999858, 22.35770716749999920 ) ) ;
#6782 = CARTESIAN_POINT ( 'NONE',  ( -12.97028186550000051, -64.93834961630000180, 21.65804104839999766 ) ) ;
#6783 = DIRECTION ( 'NONE',  ( 0.9279287544047433167, 0.000000000000000000, 0.3727575978418970482 ) ) ;
#6784 = CARTESIAN_POINT ( 'NONE',  ( -24.15516222109999944, -94.98812477599999227, -4.102682939769999315 ) ) ;
#6785 = CARTESIAN_POINT ( 'NONE',  ( -19.58536422119999543, -55.03616289790000593, 13.60193610299999989 ) ) ;
#6786 = EDGE_CURVE ( 'NONE', #25949, #14280, #11229, .T. ) ;
#6787 = CARTESIAN_POINT ( 'NONE',  ( 19.92838004652724138, -19.48035124000026741, -8.655192717976913030 ) ) ;
#6788 = CARTESIAN_POINT ( 'NONE',  ( -11.46863496920000003, -57.40875702469999453, -22.62382260909999943 ) ) ;
#6789 = ORIENTED_EDGE ( 'NONE', *, *, #9439, .T. ) ;
#6790 = FACE_OUTER_BOUND ( 'NONE', #15460, .T. ) ;
#6791 = CARTESIAN_POINT ( 'NONE',  ( 28.79684628073619024, -74.38486911952558955, -26.65149887044830734 ) ) ;
#6792 = CARTESIAN_POINT ( 'NONE',  ( 7.260991986019999622, -74.03376265059999639, -40.00088823080000111 ) ) ;
#6793 = VERTEX_POINT ( 'NONE', #26282 ) ;
#6794 = ADVANCED_FACE ( 'NONE', ( #24080 ), #10795, .T. ) ;
#6795 = CARTESIAN_POINT ( 'NONE',  ( 0.000000000000000000, -2.000000000000000000, 0.000000000000000000 ) ) ;
#6796 = CARTESIAN_POINT ( 'NONE',  ( -37.36725231429999639, -81.75000000000000000, 1.438276615809999992 ) ) ;
#6797 = FACE_OUTER_BOUND ( 'NONE', #13504, .T. ) ;
#6798 = CARTESIAN_POINT ( 'NONE',  ( 21.98573708710000219, -45.96202241439999625, 9.944421315929998784 ) ) ;
#6799 = CIRCLE ( 'NONE', #13284, 0.5000000000000004441 ) ;
#6800 = FACE_BOUND ( 'NONE', #16098, .T. ) ;
#6801 = CARTESIAN_POINT ( 'NONE',  ( 24.60702460379999934, -92.65997669530000280, -15.35181526640000094 ) ) ;
#6802 = CARTESIAN_POINT ( 'NONE',  ( 19.91311854129999759, -18.50000000000000000, 8.957432309550000582 ) ) ;
#6803 = CARTESIAN_POINT ( 'NONE',  ( -41.51571301719197038, -65.11307468787710206, 2.895823260651953834 ) ) ;
#6804 = CARTESIAN_POINT ( 'NONE',  ( -16.92961152516845047, -97.87901546888585358, 9.782674744978539394 ) ) ;
#6805 = ORIENTED_EDGE ( 'NONE', *, *, #5285, .F. ) ;
#6806 = CARTESIAN_POINT ( 'NONE',  ( -14.22861622156947092, -68.06112402365553748, 22.55404109828588588 ) ) ;
#6807 = CARTESIAN_POINT ( 'NONE',  ( -22.22906645670000003, -74.50000000000000000, -32.83566817450000030 ) ) ;
#6808 = CYLINDRICAL_SURFACE ( 'NONE', #16014, 5.999999999999999112 ) ;
#6809 = CARTESIAN_POINT ( 'NONE',  ( -40.00088823259999771, -74.03376265130000888, -7.260991985950000505 ) ) ;
#6810 = EDGE_LOOP ( 'NONE', ( #9704, #13954, #23547, #13042, #25183, #21310, #3433, #17543, #12710, #20831, #9332, #21638, #8832, #1262, #8255, #24367, #11266, #16752, #5820, #23904, #12601, #23708, #9906, #25886, #23422, #1399, #10445, #10786 ) ) ;
#6811 = EDGE_CURVE ( 'NONE', #22871, #5855, #1850, .T. ) ;
#6812 = CARTESIAN_POINT ( 'NONE',  ( -11.74592569580000045, -14.00000000000000000, -21.50077276629999901 ) ) ;
#6813 = ORIENTED_EDGE ( 'NONE', *, *, #25839, .T. ) ;
#6814 = DIRECTION ( 'NONE',  ( 0.4794255386042041711, 0.000000000000000000, 0.8775825618903720926 ) ) ;
#6815 = LINE ( 'NONE', #8980, #3762 ) ;
#6816 = DIRECTION ( 'NONE',  ( 0.000000000000000000, 1.000000000000000000, 0.000000000000000000 ) ) ;
#6817 = CARTESIAN_POINT ( 'NONE',  ( 12.02738831950660092, -101.4628082233756174, -10.51158039492587193 ) ) ;
#6818 = EDGE_LOOP ( 'NONE', ( #14207, #7029, #20671, #2515, #24117, #6813, #22991 ) ) ;
#6819 = EDGE_CURVE ( 'NONE', #5488, #6001, #20089, .T. ) ;
#6820 = CARTESIAN_POINT ( 'NONE',  ( 0.000000000000000000, -40.00000000000000000, 0.000000000000000000 ) ) ;
#6821 = ORIENTED_EDGE ( 'NONE', *, *, #4676, .T. ) ;
#6822 = CARTESIAN_POINT ( 'NONE',  ( 0.000000000000000000, -10.08849557519999962, 0.000000000000000000 ) ) ;
#6823 = DIRECTION ( 'NONE',  ( 0.4794255386042041156, 0.000000000000000000, 0.8775825618903722036 ) ) ;
#6824 = CARTESIAN_POINT ( 'NONE',  ( 6.114061450890000415, -93.00000000000000000, -13.40104985119999981 ) ) ;
#6825 = ORIENTED_EDGE ( 'NONE', *, *, #18279, .T. ) ;
#6826 = CARTESIAN_POINT ( 'NONE',  ( -38.90721607023505157, -63.17171877516572209, -2.651645038172750102 ) ) ;
#6827 = CARTESIAN_POINT ( 'NONE',  ( -22.53893513710000107, -80.06168502749999050, -32.36019062569999249 ) ) ;
#6828 = ADVANCED_FACE ( 'NONE', ( #17530 ), #26146, .F. ) ;
#6829 = CARTESIAN_POINT ( 'NONE',  ( 12.23878306329999788, -101.1716782170000073, -9.887962090940000337 ) ) ;
#6830 = DIRECTION ( 'NONE',  ( 1.000000000000000000, 0.000000000000000000, 0.000000000000000000 ) ) ;
#6831 = DIRECTION ( 'NONE',  ( 1.000000000000000000, 0.000000000000000000, 0.000000000000000000 ) ) ;
#6832 = ORIENTED_EDGE ( 'NONE', *, *, #25921, .T. ) ;
#6833 = DIRECTION ( 'NONE',  ( 1.000000000000000000, 0.000000000000000000, 0.000000000000000000 ) ) ;
#6834 = CARTESIAN_POINT ( 'NONE',  ( 13.87966546279999847, -99.77922884479998800, -10.06442417530000100 ) ) ;
#6835 = CARTESIAN_POINT ( 'NONE',  ( -38.71641004229999794, -73.50000000000000000, 7.135467526410000261 ) ) ;
#6836 = CARTESIAN_POINT ( 'NONE',  ( -21.88970062429999786, -74.04477437299999565, -32.25615024759999727 ) ) ;
#6837 = CARTESIAN_POINT ( 'NONE',  ( -1.450349733809999986, -57.47122622300000216, -23.51019145590000292 ) ) ;
#6838 = DIRECTION ( 'NONE',  ( 0.4794255386042041156, 0.000000000000000000, 0.8775825618903722036 ) ) ;
#6839 = DIRECTION ( 'NONE',  ( 0.000000000000000000, -1.000000000000000000, 0.000000000000000000 ) ) ;
#6840 = CARTESIAN_POINT ( 'NONE',  ( -18.58434179929999885, -19.16559685920000078, 13.41605620019999989 ) ) ;
#6841 = ORIENTED_EDGE ( 'NONE', *, *, #3216, .T. ) ;
#6842 = DIRECTION ( 'NONE',  ( 0.4794255386042040601, 0.000000000000000000, 0.8775825618903720926 ) ) ;
#6843 = EDGE_CURVE ( 'NONE', #2923, #2579, #22901, .T. ) ;
#6844 = EDGE_CURVE ( 'NONE', #18811, #7089, #21485, .T. ) ;
#6845 = CARTESIAN_POINT ( 'NONE',  ( 20.30848777263183536, -73.00723796075250505, -31.22327362632934822 ) ) ;
#6846 = CARTESIAN_POINT ( 'NONE',  ( 8.067175576580000396, -93.91547326120000605, -23.40448531159999845 ) ) ;
#6847 = DIRECTION ( 'NONE',  ( 0.000000000000000000, 1.000000000000000000, 0.000000000000000000 ) ) ;
#6848 = DIRECTION ( 'NONE',  ( 0.000000000000000000, 1.000000000000000000, 0.000000000000000000 ) ) ;
#6849 = CARTESIAN_POINT ( 'NONE',  ( -14.71230273950800616, -101.0166390262131983, 4.876656405776244263 ) ) ;
#6850 = B_SPLINE_SURFACE_WITH_KNOTS ( 'NONE', 5, 5, ( 
 ( #13666, #10864, #6827, #15841, #26937, #20223 ),
 ( #13507, #15690, #8687, #141, #22418, #6977 ),
 ( #20367, #8991, #24300, #22126, #11320, #24751 ),
 ( #24451, #24597, #4786, #19916, #4346, #22571 ),
 ( #13065, #4635, #2465, #22263, #8558, #2611 ),
 ( #20078, #11459, #17898, #17461, #26347, #6372 ) ),
 .UNSPECIFIED., .F., .F., .F.,
 ( 6, 6 ),
 ( 6, 6 ),
 ( 2.646611395639999920, 4.419061266649999986 ),
 ( 0.000000000000000000, 0.5000000000000000000 ),
 .UNSPECIFIED. ) ;
#6851 =( LENGTH_UNIT ( ) NAMED_UNIT ( * ) SI_UNIT ( .MILLI., .METRE. ) );
#6852 = EDGE_CURVE ( 'NONE', #8881, #28111, #100, .T. ) ;
#6853 = DIRECTION ( 'NONE',  ( 0.000000000000000000, -1.000000000000000000, 0.000000000000000000 ) ) ;
#6854 = VECTOR ( 'NONE', #27377, 1000.000000000000000 ) ;
#6855 = EDGE_LOOP ( 'NONE', ( #25803, #25733, #25623, #8165 ) ) ;
#6856 = CARTESIAN_POINT ( 'NONE',  ( 16.08037956160000093, -101.3150700380000018, 2.354225989130000141 ) ) ;
#6857 = ORIENTED_EDGE ( 'NONE', *, *, #2617, .F. ) ;
#6858 = DIRECTION ( 'NONE',  ( 1.000000000000000000, 0.000000000000000000, 0.000000000000000000 ) ) ;
#6859 = DIRECTION ( 'NONE',  ( 0.4794255386042000078, 0.000000000000000000, 0.8775825618903743131 ) ) ;
#6860 = ORIENTED_EDGE ( 'NONE', *, *, #13572, .T. ) ;
#6861 = CARTESIAN_POINT ( 'NONE',  ( 13.40713319760000033, -96.04856473240000980, 17.39417937919999702 ) ) ;
#6862 = CIRCLE ( 'NONE', #5477, 0.3500000000000003664 ) ;
#6863 = CARTESIAN_POINT ( 'NONE',  ( 5.750188325161174951, -93.39299082539562846, -27.04284275823775729 ) ) ;
#6864 = CARTESIAN_POINT ( 'NONE',  ( 1.316303147800000017, -94.80026829419999501, 24.39090705379999946 ) ) ;
#6865 = PLANE ( 'NONE',  #9921 ) ;
#6866 = CARTESIAN_POINT ( 'NONE',  ( -9.771355533599999532, -18.50000000000000000, -22.03737773150000123 ) ) ;
#6867 = VERTEX_POINT ( 'NONE', #3840 ) ;
#6868 = CARTESIAN_POINT ( 'NONE',  ( 0.000000000000000000, -11.50000000000000000, 0.000000000000000000 ) ) ;
#6869 = DIRECTION ( 'NONE',  ( 0.000000000000000000, -1.000000000000000000, 0.000000000000000000 ) ) ;
#6870 = DIRECTION ( 'NONE',  ( 1.000000000000000000, 0.000000000000000000, 0.000000000000000000 ) ) ;
#6871 = CARTESIAN_POINT ( 'NONE',  ( -12.43631275050667639, -92.52249206702077799, 27.84938838431781605 ) ) ;
#6872 = VERTEX_POINT ( 'NONE', #10937 ) ;
#6873 = CYLINDRICAL_SURFACE ( 'NONE', #25800, 0.5000000000000004441 ) ;
#6874 = DIRECTION ( 'NONE',  ( 0.000000000000000000, 1.000000000000000000, 0.000000000000000000 ) ) ;
#6875 = DIRECTION ( 'NONE',  ( 1.000000000000000000, 0.000000000000000000, 0.000000000000000000 ) ) ;
#6876 = EDGE_LOOP ( 'NONE', ( #2406, #1090, #23419 ) ) ;
#6877 = AXIS2_PLACEMENT_3D ( 'NONE', #23147, #27233, #23010 ) ;
#6878 = AXIS2_PLACEMENT_3D ( 'NONE', #17532, #3843, #4120 ) ;
#6879 = CARTESIAN_POINT ( 'NONE',  ( -14.79537535560000094, -100.9197064490000031, 5.022278568880000016 ) ) ;
#6880 = CARTESIAN_POINT ( 'NONE',  ( 0.6036065640569999724, -99.94751438429999268, -17.14557600869999732 ) ) ;
#6881 = CARTESIAN_POINT ( 'NONE',  ( 25.44178589691103554, -74.26977420868146851, -29.81503247152727454 ) ) ;
#6882 = CARTESIAN_POINT ( 'NONE',  ( -16.73195129730000374, -84.75000000000000000, -30.62763141000000289 ) ) ;
#6883 = EDGE_CURVE ( 'NONE', #20553, #17731, #1060, .T. ) ;
#6884 = CARTESIAN_POINT ( 'NONE',  ( 23.33413376120000038, -63.63811275439999804, -7.452427173000001126 ) ) ;
#6885 = ADVANCED_FACE ( 'NONE', ( #19708 ), #17050, .T. ) ;
#6886 = DIRECTION ( 'NONE',  ( 0.000000000000000000, 1.000000000000000000, 0.000000000000000000 ) ) ;
#6887 = DIRECTION ( 'NONE',  ( 1.000000000000000000, 0.000000000000000000, 0.000000000000000000 ) ) ;
#6888 = B_SPLINE_CURVE_WITH_KNOTS ( 'NONE', 5,
 ( #21757, #14761, #10511, #6307, #21904, #17101 ),
 .UNSPECIFIED., .F., .F.,
 ( 6, 6 ),
 ( 0.000000000000000000, 1.000000000000000000 ),
 .UNSPECIFIED. ) ;
#6889 = TOROIDAL_SURFACE ( 'NONE', #11033, 14.25000000000000000, 2.000000000000000000 ) ;
#6890 = DIRECTION ( 'NONE',  ( 0.8775825618903722036, 0.000000000000000000, -0.4794255386042041156 ) ) ;
#6891 = EDGE_CURVE ( 'NONE', #4490, #13918, #10607, .T. ) ;
#6892 = EDGE_CURVE ( 'NONE', #4674, #20739, #4226, .T. ) ;
#6893 = ORIENTED_EDGE ( 'NONE', *, *, #2789, .F. ) ;
#6894 = CARTESIAN_POINT ( 'NONE',  ( 28.14643818373028239, -92.62800705134026202, 11.74875853647297319 ) ) ;
#6895 = CARTESIAN_POINT ( 'NONE',  ( -36.25000000000000000, -79.00000000000000000, 2.124561919619999789E-15 ) ) ;
#6896 = EDGE_LOOP ( 'NONE', ( #23084, #27395, #25077, #1532 ) ) ;
#6897 = CARTESIAN_POINT ( 'NONE',  ( 7.260205543919999727, -73.74944613220000633, 39.69269201139999836 ) ) ;
#6898 = CARTESIAN_POINT ( 'NONE',  ( 18.39097457039999739, -93.63284696350000047, 17.05711537220000196 ) ) ;
#6899 = AXIS2_PLACEMENT_3D ( 'NONE', #16462, #24924, #23172 ) ;
#6900 = CARTESIAN_POINT ( 'NONE',  ( 22.21661127598724761, -19.46574300968510229, 0.3417159844211649089 ) ) ;
#6901 = VERTEX_POINT ( 'NONE', #13102 ) ;
#6902 = AXIS2_PLACEMENT_3D ( 'NONE', #17323, #26502, #24168 ) ;
#6903 = CARTESIAN_POINT ( 'NONE',  ( 26.93262652789482559, -72.35629361427136530, -11.21074450457773075 ) ) ;
#6904 = CARTESIAN_POINT ( 'NONE',  ( 8.114520564299999350, -37.85480374339999798, -21.62119288240000259 ) ) ;
#6905 = CARTESIAN_POINT ( 'NONE',  ( 21.39667837337682599, -35.15480553054729285, -7.218929069207992377 ) ) ;
#6906 = ORIENTED_EDGE ( 'NONE', *, *, #6966, .T. ) ;
#6907 = DIRECTION ( 'NONE',  ( 0.3687499999999814260, 0.000000000000000000, -0.9295286103719527793 ) ) ;
#6908 = CARTESIAN_POINT ( 'NONE',  ( -29.52609378599999701, -92.68584525839999344, -0.4443637791730000175 ) ) ;
#6909 = CARTESIAN_POINT ( 'NONE',  ( -3.941341475290000229, -96.93384555679999437, -20.91998619789999836 ) ) ;
#6910 = CARTESIAN_POINT ( 'NONE',  ( -2.616610288655701666, -19.48999941748984810, -23.72428921426985582 ) ) ;
#6911 = ORIENTED_EDGE ( 'NONE', *, *, #25419, .F. ) ;
#6912 = CARTESIAN_POINT ( 'NONE',  ( 11.63640002800000062, -101.0314399550000104, -10.76925615409999892 ) ) ;
#6913 = CYLINDRICAL_SURFACE ( 'NONE', #9730, 0.8000000000000002665 ) ;
#6914 = CARTESIAN_POINT ( 'NONE',  ( -22.71111200904663363, -95.90275866728285337, -5.472871145369948565 ) ) ;
#6915 = CARTESIAN_POINT ( 'NONE',  ( 40.70731707320000226, -84.00000000000000000, 7.215414233289999757 ) ) ;
#6916 = CARTESIAN_POINT ( 'NONE',  ( 21.28200145869999815, -36.23996849270000098, -9.082471821829999570 ) ) ;
#6917 = LINE ( 'NONE', #2254, #27986 ) ;
#6918 = CARTESIAN_POINT ( 'NONE',  ( -38.25000000000000000, -65.14977478849999670, -2.684678751729999480 ) ) ;
#6919 = CARTESIAN_POINT ( 'NONE',  ( 14.98792925300000078, -101.2530993039999885, 2.502342737139999773 ) ) ;
#6920 = CARTESIAN_POINT ( 'NONE',  ( 23.42170070327015807, -93.74885977147994254, 12.68526725471132899 ) ) ;
#6921 = ORIENTED_EDGE ( 'NONE', *, *, #24301, .T. ) ;
#6922 = EDGE_CURVE ( 'NONE', #8136, #7650, #21657, .T. ) ;
#6923 = CARTESIAN_POINT ( 'NONE',  ( 36.70830927769999619, -74.93175448689999030, -14.75000110549999910 ) ) ;
#6924 = AXIS2_PLACEMENT_3D ( 'NONE', #11923, #27097, #27539 ) ;
#6925 = CARTESIAN_POINT ( 'NONE',  ( 7.952856579429999684, -100.9640305859999927, 13.43340132319999825 ) ) ;
#6926 = EDGE_CURVE ( 'NONE', #1588, #6867, #12179, .T. ) ;
#6927 = ORIENTED_EDGE ( 'NONE', *, *, #22923, .T. ) ;
#6928 = CARTESIAN_POINT ( 'NONE',  ( -12.04650752959999949, -69.29982884310000202, -25.46956806489999892 ) ) ;
#6929 = CARTESIAN_POINT ( 'NONE',  ( -11.57811457420000067, -60.59341626269999637, 20.59243238690000410 ) ) ;
#6930 = CARTESIAN_POINT ( 'NONE',  ( 7.244162156032840194, -74.18137224045423750, 40.29089741862549801 ) ) ;
#6931 = DIRECTION ( 'NONE',  ( 0.000000000000000000, 1.000000000000000000, 0.000000000000000000 ) ) ;
#6932 = DIRECTION ( 'NONE',  ( 0.000000000000000000, 1.000000000000000000, 0.000000000000000000 ) ) ;
#6933 = DIRECTION ( 'NONE',  ( 1.000000000000000000, 0.000000000000000000, 0.000000000000000000 ) ) ;
#6934 = CARTESIAN_POINT ( 'NONE',  ( 15.95399948070000029, -100.1340845430000002, 4.725790154640000296 ) ) ;
#6935 = ORIENTED_EDGE ( 'NONE', *, *, #24540, .F. ) ;
#6936 = CIRCLE ( 'NONE', #12033, 0.4999999999999995559 ) ;
#6937 = CARTESIAN_POINT ( 'NONE',  ( 11.27094287870000144, -92.51078253369999516, 27.07599673740000057 ) ) ;
#6938 = CARTESIAN_POINT ( 'NONE',  ( -41.09278392978337990, -63.17171877516095435, 2.651645038183386482 ) ) ;
#6939 = ORIENTED_EDGE ( 'NONE', *, *, #20230, .T. ) ;
#6940 = DIRECTION ( 'NONE',  ( 1.000000000000000000, 0.000000000000000000, 0.000000000000000000 ) ) ;
#6941 = ORIENTED_EDGE ( 'NONE', *, *, #23278, .F. ) ;
#6942 = AXIS2_PLACEMENT_3D ( 'NONE', #14700, #5678, #12090 ) ;
#6943 = AXIS2_PLACEMENT_3D ( 'NONE', #3035, #20799, #27502 ) ;
#6944 = CARTESIAN_POINT ( 'NONE',  ( 20.34628061889999984, -52.63293862049999916, 11.13082833170000008 ) ) ;
#6945 = AXIS2_PLACEMENT_3D ( 'NONE', #3095, #7747, #16613 ) ;
#6946 = CARTESIAN_POINT ( 'NONE',  ( 0.000000000000000000, -38.34400911419999858, 0.000000000000000000 ) ) ;
#6947 = TOROIDAL_SURFACE ( 'NONE', #1386, 60.66666666670000296, 10.00000000000000000 ) ;
#6948 = CARTESIAN_POINT ( 'NONE',  ( 22.07840668539999740, -19.40610837500000230, 9.666972891260000367 ) ) ;
#6949 = FACE_OUTER_BOUND ( 'NONE', #19108, .T. ) ;
#6950 = DIRECTION ( 'NONE',  ( 1.000000000000000000, 0.000000000000000000, 0.000000000000000000 ) ) ;
#6951 = DIRECTION ( 'NONE',  ( -0.000000000000000000, 1.000000000000000000, 0.000000000000000000 ) ) ;
#6952 = DIRECTION ( 'NONE',  ( 0.000000000000000000, -1.000000000000000000, 0.000000000000000000 ) ) ;
#6953 = CARTESIAN_POINT ( 'NONE',  ( -16.09618210462868504, -99.28123783267172087, 7.460060003079973967 ) ) ;
#6954 = ORIENTED_EDGE ( 'NONE', *, *, #24072, .F. ) ;
#6955 = DIRECTION ( 'NONE',  ( 0.9942974773630094409, 0.000000000000000000, -0.1066420485059984408 ) ) ;
#6956 = CARTESIAN_POINT ( 'NONE',  ( 5.273680924649999824, -107.1975888269999899, 9.653408180790000515 ) ) ;
#6957 = CARTESIAN_POINT ( 'NONE',  ( -12.65137342600000103, -100.3517545579999961, -10.97941968159999959 ) ) ;
#6958 = CARTESIAN_POINT ( 'NONE',  ( 20.83060772838619457, -19.47440675036266100, 9.481471874783228060 ) ) ;
#6959 = CARTESIAN_POINT ( 'NONE',  ( 23.26489703562036127, -63.25226117637114243, -7.438063082557897943 ) ) ;
#6960 = ORIENTED_EDGE ( 'NONE', *, *, #18432, .T. ) ;
#6961 = ADVANCED_FACE ( 'NONE', ( #10756 ), #15991, .T. ) ;
#6962 = AXIS2_PLACEMENT_3D ( 'NONE', #20801, #20655, #16259 ) ;
#6963 = DIRECTION ( 'NONE',  ( -0.7071067811865475727, 0.000000000000000000, 0.7071067811865475727 ) ) ;
#6964 = ORIENTED_EDGE ( 'NONE', *, *, #25734, .T. ) ;
#6965 = AXIS2_PLACEMENT_3D ( 'NONE', #24075, #23939, #3978 ) ;
#6966 = EDGE_CURVE ( 'NONE', #24664, #25480, #24285, .T. ) ;
#6967 = AXIS2_PLACEMENT_3D ( 'NONE', #15051, #26737, #6324 ) ;
#6968 = CARTESIAN_POINT ( 'NONE',  ( -10.93437413680000070, -19.50000027030000282, -21.85842452360000010 ) ) ;
#6969 = CARTESIAN_POINT ( 'NONE',  ( 10.50444872630000148, -92.78939691329999562, 27.51880632769999835 ) ) ;
#6970 = ORIENTED_EDGE ( 'NONE', *, *, #15368, .F. ) ;
#6971 = EDGE_LOOP ( 'NONE', ( #4972, #14678, #12232, #23322 ) ) ;
#6972 = CARTESIAN_POINT ( 'NONE',  ( -21.79612357827979707, -66.42276310376364279, 13.73860294033563356 ) ) ;
#6973 = CARTESIAN_POINT ( 'NONE',  ( 20.30842400699999928, -94.18458655290000081, 13.41360490589999976 ) ) ;
#6974 = CARTESIAN_POINT ( 'NONE',  ( -3.835404308829999831, -16.50000000000000000, -7.020660495120000455 ) ) ;
#6975 = ORIENTED_EDGE ( 'NONE', *, *, #10244, .T. ) ;
#6976 = LINE ( 'NONE', #13665, #21998 ) ;
#6977 = CARTESIAN_POINT ( 'NONE',  ( -22.17563740510000159, -80.50000000000000000, -32.38675284270000532 ) ) ;
#6978 = EDGE_CURVE ( 'NONE', #25061, #726, #430, .T. ) ;
#6979 = DIRECTION ( 'NONE',  ( 0.000000000000000000, -1.000000000000000000, 0.000000000000000000 ) ) ;
#6980 = FACE_OUTER_BOUND ( 'NONE', #15337, .T. ) ;
#6981 = CARTESIAN_POINT ( 'NONE',  ( -24.15516222759999820, -94.98812477599999227, -4.102682929219999330 ) ) ;
#6982 = ORIENTED_EDGE ( 'NONE', *, *, #12072, .T. ) ;
#6983 = CIRCLE ( 'NONE', #5588, 38.75000000000000000 ) ;
#6984 = AXIS2_PLACEMENT_3D ( 'NONE', #6618, #3600, #10005 ) ;
#6985 = CARTESIAN_POINT ( 'NONE',  ( -6.105475123031572693, -101.6077248516953091, 14.82224783260342882 ) ) ;
#6986 = CARTESIAN_POINT ( 'NONE',  ( -16.99294773969999994, -99.88067626670000720, 3.462731254189999941 ) ) ;
#6987 = CARTESIAN_POINT ( 'NONE',  ( -10.20110288159999890, -80.00000000000000000, 41.00000000000000000 ) ) ;
#6988 = CARTESIAN_POINT ( 'NONE',  ( -21.85457041760000152, -74.50000000000000000, -32.66023292159999869 ) ) ;
#6989 = CARTESIAN_POINT ( 'NONE',  ( 10.35605037799999906, -12.64149019679999952, 18.95662306240000206 ) ) ;
#6990 = DIRECTION ( 'NONE',  ( 0.000000000000000000, 1.000000000000000000, 0.000000000000000000 ) ) ;
#6991 = CARTESIAN_POINT ( 'NONE',  ( -7.486742987080038603, -73.99989313545945890, 38.95798903407855107 ) ) ;
#6992 = CARTESIAN_POINT ( 'NONE',  ( -18.28420043339999879, -18.85622860559999836, 12.72554403070000184 ) ) ;
#6993 = ORIENTED_EDGE ( 'NONE', *, *, #4298, .F. ) ;
#6995 = ADVANCED_FACE ( 'NONE', ( #5071 ), #21793, .F. ) ;
#6994 = CARTESIAN_POINT ( 'NONE',  ( -8.404838270569999992, -94.10247623609998868, -22.94303993669999997 ) ) ;
#6996 = CARTESIAN_POINT ( 'NONE',  ( 1.353583911619999998E-12, -74.50000000000000000, 1.342925770590000058E-12 ) ) ;
#6997 = CARTESIAN_POINT ( 'NONE',  ( 8.776868765820001528, -35.24001315249999777, -20.49278548850000092 ) ) ;
#6998 = CARTESIAN_POINT ( 'NONE',  ( 15.99276245056722701, -100.9510322832866223, 4.232737490328940311 ) ) ;
#6999 = CYLINDRICAL_SURFACE ( 'NONE', #13505, 4.749999999999999112 ) ;
#7000 = CARTESIAN_POINT ( 'NONE',  ( 46.91789432950000105, -79.86049234800000818, -2.756977921009999832 ) ) ;
#7001 = CIRCLE ( 'NONE', #2359, 1.999999999999999556 ) ;
#7002 = CARTESIAN_POINT ( 'NONE',  ( 19.49544348199999888, -35.50000000000000000, -8.986258402430001624 ) ) ;
#7003 = AXIS2_PLACEMENT_3D ( 'NONE', #24233, #6014, #23944 ) ;
#7004 = ORIENTED_EDGE ( 'NONE', *, *, #19062, .F. ) ;
#7005 = CARTESIAN_POINT ( 'NONE',  ( 46.84518809242615589, -73.94545411799823853, -2.389775450614370911 ) ) ;
#7006 = ORIENTED_EDGE ( 'NONE', *, *, #25539, .T. ) ;
#7007 = B_SPLINE_CURVE_WITH_KNOTS ( 'NONE', 5,
 ( #10977, #13329, #13482, #15813, #4607, #24725, #22236, #22390, #2436, #13635, #18012, #22543 ),
 .UNSPECIFIED., .F., .F.,
 ( 6, 3, 3, 6 ),
 ( 112.4516932879999871, 115.4092999559999981, 122.7593676410000114, 122.9563471670000041 ),
 .UNSPECIFIED. ) ;
#7008 = DIRECTION ( 'NONE',  ( 0.000000000000000000, 1.000000000000000000, 0.000000000000000000 ) ) ;
#7009 = DIRECTION ( 'NONE',  ( 0.000000000000000000, -1.000000000000000000, 0.000000000000000000 ) ) ;
#7010 = EDGE_LOOP ( 'NONE', ( #24743, #25985, #20685, #547 ) ) ;
#7011 = CARTESIAN_POINT ( 'NONE',  ( 13.51459830149999952, -96.25026288549999265, 17.16122692649999948 ) ) ;
#7012 = EDGE_CURVE ( 'NONE', #5746, #21862, #7077, .T. ) ;
#7013 = CARTESIAN_POINT ( 'NONE',  ( 6.184287104840868743, -93.48480241466988616, -26.64338075428234376 ) ) ;
#7014 = B_SPLINE_CURVE_WITH_KNOTS ( 'NONE', 5,
 ( #19735, #252, #7082, #13617, #688, #11417 ),
 .UNSPECIFIED., .F., .F.,
 ( 6, 6 ),
 ( -4.007730545210000273, -3.491867373409999864 ),
 .UNSPECIFIED. ) ;
#7015 = DIRECTION ( 'NONE',  ( -0.7071067811865470176, 0.000000000000000000, -0.7071067811865480168 ) ) ;
#7016 = CARTESIAN_POINT ( 'NONE',  ( -18.94125844690000093, -97.58046871240000542, 6.456825720490000364 ) ) ;
#7017 = CARTESIAN_POINT ( 'NONE',  ( 27.49607050420000220, -67.46050995630001523, 1.934818144049999855 ) ) ;
#7018 = CARTESIAN_POINT ( 'NONE',  ( 21.61406585437034522, -37.81672230097021981, -8.081625354649236925 ) ) ;
#7019 = EDGE_LOOP ( 'NONE', ( #13028, #18071, #12083, #7632 ) ) ;
#7020 = CARTESIAN_POINT ( 'NONE',  ( 8.907716207360000027, -92.51556042380001088, -27.33482343870000264 ) ) ;
#7021 = DIRECTION ( 'NONE',  ( 0.4794255386042041156, 0.000000000000000000, 0.8775825618903722036 ) ) ;
#7022 = CARTESIAN_POINT ( 'NONE',  ( 40.70731707320000226, -74.50000000000000000, 7.215414233289999757 ) ) ;
#7023 = ORIENTED_EDGE ( 'NONE', *, *, #25738, .T. ) ;
#7024 = EDGE_CURVE ( 'NONE', #5596, #28180, #11559, .T. ) ;
#7025 = TOROIDAL_SURFACE ( 'NONE', #6551, 5.500000000000000000, 0.5000000000000000000 ) ;
#7026 = CYLINDRICAL_SURFACE ( 'NONE', #21583, 20.64285714290000229 ) ;
#7027 = DIRECTION ( 'NONE',  ( 0.000000000000000000, -1.000000000000000000, 0.000000000000000000 ) ) ;
#7028 = CARTESIAN_POINT ( 'NONE',  ( -3.252988965690000178, -74.00000000000000000, -30.32986301179999700 ) ) ;
#7029 = ORIENTED_EDGE ( 'NONE', *, *, #10049, .T. ) ;
#7030 = VECTOR ( 'NONE', #22337, 1000.000000000000000 ) ;
#7031 = LINE ( 'NONE', #11516, #9538 ) ;
#7032 = AXIS2_PLACEMENT_3D ( 'NONE', #4327, #8391, #2150 ) ;
#7033 = CARTESIAN_POINT ( 'NONE',  ( -20.45998242170000125, -52.56313962710000709, 14.78974999389999923 ) ) ;
#7034 = CARTESIAN_POINT ( 'NONE',  ( 25.93996424029923986, -74.31568735978206064, -29.40961401139750109 ) ) ;
#7035 = CARTESIAN_POINT ( 'NONE',  ( 27.68682485439999752, -24.50000000000000000, 50.68039294919999804 ) ) ;
#7036 = CARTESIAN_POINT ( 'NONE',  ( 0.000000000000000000, -26.29689110869999880, 0.000000000000000000 ) ) ;
#7037 = CARTESIAN_POINT ( 'NONE',  ( 27.31181567105563346, -69.82812541820754859, 0.5419601338490444009 ) ) ;
#7038 = PLANE ( 'NONE',  #22388 ) ;
#7039 = ORIENTED_EDGE ( 'NONE', *, *, #26322, .T. ) ;
#7040 = CARTESIAN_POINT ( 'NONE',  ( 10.16215846479999918, -36.06062539180000215, -21.41592806629999757 ) ) ;
#7041 = CARTESIAN_POINT ( 'NONE',  ( 28.20244470975386974, -92.65976904079265353, 11.61346045625293577 ) ) ;
#7042 = FACE_OUTER_BOUND ( 'NONE', #13246, .T. ) ;
#7043 = VERTEX_POINT ( 'NONE', #12050 ) ;
#7044 = AXIS2_PLACEMENT_3D ( 'NONE', #22912, #2950, #20725 ) ;
#7045 = CARTESIAN_POINT ( 'NONE',  ( 7.261004788010000155, -74.03378462380000258, 40.00100507770000036 ) ) ;
#7046 = CARTESIAN_POINT ( 'NONE',  ( -20.20541094980000096, -94.98812148390000232, 12.40015412250000004 ) ) ;
#7047 = AXIS2_PLACEMENT_3D ( 'NONE', #11448, #17592, #15829 ) ;
#7048 = TOROIDAL_SURFACE ( 'NONE', #8863, 24.50000000000000000, 3.000000000000000000 ) ;
#7049 = CARTESIAN_POINT ( 'NONE',  ( 23.53415771673985191, -19.48509740633723908, 1.431415487266915365 ) ) ;
#7050 = CARTESIAN_POINT ( 'NONE',  ( -6.851093861369999871, -101.2010924020000004, 13.63775431790000070 ) ) ;
#7051 = CARTESIAN_POINT ( 'NONE',  ( -3.562216348787903275, -80.34292033684900503, 46.31451622703009718 ) ) ;
#7052 = CARTESIAN_POINT ( 'NONE',  ( -12.45052468959800507, -101.4085864806826720, -10.34185987599518874 ) ) ;
#7053 = AXIS2_PLACEMENT_3D ( 'NONE', #17869, #28634, #17573 ) ;
#7054 = CARTESIAN_POINT ( 'NONE',  ( 8.310288928540000342, -37.22172731869999751, -21.60320471790000241 ) ) ;
#7055 = EDGE_CURVE ( 'NONE', #8407, #10083, #27854, .T. ) ;
#7056 = CARTESIAN_POINT ( 'NONE',  ( -36.91568593819999933, -65.21397798589998729, -0.2399963883289999989 ) ) ;
#7057 = ADVANCED_FACE ( 'NONE', ( #23145 ), #10740, .F. ) ;
#7058 = DIRECTION ( 'NONE',  ( 1.000000000000000000, 0.000000000000000000, 0.000000000000000000 ) ) ;
#7059 = DIRECTION ( 'NONE',  ( 0.000000000000000000, 1.000000000000000000, 0.000000000000000000 ) ) ;
#7060 = CARTESIAN_POINT ( 'NONE',  ( -2.230088632699999796, -97.73638926269998706, -19.83206999720000141 ) ) ;
#7061 = CARTESIAN_POINT ( 'NONE',  ( -0.8753677514297800721, -19.46426558493637060, -22.01818526256528230 ) ) ;
#7062 = EDGE_CURVE ( 'NONE', #14956, #24995, #7449, .T. ) ;
#7063 = DIRECTION ( 'NONE',  ( 0.4794255386042041156, 0.000000000000000000, 0.8775825618903722036 ) ) ;
#7064 = CARTESIAN_POINT ( 'NONE',  ( -13.46276276179999876, -19.49999999970000175, 20.39865906480000035 ) ) ;
#7065 = CARTESIAN_POINT ( 'NONE',  ( -18.51512085397209972, -98.37417905202403290, -7.778978700159559168 ) ) ;
#7066 = ADVANCED_FACE ( 'NONE', ( #4124 ), #2745, .F. ) ;
#7067 = LINE ( 'NONE', #24833, #23065 ) ;
#7068 = CARTESIAN_POINT ( 'NONE',  ( -12.06432294940000105, -66.82248673960000929, -24.54885029159999732 ) ) ;
#7069 = CARTESIAN_POINT ( 'NONE',  ( -11.32307664120000013, -93.00000000000000000, 9.421136869679999748 ) ) ;
#7070 = CARTESIAN_POINT ( 'NONE',  ( 24.73091569213457674, -93.38554229052955691, -12.41662862040795723 ) ) ;
#7071 = CARTESIAN_POINT ( 'NONE',  ( 27.36513940969999936, -93.00000000000000000, 13.03937715500000039 ) ) ;
#7072 = CONICAL_SURFACE ( 'NONE', #14025, 53.75557630319999447, 1.380808038880000144 ) ;
#7073 = EDGE_LOOP ( 'NONE', ( #12750, #16646, #4920, #19700 ) ) ;
#7074 = AXIS2_PLACEMENT_3D ( 'NONE', #11870, #25304, #9679 ) ;
#7075 = CARTESIAN_POINT ( 'NONE',  ( 36.37213528550000774, -74.83007510990000810, -14.84647098600000170 ) ) ;
#7076 = CARTESIAN_POINT ( 'NONE',  ( -9.356041104380000917, -74.00000000000000000, -37.60355029590000697 ) ) ;
#7077 = B_SPLINE_CURVE_WITH_KNOTS ( 'NONE', 3,
 ( #7710, #24895, #16134, #590, #13807, #23008, #1026, #9866, #11609, #22713 ),
 .UNSPECIFIED., .F., .F.,
 ( 4, 2, 2, 2, 4 ),
 ( 0.000000000000000000, 0.2500000000000000000, 0.5000000000000000000, 0.7500000000000000000, 1.000000000000000000 ),
 .UNSPECIFIED. ) ;
#7078 = CARTESIAN_POINT ( 'NONE',  ( 7.816430931350000222, -101.0685486349999991, 13.30758411539999919 ) ) ;
#7079 = CARTESIAN_POINT ( 'NONE',  ( 22.51817718370000065, -95.94970068820001075, -0.7108459635960000522 ) ) ;
#7080 = CARTESIAN_POINT ( 'NONE',  ( -11.77384491379999965, -59.03025262839999954, 20.31645086680000389 ) ) ;
#7081 = DIRECTION ( 'NONE',  ( 0.000000000000000000, -1.000000000000000000, 0.000000000000000000 ) ) ;
#7082 = CARTESIAN_POINT ( 'NONE',  ( 20.21912291310000143, -36.00000000000000000, -9.726844800120000301 ) ) ;
#7083 = CARTESIAN_POINT ( 'NONE',  ( 18.93809058890547448, -18.60284036879449943, 10.27270654917301762 ) ) ;
#7084 = CARTESIAN_POINT ( 'NONE',  ( -11.90443957499999961, -64.24504445130001784, -23.68393584109999850 ) ) ;
#7085 = LINE ( 'NONE', #15948, #13615 ) ;
#7086 = VERTEX_POINT ( 'NONE', #5645 ) ;
#7087 = CARTESIAN_POINT ( 'NONE',  ( -7.256994698139999755, -74.37142462010000088, -40.28432270869999599 ) ) ;
#7088 = CARTESIAN_POINT ( 'NONE',  ( -23.55554596629999864, -94.54719592040000009, -3.773182298170000060 ) ) ;
#7089 = VERTEX_POINT ( 'NONE', #8344 ) ;
#7090 = AXIS2_PLACEMENT_3D ( 'NONE', #3751, #6063, #14942 ) ;
#7091 = CARTESIAN_POINT ( 'NONE',  ( -30.48995558417433216, -92.50638022835022412, 0.7959123993752857951 ) ) ;
#7092 = ORIENTED_EDGE ( 'NONE', *, *, #22845, .F. ) ;
#7093 = EDGE_CURVE ( 'NONE', #25766, #4968, #25980, .T. ) ;
#7094 = CARTESIAN_POINT ( 'NONE',  ( 20.94731949980000252, -52.62618816489948159, 10.41165191589998962 ) ) ;
#7095 = CARTESIAN_POINT ( 'NONE',  ( -6.858694523154360567, -97.53591929605553901, 18.86159558765225341 ) ) ;
#7096 = CARTESIAN_POINT ( 'NONE',  ( -13.14566783280000095, -99.53431386179998697, -11.42099844400000030 ) ) ;
#7097 = CARTESIAN_POINT ( 'NONE',  ( -7.239203719582017804, -74.26034152684405854, -40.39659210438060200 ) ) ;
#7098 = EDGE_CURVE ( 'NONE', #25224, #20206, #19029, .T. ) ;
#7099 = CARTESIAN_POINT ( 'NONE',  ( 19.35838836099999938, -19.15810970359999743, 10.50069124240000029 ) ) ;
#7100 = CARTESIAN_POINT ( 'NONE',  ( -21.54806777370000148, -66.92971392940000896, 14.85312681689999970 ) ) ;
#7101 = CARTESIAN_POINT ( 'NONE',  ( -17.03020756475430275, -97.66307011826351925, 10.16080538950990331 ) ) ;
#7102 = B_SPLINE_SURFACE_WITH_KNOTS ( 'NONE', 5, 5, ( 
 ( #6242, #12782, #27976, #3509, #17175, #8013 ),
 ( #5822, #12918, #10311, #7876, #8276, #26063 ),
 ( #16757, #6091, #14833, #3779, #12639, #5682 ),
 ( #14562, #21553, #8414, #1608, #23469, #10579 ),
 ( #12366, #16903, #1329, #17321, #14969, #25793 ),
 ( #19500, #15106, #19224, #21690, #10446, #3639 ) ),
 .UNSPECIFIED., .F., .F., .F.,
 ( 6, 6 ),
 ( 6, 6 ),
 ( 15.82768567759999989, 30.79603606510000091 ),
 ( 0.000000000000000000, 0.5000000000000000000 ),
 .UNSPECIFIED. ) ;
#7103 = ORIENTED_EDGE ( 'NONE', *, *, #15393, .T. ) ;
#7104 = PLANE ( 'NONE',  #3235 ) ;
#7105 = CARTESIAN_POINT ( 'NONE',  ( 26.80851110240000068, -72.43053626620000784, -11.12358378779999946 ) ) ;
#7106 = CARTESIAN_POINT ( 'NONE',  ( -13.17630453619999997, -99.61736775859999682, -11.27972924090000006 ) ) ;
#7107 = CARTESIAN_POINT ( 'NONE',  ( 21.05437574795876188, -19.47731532787699038, 9.460113418286871578 ) ) ;
#7108 = CARTESIAN_POINT ( 'NONE',  ( -36.79999999999999716, -63.07912966450000880, 0.1732050807570000017 ) ) ;
#7109 = EDGE_LOOP ( 'NONE', ( #15317, #431, #4580, #26345 ) ) ;
#7110 = AXIS2_PLACEMENT_3D ( 'NONE', #6795, #10834, #2134 ) ;
#7111 = FACE_OUTER_BOUND ( 'NONE', #23761, .T. ) ;
#7112 = EDGE_LOOP ( 'NONE', ( #26747, #1860, #23308, #24440 ) ) ;
#7113 = CIRCLE ( 'NONE', #23829, 28.68388914670000034 ) ;
#7114 = CARTESIAN_POINT ( 'NONE',  ( -1.776356839399999804E-15, -19.00000000000000000, 0.000000000000000000 ) ) ;
#7115 = DIRECTION ( 'NONE',  ( 0.000000000000000000, 1.000000000000000000, 0.000000000000000000 ) ) ;
#7116 = CARTESIAN_POINT ( 'NONE',  ( 5.602404968130000107, -93.19697538779999491, 26.61643030870000004 ) ) ;
#7117 = ORIENTED_EDGE ( 'NONE', *, *, #17777, .T. ) ;
#7118 = VERTEX_POINT ( 'NONE', #6166 ) ;
#7119 = FACE_OUTER_BOUND ( 'NONE', #10241, .T. ) ;
#7120 = CARTESIAN_POINT ( 'NONE',  ( -17.13033212710000086, -72.00000000000000000, 23.49748962700000021 ) ) ;
#7121 = CARTESIAN_POINT ( 'NONE',  ( 47.13608539959999888, -74.52720457959999578, -1.647993573179999949 ) ) ;
#7122 = VERTEX_POINT ( 'NONE', #2107 ) ;
#7123 = ADVANCED_FACE ( 'NONE', ( #10942 ), #6440, .F. ) ;
#7124 = AXIS2_PLACEMENT_3D ( 'NONE', #25338, #436, #9430 ) ;
#7125 = DIRECTION ( 'NONE',  ( 0.000000000000000000, 1.000000000000000000, 0.000000000000000000 ) ) ;
#7126 = DIRECTION ( 'NONE',  ( 0.4794255386042041156, 0.000000000000000000, 0.8775825618903722036 ) ) ;
#7127 = CARTESIAN_POINT ( 'NONE',  ( 0.000000000000000000, -91.50000000000000000, 0.000000000000000000 ) ) ;
#7128 = EDGE_LOOP ( 'NONE', ( #8787, #8572, #12185, #4360, #23389, #1730 ) ) ;
#7129 = EDGE_CURVE ( 'NONE', #15684, #22913, #12262, .T. ) ;
#7130 = CARTESIAN_POINT ( 'NONE',  ( 36.34782515470000419, -74.05802478990000282, -14.27927808980000002 ) ) ;
#7131 = CARTESIAN_POINT ( 'NONE',  ( -16.87609683389999660, -99.97540119910000556, 3.286633550649999957 ) ) ;
#7132 = DIRECTION ( 'NONE',  ( 0.000000000000000000, 1.000000000000000000, 0.000000000000000000 ) ) ;
#7133 = CARTESIAN_POINT ( 'NONE',  ( -21.96310081540000070, -74.00000000000000000, -32.01947790320000564 ) ) ;
#7134 = ORIENTED_EDGE ( 'NONE', *, *, #7754, .T. ) ;
#7135 = CARTESIAN_POINT ( 'NONE',  ( -12.29363612059999866, -101.2530993000000024, -8.928690578620001261 ) ) ;
#7136 = DIRECTION ( 'NONE',  ( 1.000000000000000000, 0.000000000000000000, 0.000000000000000000 ) ) ;
#7137 = CARTESIAN_POINT ( 'NONE',  ( 0.1178905558060000108, -101.2358105800000061, -15.21680457949999976 ) ) ;
#7138 = CARTESIAN_POINT ( 'NONE',  ( -17.60583313680000472, -18.50000000000000000, 11.52657685249999986 ) ) ;
#7139 = VERTEX_POINT ( 'NONE', #5152 ) ;
#7140 = FACE_OUTER_BOUND ( 'NONE', #10514, .T. ) ;
#7141 = AXIS2_PLACEMENT_3D ( 'NONE', #23647, #10635, #19277 ) ;
#7142 = CARTESIAN_POINT ( 'NONE',  ( 23.58655530659999755, -94.70873790539999959, -2.249368515490000053 ) ) ;
#7143 = CARTESIAN_POINT ( 'NONE',  ( -38.55000000000000426, -65.14977478849999670, -2.857883832489999776 ) ) ;
#7144 = CARTESIAN_POINT ( 'NONE',  ( 15.62649610739214090, -101.5829753080984972, 3.664801835284849485 ) ) ;
#7145 = DIRECTION ( 'NONE',  ( -0.000000000000000000, 1.000000000000000000, 0.000000000000000000 ) ) ;
#7146 = ORIENTED_EDGE ( 'NONE', *, *, #4159, .T. ) ;
#7147 = CARTESIAN_POINT ( 'NONE',  ( 46.43423234700000535, -80.49808279690000745, -3.486565683130000259 ) ) ;
#7148 = CARTESIAN_POINT ( 'NONE',  ( -11.65446625000000047, -63.14742133130000923, -22.75868051570000006 ) ) ;
#7149 = AXIS2_PLACEMENT_3D ( 'NONE', #8239, #23835, #18913 ) ;
#7150 = TOROIDAL_SURFACE ( 'NONE', #23429, 2.500000000000000000, 0.5000000000000000000 ) ;
#7151 = CARTESIAN_POINT ( 'NONE',  ( 25.21073747289999645, -68.18737760160000505, -8.386242643919999296 ) ) ;
#7152 = CARTESIAN_POINT ( 'NONE',  ( 8.576875435287405480, -93.15740241113648779, 27.32333530169154301 ) ) ;
#7153 = ORIENTED_EDGE ( 'NONE', *, *, #10145, .F. ) ;
#7154 = CARTESIAN_POINT ( 'NONE',  ( -11.91166822033579464, -71.21053272331209882, -26.23707332927977021 ) ) ;
#7155 = ORIENTED_EDGE ( 'NONE', *, *, #6545, .T. ) ;
#7156 = CARTESIAN_POINT ( 'NONE',  ( 28.57122076013681422, -72.72581502554379540, 1.952398001462756216 ) ) ;
#7157 = LINE ( 'NONE', #20555, #26056 ) ;
#7158 = ORIENTED_EDGE ( 'NONE', *, *, #2789, .T. ) ;
#7159 = CARTESIAN_POINT ( 'NONE',  ( 31.00000000000000000, -11.00000000000000000, 4.500000000000000000 ) ) ;
#7160 = EDGE_CURVE ( 'NONE', #17027, #14123, #8789, .T. ) ;
#7161 = EDGE_CURVE ( 'NONE', #5109, #914, #16065, .T. ) ;
#7162 = AXIS2_PLACEMENT_3D ( 'NONE', #10622, #26257, #9727 ) ;
#7163 = CARTESIAN_POINT ( 'NONE',  ( 1.472192074426218689, -93.00000237470425191, -29.94733696998120820 ) ) ;
#7164 = CARTESIAN_POINT ( 'NONE',  ( -16.49390888960000368, -74.50000000000000000, 44.28897684009999836 ) ) ;
#7165 = CARTESIAN_POINT ( 'NONE',  ( -19.50386435929999962, -96.83699978299999600, 8.450360047540000252 ) ) ;
#7166 = CARTESIAN_POINT ( 'NONE',  ( -10.55247273420000020, -18.86819686409999974, -21.60718219059999967 ) ) ;
#7167 = CARTESIAN_POINT ( 'NONE',  ( 21.64462882888506812, -37.86826266693650211, -8.165772047040821491 ) ) ;
#7168 = ORIENTED_EDGE ( 'NONE', *, *, #7993, .T. ) ;
#7169 = DIRECTION ( 'NONE',  ( 1.000000000000000000, 0.000000000000000000, 0.000000000000000000 ) ) ;
#7170 = CARTESIAN_POINT ( 'NONE',  ( -38.00285745627953560, -65.72850285332773979, -0.9288085058657069570 ) ) ;
#7171 = CARTESIAN_POINT ( 'NONE',  ( -13.34145344800987942, -92.96960399592896351, 27.42727875496046508 ) ) ;
#7172 = ORIENTED_EDGE ( 'NONE', *, *, #22557, .T. ) ;
#7173 = EDGE_CURVE ( 'NONE', #6525, #16196, #14034, .T. ) ;
#7174 = AXIS2_PLACEMENT_3D ( 'NONE', #5946, #26211, #28108 ) ;
#7175 = CARTESIAN_POINT ( 'NONE',  ( 20.63161943080000071, -19.46510050319999863, -7.734358783100000245 ) ) ;
#7176 = CARTESIAN_POINT ( 'NONE',  ( 29.17304402409999753, -40.00000000000000000, 53.40089889099999709 ) ) ;
#7177 = DIRECTION ( 'NONE',  ( -0.3390050494208429743, 0.7071067811866730279, -0.6205445805637129775 ) ) ;
#7178 = ORIENTED_EDGE ( 'NONE', *, *, #20752, .T. ) ;
#7179 = CARTESIAN_POINT ( 'NONE',  ( -18.26050467580000003, -97.41004717059999507, 11.26842931770000078 ) ) ;
#7180 = CARTESIAN_POINT ( 'NONE',  ( -19.57536200539999882, -26.03958238319999907, 14.34081999809999886 ) ) ;
#7181 = CARTESIAN_POINT ( 'NONE',  ( 43.75000000000000000, -84.50000000000000000, 5.357814579270000097E-15 ) ) ;
#7182 = CARTESIAN_POINT ( 'NONE',  ( 31.15598256050000003, -72.92631784149999419, -20.30650074509999925 ) ) ;
#7183 = CARTESIAN_POINT ( 'NONE',  ( -14.68358879805363060, -74.18174932740166128, 36.27808831497246445 ) ) ;
#7184 = AXIS2_PLACEMENT_3D ( 'NONE', #3379, #8285, #28671 ) ;
#7185 = EDGE_CURVE ( 'NONE', #7833, #22866, #27400, .T. ) ;
#7186 =( LENGTH_UNIT ( ) NAMED_UNIT ( * ) SI_UNIT ( .MILLI., .METRE. ) );
#7187 = AXIS2_PLACEMENT_3D ( 'NONE', #13302, #20011, #8931 ) ;
#7188 = EDGE_LOOP ( 'NONE', ( #2172, #12058, #2808, #26898 ) ) ;
#7189 = DIRECTION ( 'NONE',  ( 0.000000000000000000, 1.000000000000000000, 0.000000000000000000 ) ) ;
#7190 = CARTESIAN_POINT ( 'NONE',  ( 12.40657046930000007, -98.24905629650000094, 14.77807252610000077 ) ) ;
#7191 = ORIENTED_EDGE ( 'NONE', *, *, #18544, .F. ) ;
#7192 = COLOUR_RGB ( '', 0.08235294, 0.09019608, 0.10196078) ;
#7193 = CARTESIAN_POINT ( 'NONE',  ( 7.250133233359999707, -73.75841684550000821, 39.12193274490000050 ) ) ;
#7194 = CARTESIAN_POINT ( 'NONE',  ( 46.63086251900000434, -74.05159139319999895, -3.730496185299999823 ) ) ;
#7195 = CARTESIAN_POINT ( 'NONE',  ( 23.52750467767722142, -19.48498740571179866, 1.429708917240688937 ) ) ;
#7196 = CARTESIAN_POINT ( 'NONE',  ( 26.98670340789999855, -72.82938977469999031, -9.720255250690000182 ) ) ;
#7197 = CARTESIAN_POINT ( 'NONE',  ( 0.3872056760440000245, -99.92967571559999840, -17.35614698070000017 ) ) ;
#7198 = CARTESIAN_POINT ( 'NONE',  ( 8.201563467870000679, -37.53730314839999949, -21.64399269869999642 ) ) ;
#7199 = CARTESIAN_POINT ( 'NONE',  ( 8.697618611485006923, -19.48148083423015109, -19.87404037427484838 ) ) ;
#7200 = ORIENTED_EDGE ( 'NONE', *, *, #27497, .T. ) ;
#7201 = CARTESIAN_POINT ( 'NONE',  ( 8.377755539869999879, -98.98742664769999067, 16.24331995230000203 ) ) ;
#7202 = DIRECTION ( 'NONE',  ( 0.9704142011833034598, 0.000000000000000000, 0.2414462220490750932 ) ) ;
#7203 = CARTESIAN_POINT ( 'NONE',  ( 21.53806854011714478, -36.56992522606418561, -6.948750312138934682 ) ) ;
#7204 = CARTESIAN_POINT ( 'NONE',  ( -1.681229913738337967, -19.46756325247292807, -22.31722361663701903 ) ) ;
#7205 = CARTESIAN_POINT ( 'NONE',  ( -14.85886005390000086, -100.9728335899999934, 4.751291413199999702 ) ) ;
#7206 = CARTESIAN_POINT ( 'NONE',  ( -19.92984078955770499, -18.50000000000000000, 15.63765909864717152 ) ) ;
#7207 = CARTESIAN_POINT ( 'NONE',  ( 12.69276409558878882, -96.42123289902950489, 17.27298930703739543 ) ) ;
#7208 = CARTESIAN_POINT ( 'NONE',  ( -37.93569409864744557, -65.70894154424837552, 0.8597713696862059329 ) ) ;
#7209 = CARTESIAN_POINT ( 'NONE',  ( 21.72762743471350788, -37.33446486334822367, -8.509936560388821292 ) ) ;
#7210 = CIRCLE ( 'NONE', #3922, 0.4999999999999997224 ) ;
#7211 = CARTESIAN_POINT ( 'NONE',  ( 24.63826343349942505, -93.08384138313128631, -15.50111966657502371 ) ) ;
#7212 = DIRECTION ( 'NONE',  ( 0.4794255386042036715, 0.000000000000000000, 0.8775825618903723147 ) ) ;
#7213 = ORIENTED_EDGE ( 'NONE', *, *, #3002, .T. ) ;
#7214 = CARTESIAN_POINT ( 'NONE',  ( 0.000000000000000000, -101.6484611540000031, 0.000000000000000000 ) ) ;
#7215 = EDGE_CURVE ( 'NONE', #3837, #19973, #23428, .T. ) ;
#7216 = CARTESIAN_POINT ( 'NONE',  ( -20.20541094980000096, -94.98812148390000232, 12.40015412250000004 ) ) ;
#7217 = AXIS2_PLACEMENT_3D ( 'NONE', #24584, #18173, #4917 ) ;
#7218 = CARTESIAN_POINT ( 'NONE',  ( 7.685241111800000802, -101.1376244509999935, 13.75999003799999976 ) ) ;
#7219 = ADVANCED_FACE ( 'NONE', ( #20448 ), #6351, .T. ) ;
#7220 = FACE_OUTER_BOUND ( 'NONE', #28537, .T. ) ;
#7221 = CARTESIAN_POINT ( 'NONE',  ( 20.52569424150000188, -35.38531346950000511, -8.770435587459999738 ) ) ;
#7222 = DIRECTION ( 'NONE',  ( 0.4794255386042040601, 0.000000000000000000, 0.8775825618903720926 ) ) ;
#7223 = AXIS2_PLACEMENT_3D ( 'NONE', #5726, #1372, #23514 ) ;
#7224 = EDGE_CURVE ( 'NONE', #12473, #21862, #959, .T. ) ;
#7225 = CARTESIAN_POINT ( 'NONE',  ( -0.5335602090290000321, -52.63293862049999916, -23.18581005440000098 ) ) ;
#7226 = DIRECTION ( 'NONE',  ( 1.000000000000000000, 0.000000000000000000, 0.000000000000000000 ) ) ;
#7227 = EDGE_CURVE ( 'NONE', #24310, #12443, #14797, .T. ) ;
#7228 = CARTESIAN_POINT ( 'NONE',  ( -14.62558108616616614, -93.99439547214892343, -21.62054592744825854 ) ) ;
#7229 = CARTESIAN_POINT ( 'NONE',  ( 16.81253980019999972, -99.88067631459999518, 4.253150432089999988 ) ) ;
#7230 = ORIENTED_EDGE ( 'NONE', *, *, #3758, .T. ) ;
#7231 = CARTESIAN_POINT ( 'NONE',  ( 0.000000000000000000, -11.55246854740000018, 0.000000000000000000 ) ) ;
#7232 = CARTESIAN_POINT ( 'NONE',  ( -24.00582602940000143, -94.71481430550001335, -4.132763454370000034 ) ) ;
#7233 = ORIENTED_EDGE ( 'NONE', *, *, #4873, .F. ) ;
#7234 = CARTESIAN_POINT ( 'NONE',  ( 8.504167659047778827, -92.65976904079447252, 29.29043331537584649 ) ) ;
#7235 = LINE ( 'NONE', #20484, #6236 ) ;
#7236 = CARTESIAN_POINT ( 'NONE',  ( 0.000000000000000000, -102.5000000000000000, 0.000000000000000000 ) ) ;
#7237 = CIRCLE ( 'NONE', #7704, 0.5000000000000004441 ) ;
#7238 = DIRECTION ( 'NONE',  ( 0.4794255386042033384, 0.000000000000000000, 0.8775825618903726477 ) ) ;
#7239 = CARTESIAN_POINT ( 'NONE',  ( -7.224488193841309247, -74.42768721721228076, -40.61475266807387641 ) ) ;
#7240 = CARTESIAN_POINT ( 'NONE',  ( -14.02382502650000085, -74.01102208230000201, 36.34092783020000184 ) ) ;
#7241 = CARTESIAN_POINT ( 'NONE',  ( 11.12357766309999896, -72.43053616469998701, -26.80850844170000258 ) ) ;
#7242 = B_SPLINE_CURVE_WITH_KNOTS ( 'NONE', 5,
 ( #22356, #17983, #2116, #10951, #19861, #2400 ),
 .UNSPECIFIED., .F., .F.,
 ( 6, 6 ),
 ( -66.18347591719999912, -36.59856967589999499 ),
 .UNSPECIFIED. ) ;
#7243 = CARTESIAN_POINT ( 'NONE',  ( -17.03345617734097317, -97.65592479666719328, 10.17337226560459307 ) ) ;
#7244 = ORIENTED_EDGE ( 'NONE', *, *, #25921, .F. ) ;
#7245 = CARTESIAN_POINT ( 'NONE',  ( 4.500000000000000000, -15.00000000000000000, -40.50000000000000000 ) ) ;
#7246 = CARTESIAN_POINT ( 'NONE',  ( 8.521725336259999395, -22.48306963330000130, -20.31493383569999978 ) ) ;
#7247 = CARTESIAN_POINT ( 'NONE',  ( -13.13284500319999992, -100.0994409990000094, -11.14317245900000053 ) ) ;
#7248 = CARTESIAN_POINT ( 'NONE',  ( -41.45000000000000284, -63.07912966450000880, 2.857883832489999776 ) ) ;
#7249 = CARTESIAN_POINT ( 'NONE',  ( 7.188502612221723709, -73.76099270142834996, -38.70686962976383683 ) ) ;
#7250 = EDGE_LOOP ( 'NONE', ( #11774, #9101, #28431, #26460 ) ) ;
#7251 = CARTESIAN_POINT ( 'NONE',  ( 27.19598314615092249, -92.50000000000001421, -13.80718576071233450 ) ) ;
#7252 = ORIENTED_EDGE ( 'NONE', *, *, #26009, .F. ) ;
#7253 = EDGE_CURVE ( 'NONE', #10170, #28264, #18554, .T. ) ;
#7254 = EDGE_CURVE ( 'NONE', #5383, #7122, #17136, .T. ) ;
#7255 = CIRCLE ( 'NONE', #26313, 3.500000000000003109 ) ;
#7256 = FACE_OUTER_BOUND ( 'NONE', #3102, .T. ) ;
#7257 = EDGE_CURVE ( 'NONE', #13019, #4784, #1356, .T. ) ;
#7258 = CARTESIAN_POINT ( 'NONE',  ( -5.029458127119999844, -99.62155223700000306, 16.98269931899999818 ) ) ;
#7259 = CARTESIAN_POINT ( 'NONE',  ( 4.039384380619999604, -93.70847541930001512, 26.05804507789999747 ) ) ;
#7260 = ADVANCED_FACE ( 'NONE', ( #9935 ), #812, .F. ) ;
#7261 = EDGE_LOOP ( 'NONE', ( #3084, #13307, #23431, #20726, #7023 ) ) ;
#7262 = CARTESIAN_POINT ( 'NONE',  ( -25.64971708790767835, -94.16483583517798195, -2.508592371179793279 ) ) ;
#7263 = CARTESIAN_POINT ( 'NONE',  ( -21.97687417839999569, -92.51331408429999215, -19.45668579410000376 ) ) ;
#7264 = CARTESIAN_POINT ( 'NONE',  ( 46.85181496819999580, -74.07956791590001444, -2.486435421679999980 ) ) ;
#7265 = ORIENTED_EDGE ( 'NONE', *, *, #14844, .F. ) ;
#7266 = CARTESIAN_POINT ( 'NONE',  ( 7.249694362036529505, -73.91587151478432816, -39.90536558169799974 ) ) ;
#7267 = PLANE ( 'NONE',  #22499 ) ;
#7268 = CARTESIAN_POINT ( 'NONE',  ( -6.754619094799999779, -97.17811284689999241, -19.41490638410000003 ) ) ;
#7269 = CARTESIAN_POINT ( 'NONE',  ( -2.969720195599999890, -65.80499425489999510, -26.85431770659999984 ) ) ;
#7270 = CARTESIAN_POINT ( 'NONE',  ( -14.67079327179999915, -67.87586646439999072, 22.52608794949999904 ) ) ;
#7271 = ORIENTED_EDGE ( 'NONE', *, *, #8341, .T. ) ;
#7272 = DIRECTION ( 'NONE',  ( 0.9952295494196654602, 0.000000000000000000, -0.09756097560976760563 ) ) ;
#7273 = PLANE ( 'NONE',  #22049 ) ;
#7274 = CARTESIAN_POINT ( 'NONE',  ( 26.23106671699999737, -64.35840483370000698, 1.472051099300000221 ) ) ;
#7275 = LINE ( 'NONE', #16142, #26446 ) ;
#7276 = ORIENTED_EDGE ( 'NONE', *, *, #2963, .T. ) ;
#7277 = CARTESIAN_POINT ( 'NONE',  ( -0.5256381167571819724, -45.99935878244429688, -22.95428131896234092 ) ) ;
#7278 = FACE_OUTER_BOUND ( 'NONE', #22734, .T. ) ;
#7279 = CARTESIAN_POINT ( 'NONE',  ( 36.62847051954670263, -74.18064277860715094, -14.32357927737881553 ) ) ;
#7280 = ORIENTED_EDGE ( 'NONE', *, *, #4882, .T. ) ;
#7281 = FACE_OUTER_BOUND ( 'NONE', #9210, .T. ) ;
#7282 = CARTESIAN_POINT ( 'NONE',  ( 21.33526310999999964, -62.97603269449999885, 11.59349340770000047 ) ) ;
#7283 = CARTESIAN_POINT ( 'NONE',  ( 8.988996102879999839, -34.66800400750000222, -19.43643858049999906 ) ) ;
#7284 = DIRECTION ( 'NONE',  ( -0.5012776526529407750, 0.000000000000000000, -0.8652864929898985702 ) ) ;
#7285 = DIRECTION ( 'NONE',  ( 0.8775825618903722036, 0.000000000000000000, -0.4794255386042041156 ) ) ;
#7286 = ORIENTED_EDGE ( 'NONE', *, *, #17324, .T. ) ;
#7287 = CARTESIAN_POINT ( 'NONE',  ( 45.89652018349999452, -80.18584073460000639, -4.323400012419999605 ) ) ;
#7288 = ADVANCED_FACE ( 'NONE', ( #28008 ), #10343, .T. ) ;
#7289 = PRODUCT_CONTEXT ( 'NONE', #5873, 'mechanical' ) ;
#7290 = CARTESIAN_POINT ( 'NONE',  ( -12.21854180399999912, -18.61865655080000082, 18.67250271059999989 ) ) ;
#7291 = CARTESIAN_POINT ( 'NONE',  ( -12.69354674090000046, -63.63799337809999912, -20.95011387349999765 ) ) ;
#7292 = CARTESIAN_POINT ( 'NONE',  ( 26.22359489970000013, -71.21989987509999764, -9.687831617969999698 ) ) ;
#7293 = CARTESIAN_POINT ( 'NONE',  ( 12.80450217360000131, -93.00000000000000000, 27.55316291459999789 ) ) ;
#7294 = ADVANCED_FACE ( 'NONE', ( #21722 ), #14998, .T. ) ;
#7295 = ORIENTED_EDGE ( 'NONE', *, *, #1602, .T. ) ;
#7296 = LINE ( 'NONE', #12219, #20544 ) ;
#7297 = CARTESIAN_POINT ( 'NONE',  ( 23.05498405910000059, -94.52419709919999491, -6.735184622040000235 ) ) ;
#7298 = ORIENTED_EDGE ( 'NONE', *, *, #13312, .F. ) ;
#7299 = CARTESIAN_POINT ( 'NONE',  ( 26.02259374959999860, -93.00000000000000000, -15.90831903569999994 ) ) ;
#7300 = CARTESIAN_POINT ( 'NONE',  ( -14.79537251110000007, -100.9197086940000077, 5.022279785309999411 ) ) ;
#7301 = VERTEX_POINT ( 'NONE', #6273 ) ;
#7302 = DIRECTION ( 'NONE',  ( 0.000000000000000000, -1.000000000000000000, 0.000000000000000000 ) ) ;
#7303 = CARTESIAN_POINT ( 'NONE',  ( 21.30133042140352373, -35.02996653984773445, -7.508028375805006149 ) ) ;
#7304 = ORIENTED_EDGE ( 'NONE', *, *, #26378, .F. ) ;
#7305 = CARTESIAN_POINT ( 'NONE',  ( 23.08854236903368218, -49.87586154376155179, -0.5737623537064138191 ) ) ;
#7306 = CARTESIAN_POINT ( 'NONE',  ( 23.05498378868082909, -94.52419745020957009, -6.735183927839049289 ) ) ;
#7307 = CARTESIAN_POINT ( 'NONE',  ( 0.000000000000000000, -24.50000000000000000, 0.000000000000000000 ) ) ;
#7308 = CARTESIAN_POINT ( 'NONE',  ( 9.617235035043430358, -59.75166407288456583, -23.68427203224058530 ) ) ;
#7309 = ORIENTED_EDGE ( 'NONE', *, *, #6892, .T. ) ;
#7310 = CARTESIAN_POINT ( 'NONE',  ( 0.000000000000000000, -89.00000000000000000, 0.000000000000000000 ) ) ;
#7311 = CARTESIAN_POINT ( 'NONE',  ( -20.76808354211960150, -63.08717869840388204, 12.74414642584173407 ) ) ;
#7312 = CARTESIAN_POINT ( 'NONE',  ( 14.89070032189999893, -101.0875971110000080, 3.963397078339999879 ) ) ;
#7313 = EDGE_LOOP ( 'NONE', ( #5373, #6644, #8345, #22424, #14308 ) ) ;
#7314 = CARTESIAN_POINT ( 'NONE',  ( 20.51869861192218281, -18.95847997710646027, -7.692027150944580782 ) ) ;
#7315 = CARTESIAN_POINT ( 'NONE',  ( 0.000000000000000000, -25.10000000000000142, 0.000000000000000000 ) ) ;
#7316 = DIRECTION ( 'NONE',  ( 1.000000000000000000, 0.000000000000000000, 0.000000000000000000 ) ) ;
#7317 = EDGE_LOOP ( 'NONE', ( #785, #13622, #14146, #18675 ) ) ;
#7318 = CARTESIAN_POINT ( 'NONE',  ( -18.21762735589999949, -97.23113437169998008, 11.17752812540000029 ) ) ;
#7319 = B_SPLINE_CURVE_WITH_KNOTS ( 'NONE', 5,
 ( #602, #154, #18052, #20380, #9594, #13820, #20532, #308, #16146, #7137, #25051, #16004 ),
 .UNSPECIFIED., .F., .F.,
 ( 6, 3, 3, 6 ),
 ( 0.000000000000000000, 0.4964111757615225495, 0.7833083924343531290, 1.000000000000000000 ),
 .UNSPECIFIED. ) ;
#7320 = CARTESIAN_POINT ( 'NONE',  ( 0.8950076880280000147, -99.72202992580000114, -17.14962640039999897 ) ) ;
#7321 = DIRECTION ( 'NONE',  ( -0.7071067811865474617, 0.000000000000000000, -0.7071067811865474617 ) ) ;
#7322 = EDGE_CURVE ( 'NONE', #17051, #16242, #18107, .T. ) ;
#7323 = DIRECTION ( 'NONE',  ( 0.000000000000000000, -1.000000000000000000, 0.000000000000000000 ) ) ;
#7324 = EDGE_CURVE ( 'NONE', #7420, #17308, #22281, .T. ) ;
#7325 = EDGE_CURVE ( 'NONE', #2162, #12777, #12955, .T. ) ;
#7326 = B_SPLINE_CURVE_WITH_KNOTS ( 'NONE', 3,
 ( #26580, #17408, #2401, #24100, #11259, #19724 ),
 .UNSPECIFIED., .F., .F.,
 ( 4, 2, 4 ),
 ( 0.000000000000000000, 0.5000000000000000000, 1.000000000000000000 ),
 .UNSPECIFIED. ) ;
#7327 = CARTESIAN_POINT ( 'NONE',  ( 27.29208946090000154, -66.82248673960000929, 1.826414992130000137 ) ) ;
#7328 = CARTESIAN_POINT ( 'NONE',  ( -10.72007167189999777, -18.61782383720000311, 18.81070191750000120 ) ) ;
#7329 = EDGE_CURVE ( 'NONE', #18068, #8093, #17848, .T. ) ;
#7330 = VERTEX_POINT ( 'NONE', #23912 ) ;
#7331 = CARTESIAN_POINT ( 'NONE',  ( -19.35716652280000005, -18.50000000000000000, 15.34467299940000018 ) ) ;
#7332 = DIRECTION ( 'NONE',  ( 0.000000000000000000, 1.000000000000000000, 0.000000000000000000 ) ) ;
#7333 = EDGE_LOOP ( 'NONE', ( #20871, #10302, #24906, #9615 ) ) ;
#7334 = CARTESIAN_POINT ( 'NONE',  ( 23.31078553111326457, -92.52640451556820267, -19.66869558794967432 ) ) ;
#7335 = CARTESIAN_POINT ( 'NONE',  ( 7.509443212019999869, -18.50000000000000000, -19.64862788269999783 ) ) ;
#7336 = B_SPLINE_SURFACE_WITH_KNOTS ( 'NONE', 5, 5, ( 
 ( #13026, #17425, #28487, #21507, #19455, #1989 ),
 ( #14790, #1568, #10409, #15204, #21939, #24118 ),
 ( #13180, #4154, #10831, #28627, #28202, #8659 ),
 ( #1423, #8235, #15350, #14928, #10267, #6045 ),
 ( #19181, #5908, #23833, #3873, #21653, #5031 ),
 ( #548, #22089, #8804, #4891, #26900, #13472 ) ),
 .UNSPECIFIED., .F., .F., .F.,
 ( 6, 6 ),
 ( 6, 6 ),
 ( 7.598610046719999289, 9.882009902280000091 ),
 ( 0.000000000000000000, 0.3214525575110000477 ),
 .UNSPECIFIED. ) ;
#7337 = FACE_OUTER_BOUND ( 'NONE', #28473, .T. ) ;
#7338 = CARTESIAN_POINT ( 'NONE',  ( -8.157403593650000673, -100.1340845430000002, 14.50241216579999914 ) ) ;
#7339 = CARTESIAN_POINT ( 'NONE',  ( 6.136951313910000039, -92.68584525849999523, 28.88469321279999846 ) ) ;
#7340 = CARTESIAN_POINT ( 'NONE',  ( -11.42926189381041091, -93.65092297039508651, -23.40447979846856796 ) ) ;
#7341 = CARTESIAN_POINT ( 'NONE',  ( 9.235022047270001977, -35.95171755970000049, -20.04752849569999995 ) ) ;
#7342 = CARTESIAN_POINT ( 'NONE',  ( 46.25000000000000000, -74.00000000000000000, -4.582575694960000057 ) ) ;
#7343 = ORIENTED_EDGE ( 'NONE', *, *, #1377, .T. ) ;
#7344 = AXIS2_PLACEMENT_3D ( 'NONE', #27896, #5334, #2864 ) ;
#7345 = CARTESIAN_POINT ( 'NONE',  ( -40.30949744628526332, -74.19510049693010956, 7.243395527605200890 ) ) ;
#7346 = EDGE_CURVE ( 'NONE', #11658, #14280, #12673, .T. ) ;
#7347 = LINE ( 'NONE', #22502, #6077 ) ;
#7348 = CARTESIAN_POINT ( 'NONE',  ( -12.41213674656621890, -19.47453264959771246, 19.24115019510791669 ) ) ;
#7349 = CARTESIAN_POINT ( 'NONE',  ( -3.633275807539999569, -96.53848370299999715, -21.05217880330000213 ) ) ;
#7350 = ORIENTED_EDGE ( 'NONE', *, *, #20855, .T. ) ;
#7351 = CARTESIAN_POINT ( 'NONE',  ( -2.504890583376165658, -19.48260761093995086, -23.29076242136417108 ) ) ;
#7352 = CARTESIAN_POINT ( 'NONE',  ( 11.85649048139999984, -101.3399913430000083, -10.94058650880000094 ) ) ;
#7353 = CARTESIAN_POINT ( 'NONE',  ( -1.164060375740000097, -45.99732788909999925, -23.00302772650000094 ) ) ;
#7354 = CARTESIAN_POINT ( 'NONE',  ( 15.50203935347336248, -95.03667172802255436, 17.29208320189042425 ) ) ;
#7355 = CARTESIAN_POINT ( 'NONE',  ( -38.41638535914064079, -63.05597747387668761, -2.885209034396270411 ) ) ;
#7356 = AXIS2_PLACEMENT_3D ( 'NONE', #5833, #23604, #10046 ) ;
#7357 = DIRECTION ( 'NONE',  ( 0.000000000000000000, 1.000000000000000000, 0.000000000000000000 ) ) ;
#7358 = CARTESIAN_POINT ( 'NONE',  ( 21.71814693700000021, -44.93138464870000348, -7.554088719500000160 ) ) ;
#7359 = CARTESIAN_POINT ( 'NONE',  ( 13.86995119186533110, -98.07255187705551691, 15.06288721130092512 ) ) ;
#7360 = DIRECTION ( 'NONE',  ( 0.000000000000000000, 1.000000000000000000, 0.000000000000000000 ) ) ;
#7361 = ORIENTED_EDGE ( 'NONE', *, *, #9993, .F. ) ;
#7362 = ADVANCED_FACE ( 'NONE', ( #5983 ), #1642, .T. ) ;
#7363 = CARTESIAN_POINT ( 'NONE',  ( 6.879827010689999689, -101.5964542560000012, 14.49003032519999934 ) ) ;
#7364 = CARTESIAN_POINT ( 'NONE',  ( -17.91778080311958377, -92.49838891740266433, -23.83053502024295156 ) ) ;
#7365 = CIRCLE ( 'NONE', #5503, 55.50192378860000275 ) ;
#7366 = CARTESIAN_POINT ( 'NONE',  ( 22.54736958690000037, -95.60035679240000661, -0.4727289621530000319 ) ) ;
#7367 = CARTESIAN_POINT ( 'NONE',  ( 19.96643108339999984, -35.14332902089999777, -8.964388679729999865 ) ) ;
#7368 = CARTESIAN_POINT ( 'NONE',  ( 7.220129148630540783, -73.62781383915867650, 39.34253424956806100 ) ) ;
#7369 = CIRCLE ( 'NONE', #12904, 3.750000000000000000 ) ;
#7370 = CARTESIAN_POINT ( 'NONE',  ( 8.677144207910000517, -37.95796631070000160, -21.92880662259999980 ) ) ;
#7371 = CARTESIAN_POINT ( 'NONE',  ( 21.61812661869999985, -36.72157724490000419, -8.702650991499998767 ) ) ;
#7372 = LINE ( 'NONE', #3150, #6747 ) ;
#7373 = DIRECTION ( 'NONE',  ( 0.000000000000000000, 1.000000000000000000, 0.000000000000000000 ) ) ;
#7374 = ORIENTED_EDGE ( 'NONE', *, *, #8540, .T. ) ;
#7375 = CARTESIAN_POINT ( 'NONE',  ( -13.32816333360000094, -101.1889999979999999, -11.12411022969999941 ) ) ;
#7376 = AXIS2_PLACEMENT_3D ( 'NONE', #19099, #1340, #27987 ) ;
#7377 = DIRECTION ( 'NONE',  ( 0.000000000000000000, 1.000000000000000000, 0.000000000000000000 ) ) ;
#7378 = ORIENTED_EDGE ( 'NONE', *, *, #191, .F. ) ;
#7379 = CARTESIAN_POINT ( 'NONE',  ( -30.45126014524323566, -92.64884742710843568, 1.723988062537378241 ) ) ;
#7380 = VERTEX_POINT ( 'NONE', #12812 ) ;
#7381 = CARTESIAN_POINT ( 'NONE',  ( 0.5734641406102992667, -100.3041487037959882, -17.04849403054064183 ) ) ;
#7382 = EDGE_CURVE ( 'NONE', #23896, #2628, #23081, .T. ) ;
#7383 = CARTESIAN_POINT ( 'NONE',  ( -11.98370860700000051, -101.2530993010000060, -9.340542411159999503 ) ) ;
#7384 = EDGE_CURVE ( 'NONE', #13154, #11916, #15024, .T. ) ;
#7385 = B_SPLINE_CURVE_WITH_KNOTS ( 'NONE', 5,
 ( #26940, #13514, #2470, #22574, #11323, #440, #4792, #299, #6981 ),
 .UNSPECIFIED., .F., .F.,
 ( 6, 3, 6 ),
 ( 0.000000000000000000, 0.5000000000000000000, 1.000000000000000000 ),
 .UNSPECIFIED. ) ;
#7386 = CARTESIAN_POINT ( 'NONE',  ( -7.220129148633156468, -73.62781383918019174, -39.34253424959684509 ) ) ;
#7387 = VECTOR ( 'NONE', #13078, 1000.000000000000114 ) ;
#7388 = CARTESIAN_POINT ( 'NONE',  ( -14.93121066289999987, -74.50000000000000000, 36.29905574720000061 ) ) ;
#7389 = DIRECTION ( 'NONE',  ( 0.4794255386042036715, 0.000000000000000000, 0.8775825618903723147 ) ) ;
#7390 = CARTESIAN_POINT ( 'NONE',  ( 13.03263440049999922, -94.63960162979999780, -19.83860502579999974 ) ) ;
#7391 = VERTEX_POINT ( 'NONE', #15591 ) ;
#7392 = CIRCLE ( 'NONE', #24124, 3.000000000000000888 ) ;
#7393 = CARTESIAN_POINT ( 'NONE',  ( -12.05351144729999824, -70.58794772379999927, -25.57911838539999749 ) ) ;
#7394 = CARTESIAN_POINT ( 'NONE',  ( 8.982220866290001382, -19.48263932869999948, -19.39107707569999661 ) ) ;
#7395 = DIRECTION ( 'NONE',  ( 0.000000000000000000, 1.000000000000000000, 0.000000000000000000 ) ) ;
#7396 = EDGE_CURVE ( 'NONE', #28554, #22934, #16820, .T. ) ;
#7397 = DIRECTION ( 'NONE',  ( 1.000000000000000000, 0.000000000000000000, 0.000000000000000000 ) ) ;
#7398 = CARTESIAN_POINT ( 'NONE',  ( -39.12175830409999122, -73.75838856979999036, -7.250123850439999629 ) ) ;
#7399 = ORIENTED_EDGE ( 'NONE', *, *, #3414, .F. ) ;
#7400 = ORIENTED_EDGE ( 'NONE', *, *, #4334, .T. ) ;
#7401 = EDGE_LOOP ( 'NONE', ( #15209, #21676, #492, #14588 ) ) ;
#7402 = DIRECTION ( 'NONE',  ( 0.000000000000000000, 1.000000000000000000, 0.000000000000000000 ) ) ;
#7403 = CARTESIAN_POINT ( 'NONE',  ( -4.778856212590000041, -99.55619081999999764, 16.81624398279999966 ) ) ;
#7404 = CARTESIAN_POINT ( 'NONE',  ( 10.50533355230000154, -92.65222886450000317, 27.42001380359999985 ) ) ;
#7405 = ORIENTED_EDGE ( 'NONE', *, *, #9898, .T. ) ;
#7406 = AXIS2_PLACEMENT_3D ( 'NONE', #22240, #9116, #2441 ) ;
#7407 = AXIS2_PLACEMENT_3D ( 'NONE', #5225, #7416, #16435 ) ;
#7408 = AXIS2_PLACEMENT_3D ( 'NONE', #23388, #3295, #20927 ) ;
#7409 = CARTESIAN_POINT ( 'NONE',  ( -28.92399207428294972, -93.08384138316088752, 3.275884373694147200 ) ) ;
#7410 = CARTESIAN_POINT ( 'NONE',  ( 9.393614001710000494, -38.00000000000000000, -22.97877290430000130 ) ) ;
#7411 = CARTESIAN_POINT ( 'NONE',  ( 11.21184057910000043, -36.00000000000000000, -22.05994369109999909 ) ) ;
#7412 = VERTEX_POINT ( 'NONE', #11207 ) ;
#7413 = CARTESIAN_POINT ( 'NONE',  ( 7.216929735086898390, -73.61493928631104211, -39.30828467231233958 ) ) ;
#7414 = CARTESIAN_POINT ( 'NONE',  ( -11.76694263665041262, -63.20675823528085147, 21.38603125774777425 ) ) ;
#7415 = CARTESIAN_POINT ( 'NONE',  ( -4.724916302899999643, -98.37119197950001137, -18.40548062020000231 ) ) ;
#7416 = DIRECTION ( 'NONE',  ( -0.6147555381618261539, 7.777821624297800830E-17, 0.7887177114147772006 ) ) ;
#7417 = CARTESIAN_POINT ( 'NONE',  ( -2.606614045719999773, -69.52108470319998901, -27.18390150700000163 ) ) ;
#7418 = ADVANCED_FACE ( 'NONE', ( #13709 ), #4967, .F. ) ;
#7419 = CARTESIAN_POINT ( 'NONE',  ( -14.56435550020000136, -68.97522950350000315, 22.81609951000000081 ) ) ;
#7420 = VERTEX_POINT ( 'NONE', #20563 ) ;
#7421 = EDGE_CURVE ( 'NONE', #12917, #18911, #3264, .T. ) ;
#7422 = DIRECTION ( 'NONE',  ( 0.000000000000000000, 1.000000000000000000, 0.000000000000000000 ) ) ;
#7423 = CARTESIAN_POINT ( 'NONE',  ( -16.57647362440000194, -100.3252744939999985, 3.114049206399999825 ) ) ;
#7424 = CARTESIAN_POINT ( 'NONE',  ( 25.16979986939999847, -65.00127508749999095, 0.1507740601240000200 ) ) ;
#7425 = CARTESIAN_POINT ( 'NONE',  ( 19.49544348199999888, -35.50000000000000000, -8.986258402430001624 ) ) ;
#7426 = EDGE_LOOP ( 'NONE', ( #26743, #12938, #11192, #1031 ) ) ;
#7427 = AXIS2_PLACEMENT_3D ( 'NONE', #53, #15608, #13422 ) ;
#7428 = FACE_OUTER_BOUND ( 'NONE', #23993, .T. ) ;
#7429 = EDGE_CURVE ( 'NONE', #15559, #9997, #3232, .T. ) ;
#7430 = CARTESIAN_POINT ( 'NONE',  ( -7.405876894974190883, -73.99964090891569413, 39.17806186240734689 ) ) ;
#7431 = CARTESIAN_POINT ( 'NONE',  ( 36.74680559931929480, -74.42334987367621579, -14.56713157595660668 ) ) ;
#7432 = ORIENTED_EDGE ( 'NONE', *, *, #11997, .F. ) ;
#7433 = EDGE_CURVE ( 'NONE', #12945, #22875, #27419, .T. ) ;
#7434 = AXIS2_PLACEMENT_3D ( 'NONE', #20860, #2797, #13552 ) ;
#7435 = CIRCLE ( 'NONE', #27882, 2.999999999999998224 ) ;
#7436 = CARTESIAN_POINT ( 'NONE',  ( -9.503513001449999109, -93.67083441959999845, -23.28128293860000042 ) ) ;
#7437 = AXIS2_PLACEMENT_3D ( 'NONE', #18156, #6649, #15512 ) ;
#7438 = CIRCLE ( 'NONE', #12506, 23.79684788999999867 ) ;
#7439 = CARTESIAN_POINT ( 'NONE',  ( 21.71348175089999799, -64.04267428580000399, 11.73101879090000033 ) ) ;
#7440 = CARTESIAN_POINT ( 'NONE',  ( 8.965452453730000215, -34.82094141099999973, -19.92119506740000290 ) ) ;
#7441 = DIRECTION ( 'NONE',  ( 0.000000000000000000, 1.000000000000000000, 0.000000000000000000 ) ) ;
#7442 = CARTESIAN_POINT ( 'NONE',  ( 36.74383121569999844, -74.66666669110000498, -14.69280905019999928 ) ) ;
#7443 = VERTEX_POINT ( 'NONE', #9905 ) ;
#7444 = CARTESIAN_POINT ( 'NONE',  ( 47.15414012749999983, -79.55218225590000714, -1.873848225679999757 ) ) ;
#7445 = UNCERTAINTY_MEASURE_WITH_UNIT (LENGTH_MEASURE( 1.000000000000000082E-05 ), #6851, 'distance_accuracy_value', 'NONE');
#7446 = CONTEXT_DEPENDENT_SHAPE_REPRESENTATION ( #18367, #25727 ) ;
#7447 = CARTESIAN_POINT ( 'NONE',  ( -11.41034487649999996, -19.46528075099999811, 19.03911974529999895 ) ) ;
#7448 = CARTESIAN_POINT ( 'NONE',  ( -12.45267061699999900, -63.62177041899999352, -21.09031584749999766 ) ) ;
#7449 = B_SPLINE_CURVE_WITH_KNOTS ( 'NONE', 5,
 ( #1289, #10132, #19848, #8629, #17682, #19052, #7837, #25614, #10654 ),
 .UNSPECIFIED., .F., .F.,
 ( 6, 3, 6 ),
 ( 0.000000000000000000, 1.237573681320000007, 1.566718891449999873 ),
 .UNSPECIFIED. ) ;
#7450 = CARTESIAN_POINT ( 'NONE',  ( 37.09477810047854973, -79.93445530391007026, -14.10616743337098455 ) ) ;
#7451 = CARTESIAN_POINT ( 'NONE',  ( 25.33520104860000188, -65.80271452349998640, -10.35056844610000049 ) ) ;
#7452 = CARTESIAN_POINT ( 'NONE',  ( 3.624928909112701714, -94.04663295064030137, 25.74405677523981950 ) ) ;
#7453 = ORIENTED_EDGE ( 'NONE', *, *, #3942, .T. ) ;
#7454 = DIRECTION ( 'NONE',  ( 1.000000000000000000, 0.000000000000000000, 0.000000000000000000 ) ) ;
#7455 = ORIENTED_EDGE ( 'NONE', *, *, #8070, .T. ) ;
#7456 = CARTESIAN_POINT ( 'NONE',  ( -13.39932972679999956, -27.00850923819999849, 20.26025068540000262 ) ) ;
#7457 = CARTESIAN_POINT ( 'NONE',  ( -5.845306076740000023, -101.1045726949999874, 14.39333474509999888 ) ) ;
#7458 = EDGE_LOOP ( 'NONE', ( #17312, #21391, #23832, #6561 ) ) ;
#7459 = CARTESIAN_POINT ( 'NONE',  ( -37.75000000000000000, -63.30468293320000583, -0.7216878364849999006 ) ) ;
#7460 = CARTESIAN_POINT ( 'NONE',  ( 0.000000000000000000, -101.2530993010000060, 0.000000000000000000 ) ) ;
#7461 = CIRCLE ( 'NONE', #18618, 23.79684788999999867 ) ;
#7462 = ORIENTED_EDGE ( 'NONE', *, *, #4641, .T. ) ;
#7463 = CARTESIAN_POINT ( 'NONE',  ( 39.64169929330000031, -73.82505178019999903, 7.260629316899999353 ) ) ;
#7464 = CARTESIAN_POINT ( 'NONE',  ( -10.50201809968876354, -19.47159322330747599, -20.11218106846735765 ) ) ;
#7465 = CARTESIAN_POINT ( 'NONE',  ( 7.105427357599999217E-15, -74.50000000000000000, 3.552713678799999608E-15 ) ) ;
#7466 = CARTESIAN_POINT ( 'NONE',  ( -40.81117883860000006, -65.49083508809999898, -2.489060262989999828 ) ) ;
#7467 = CARTESIAN_POINT ( 'NONE',  ( 46.25000000000000000, -80.00000000000000000, -4.582575694960000057 ) ) ;
#7468 = ORIENTED_EDGE ( 'NONE', *, *, #25001, .F. ) ;
#7469 = EDGE_CURVE ( 'NONE', #8141, #2786, #9712, .T. ) ;
#7470 = CARTESIAN_POINT ( 'NONE',  ( 4.882943008269999509E-15, -74.50000000000000000, -40.00000000000000000 ) ) ;
#7471 = CARTESIAN_POINT ( 'NONE',  ( 18.32884736220000121, -98.65110728940000229, 3.454506764930000084 ) ) ;
#7472 = FACE_OUTER_BOUND ( 'NONE', #1599, .T. ) ;
#7473 = ORIENTED_EDGE ( 'NONE', *, *, #1529, .T. ) ;
#7474 = DIRECTION ( 'NONE',  ( 0.000000000000000000, -1.000000000000000000, 0.000000000000000000 ) ) ;
#7475 = DIRECTION ( 'NONE',  ( 0.000000000000000000, 1.000000000000000000, 0.000000000000000000 ) ) ;
#7476 = DIRECTION ( 'NONE',  ( 0.5000000000001886269, 0.000000000000000000, 0.8660254037843296837 ) ) ;
#7477 = ORIENTED_EDGE ( 'NONE', *, *, #8070, .F. ) ;
#7478 = EDGE_CURVE ( 'NONE', #27002, #16095, #10184, .T. ) ;
#7479 = CARTESIAN_POINT ( 'NONE',  ( -18.45777030029999821, -95.98445299990001445, 13.67729003380000030 ) ) ;
#7480 = CARTESIAN_POINT ( 'NONE',  ( 0.4578259502959999838, -99.78393592979999482, -17.31657152750000250 ) ) ;
#7481 = CARTESIAN_POINT ( 'NONE',  ( -16.54318588419999969, -91.50000000000000000, 25.62368046950000178 ) ) ;
#7482 = CARTESIAN_POINT ( 'NONE',  ( 27.75394116159999669, -74.50000000000000000, -27.75394116159999669 ) ) ;
#7483 = CARTESIAN_POINT ( 'NONE',  ( -14.87486851012731393, -74.34009834986436260, 36.29443389971319078 ) ) ;
#7484 = AXIS2_PLACEMENT_3D ( 'NONE', #16, #15417, #22444 ) ;
#7485 = TOROIDAL_SURFACE ( 'NONE', #11142, 7.750000000000000000, 0.5000000000000000000 ) ;
#7486 = ORIENTED_EDGE ( 'NONE', *, *, #19652, .T. ) ;
#7487 = CARTESIAN_POINT ( 'NONE',  ( 9.885503723209998483, -36.00000000000000000, -20.33566493420000043 ) ) ;
#7488 = FACE_BOUND ( 'NONE', #6490, .T. ) ;
#7489 = CARTESIAN_POINT ( 'NONE',  ( 20.76816312569999923, -36.14487676950000150, -8.994776261610001100 ) ) ;
#7490 = CARTESIAN_POINT ( 'NONE',  ( 8.188639545130001807, -100.9197082849999987, 13.30686044670000001 ) ) ;
#7491 = ORIENTED_EDGE ( 'NONE', *, *, #2333, .T. ) ;
#7492 = DIRECTION ( 'NONE',  ( 0.000000000000000000, -1.000000000000000000, 0.000000000000000000 ) ) ;
#7493 = DIRECTION ( 'NONE',  ( 0.4794255386042000078, 0.000000000000000000, 0.8775825618903743131 ) ) ;
#7494 = CARTESIAN_POINT ( 'NONE',  ( -20.89470113654807193, -64.89165741046112146, 14.23290170999320736 ) ) ;
#7495 = CARTESIAN_POINT ( 'NONE',  ( -8.092637767860001219, -100.1512121650000040, 14.53899152610000201 ) ) ;
#7496 =( LENGTH_UNIT ( ) NAMED_UNIT ( * ) SI_UNIT ( .MILLI., .METRE. ) );
#7497 = CARTESIAN_POINT ( 'NONE',  ( -20.45998242170000125, -45.73899999920000425, 14.78974999389999923 ) ) ;
#7498 = CIRCLE ( 'NONE', #23751, 0.4999999999999981126 ) ;
#7499 = CARTESIAN_POINT ( 'NONE',  ( 7.585614467160000096, -101.4252535300000062, 14.05241625360000057 ) ) ;
#7500 = VERTEX_POINT ( 'NONE', #27708 ) ;
#7501 = VECTOR ( 'NONE', #474, 1000.000000000000000 ) ;
#7502 = EDGE_CURVE ( 'NONE', #20928, #22701, #19476, .T. ) ;
#7503 = CARTESIAN_POINT ( 'NONE',  ( -43.24373363001436132, -65.12549727759811447, -0.1396600726280878280 ) ) ;
#7504 = AXIS2_PLACEMENT_3D ( 'NONE', #6996, #15859, #27103 ) ;
#7505 = CARTESIAN_POINT ( 'NONE',  ( 23.98359025029999714, -18.62222165789999906, 1.917870889060000028 ) ) ;
#7506 = DIRECTION ( 'NONE',  ( 0.2414462220490753985, 0.000000000000000000, 0.9704142011833032377 ) ) ;
#7507 = EDGE_LOOP ( 'NONE', ( #14256, #18616, #5360, #13627 ) ) ;
#7508 = CARTESIAN_POINT ( 'NONE',  ( -11.31667057079999950, -95.23931402160000914, -21.36056405359999744 ) ) ;
#7509 = CARTESIAN_POINT ( 'NONE',  ( 12.04737265750000041, -101.6484611540000031, -10.52904611299999971 ) ) ;
#7510 = CARTESIAN_POINT ( 'NONE',  ( -2.584367914690000045, -39.30675845289999870, -24.46232226030000234 ) ) ;
#7511 = CARTESIAN_POINT ( 'NONE',  ( -17.48265869433503639, -92.69183043860316218, 24.99229797076763049 ) ) ;
#7512 = EDGE_CURVE ( 'NONE', #12727, #5555, #5549, .T. ) ;
#7513 = DIRECTION ( 'NONE',  ( 0.8077658500622459936, 0.000000000000000000, -0.5895034617991798953 ) ) ;
#7514 = B_SPLINE_CURVE_WITH_KNOTS ( 'NONE', 5,
 ( #12061, #18792, #23158, #20690, #16147, #5237, #21118, #16296, #18928, #11777, #13970, #7848 ),
 .UNSPECIFIED., .F., .F.,
 ( 6, 3, 3, 6 ),
 ( -25.08217527269999891, -18.82032368775269759, -10.56887946808384804, -7.186327137960567768 ),
 .UNSPECIFIED. ) ;
#7515 = CARTESIAN_POINT ( 'NONE',  ( 11.93197532131579486, -101.6077248516953233, -10.70531747399618006 ) ) ;
#7516 = CARTESIAN_POINT ( 'NONE',  ( 21.79505839750000007, -40.73328259210000368, -8.465915579709999861 ) ) ;
#7517 = DIRECTION ( 'NONE',  ( 0.000000000000000000, -1.000000000000000000, 0.000000000000000000 ) ) ;
#7518 = FACE_OUTER_BOUND ( 'NONE', #10158, .T. ) ;
#7519 = ORIENTED_EDGE ( 'NONE', *, *, #3500, .T. ) ;
#7520 = CARTESIAN_POINT ( 'NONE',  ( 6.669404441700000241, -101.1848541609999899, 13.75051561090000085 ) ) ;
#7521 = CARTESIAN_POINT ( 'NONE',  ( -7.333297298759998917, -94.59276292389999696, -22.63874378639999563 ) ) ;
#7522 = B_SPLINE_CURVE_WITH_KNOTS ( 'NONE', 5,
 ( #22304, #2350, #182, #18227, #8728, #2650, #9031, #11501, #20409, #24198, #27124, #13105 ),
 .UNSPECIFIED., .F., .F.,
 ( 6, 3, 3, 6 ),
 ( -25.08217526769999850, -18.82032368487667640, -10.56887946683943547, -7.186327137019109301 ),
 .UNSPECIFIED. ) ;
#7523 = CARTESIAN_POINT ( 'NONE',  ( 7.743429286519999621, -101.6328744999999998, 14.01526831580000021 ) ) ;
#7524 = VECTOR ( 'NONE', #18174, 1000.000000000000000 ) ;
#7525 = CIRCLE ( 'NONE', #9821, 11.00000000000000000 ) ;
#7526 = CARTESIAN_POINT ( 'NONE',  ( 40.00000000000000000, -69.00000000000000000, 5.786765616290000531E-15 ) ) ;
#7527 = CARTESIAN_POINT ( 'NONE',  ( 21.21808932789999957, -34.59820509829999935, -7.670972970090000231 ) ) ;
#7528 = CARTESIAN_POINT ( 'NONE',  ( 23.29172356445612024, -59.74599976188999761, 10.44929617870533534 ) ) ;
#7529 = CIRCLE ( 'NONE', #14918, 55.50192378860000275 ) ;
#7530 = DIRECTION ( 'NONE',  ( 0.000000000000000000, 1.000000000000000000, 0.000000000000000000 ) ) ;
#7531 = CARTESIAN_POINT ( 'NONE',  ( 21.84310887519999866, -37.95394735069999825, -8.556787659450000305 ) ) ;
#7532 = CARTESIAN_POINT ( 'NONE',  ( -19.33030770744392868, -93.18010901131746948, -20.96669272993039357 ) ) ;
#7533 = LINE ( 'NONE', #20922, #9358 ) ;
#7534 = ORIENTED_EDGE ( 'NONE', *, *, #19822, .T. ) ;
#7535 = FILL_AREA_STYLE ('',( #18595 ) ) ;
#7536 = CARTESIAN_POINT ( 'NONE',  ( -19.58183770029999948, -93.00000000000000000, 20.70264511730000123 ) ) ;
#7537 = VERTEX_POINT ( 'NONE', #25507 ) ;
#7538 = CARTESIAN_POINT ( 'NONE',  ( 9.718892398710000435, -93.00000000000000000, 28.91008700340000104 ) ) ;
#7539 = VERTEX_POINT ( 'NONE', #5543 ) ;
#7540 = EDGE_CURVE ( 'NONE', #23975, #4037, #16762, .T. ) ;
#7541 = EDGE_CURVE ( 'NONE', #23580, #7650, #4574, .T. ) ;
#7542 = CARTESIAN_POINT ( 'NONE',  ( 0.5662235371520514260, -100.9570234915770897, -16.52900152527487876 ) ) ;
#7543 = CARTESIAN_POINT ( 'NONE',  ( 6.496108347790000792, -101.2358105800000061, 13.76101799030000095 ) ) ;
#7544 = CARTESIAN_POINT ( 'NONE',  ( -12.05063396398067965, -64.89165752751554805, -22.22490323539291524 ) ) ;
#7545 = AXIS2_PLACEMENT_3D ( 'NONE', #24391, #8777, #1818 ) ;
#7546 = CARTESIAN_POINT ( 'NONE',  ( -7.244162156032069255, -74.18137224046682832, -40.29089741864455476 ) ) ;
#7547 = AXIS2_PLACEMENT_3D ( 'NONE', #4511, #2340, #4662 ) ;
#7548 = AXIS2_PLACEMENT_3D ( 'NONE', #318, #26370, #9158 ) ;
#7549 = DIRECTION ( 'NONE',  ( 0.7071067811865474617, 0.000000000000000000, 0.7071067811865474617 ) ) ;
#7550 = CARTESIAN_POINT ( 'NONE',  ( 12.83908660400000024, -94.89196973819998959, -19.89638119809999850 ) ) ;
#7551 = ORIENTED_EDGE ( 'NONE', *, *, #13517, .T. ) ;
#7552 = CYLINDRICAL_SURFACE ( 'NONE', #17153, 10.00000000000000000 ) ;
#7553 = DIRECTION ( 'NONE',  ( 0.000000000000000000, 1.000000000000000000, 0.000000000000000000 ) ) ;
#7554 = CARTESIAN_POINT ( 'NONE',  ( -2.488381629358669134, -57.43018252028311821, -24.62423963244554059 ) ) ;
#7555 = CARTESIAN_POINT ( 'NONE',  ( 19.50599165336712915, -19.46426558497125470, 10.25100193001445170 ) ) ;
#7556 = ORIENTED_EDGE ( 'NONE', *, *, #19652, .F. ) ;
#7557 = ORIENTED_EDGE ( 'NONE', *, *, #14502, .T. ) ;
#7558 = EDGE_CURVE ( 'NONE', #21778, #4525, #1501, .T. ) ;
#7559 = CARTESIAN_POINT ( 'NONE',  ( -1.980680968570000200, -57.88555731719999642, -23.85230741780000230 ) ) ;
#7560 = EDGE_CURVE ( 'NONE', #2039, #11046, #13425, .T. ) ;
#7561 = DIRECTION ( 'NONE',  ( 6.106226635439999831E-16, 0.000000000000000000, 1.000000000000000000 ) ) ;
#7562 = AXIS2_PLACEMENT_3D ( 'NONE', #491, #4975, #15600 ) ;
#7563 = CARTESIAN_POINT ( 'NONE',  ( 8.025111386280000758, -92.67508346670000208, 27.00340670960000011 ) ) ;
#7564 = ORIENTED_EDGE ( 'NONE', *, *, #10088, .T. ) ;
#7565 = ORIENTED_EDGE ( 'NONE', *, *, #12031, .F. ) ;
#7566 = FACE_OUTER_BOUND ( 'NONE', #6284, .T. ) ;
#7567 = CARTESIAN_POINT ( 'NONE',  ( 21.94388422209999945, -37.05206035260000164, -9.022696796810000919 ) ) ;
#7568 = CARTESIAN_POINT ( 'NONE',  ( 47.25000000000000000, -75.00000000000000000, -13.75000000000000000 ) ) ;
#7569 = EDGE_LOOP ( 'NONE', ( #25031, #12256, #27068, #5519 ) ) ;
#7570 = CARTESIAN_POINT ( 'NONE',  ( 7.249551406111377716, -74.03750509262690116, -40.08893529128285138 ) ) ;
#7571 = CARTESIAN_POINT ( 'NONE',  ( -10.61287167059999881, -19.46510050329999686, 19.30934957549999709 ) ) ;
#7572 = VERTEX_POINT ( 'NONE', #8563 ) ;
#7573 = CARTESIAN_POINT ( 'NONE',  ( 21.70991749090000056, -40.75155002500000023, -6.890073352940000007 ) ) ;
#7574 = CARTESIAN_POINT ( 'NONE',  ( -2.647831762760000096, -64.47176800949999631, -25.90231288840000090 ) ) ;
#7575 = DIRECTION ( 'NONE',  ( 0.4151946956541399669, 0.5000000000001689759, 0.7600087925152558821 ) ) ;
#7576 = ORIENTED_EDGE ( 'NONE', *, *, #331, .F. ) ;
#7577 = CARTESIAN_POINT ( 'NONE',  ( 36.29989756469999662, -74.04896632250000721, -14.30540807509999901 ) ) ;
#7578 = CARTESIAN_POINT ( 'NONE',  ( -15.75068343869999765, -101.2375447300000104, 3.306461786589999896 ) ) ;
#7579 = CARTESIAN_POINT ( 'NONE',  ( 25.43931335289999751, -61.67863912290000172, 1.361017498729999886 ) ) ;
#7580 = CARTESIAN_POINT ( 'NONE',  ( 36.22844186549999534, -74.00000000000000000, -13.75000000000000000 ) ) ;
#7581 = ORIENTED_EDGE ( 'NONE', *, *, #429, .F. ) ;
#7582 = CARTESIAN_POINT ( 'NONE',  ( -0.5856137342820000313, -19.46510053389999939, -22.02591827759999887 ) ) ;
#7583 = AXIS2_PLACEMENT_3D ( 'NONE', #1621, #26075, #1750 ) ;
#7584 = CARTESIAN_POINT ( 'NONE',  ( -7.285364666873626938, -73.99996940651281818, 39.64792326107047415 ) ) ;
#7585 = CARTESIAN_POINT ( 'NONE',  ( 36.70128390686866737, -74.28717797990978511, -14.45333729646541698 ) ) ;
#7586 = ORIENTED_EDGE ( 'NONE', *, *, #20330, .F. ) ;
#7587 = CARTESIAN_POINT ( 'NONE',  ( -13.64864847579999996, -18.50000000000000000, 18.87892408420000123 ) ) ;
#7588 = CARTESIAN_POINT ( 'NONE',  ( -41.74285146984968975, -65.12158389260652314, -2.747462277523349705 ) ) ;
#7589 = CARTESIAN_POINT ( 'NONE',  ( -38.66568593819999933, -65.21397798589998729, -2.791092524920000262 ) ) ;
#7590 = CARTESIAN_POINT ( 'NONE',  ( 16.39558919584665730, -100.4211561361363181, 4.355600236979787709 ) ) ;
#7591 = FACE_OUTER_BOUND ( 'NONE', #22899, .T. ) ;
#7592 = ORIENTED_EDGE ( 'NONE', *, *, #3612, .T. ) ;
#7593 = B_SPLINE_SURFACE_WITH_KNOTS ( 'NONE', 5, 5, ( 
 ( #27018, #15923, #2547, #13892, #11694, #17832 ),
 ( #9370, #24527, #2244, #26728, #9518, #13296 ),
 ( #2395, #15772, #7060, #16069, #20606, #17977 ),
 ( #6909, #24683, #11398, #523, #18419, #7349 ),
 ( #15628, #24385, #22351, #24828, #18272, #26869 ),
 ( #11087, #4564, #20301, #13442, #4425, #2689 ) ),
 .UNSPECIFIED., .F., .F., .F.,
 ( 6, 6 ),
 ( 6, 6 ),
 ( 15.82768567739999988, 30.79603606530000093 ),
 ( 0.000000000000000000, 0.5000000000000000000 ),
 .UNSPECIFIED. ) ;
#7594 = CARTESIAN_POINT ( 'NONE',  ( 25.86648679569999842, -67.35799111629999913, -10.65566745589999975 ) ) ;
#7595 = CARTESIAN_POINT ( 'NONE',  ( 6.552802695180705683, -93.39297675734871973, 26.85969955741595783 ) ) ;
#7596 = EDGE_CURVE ( 'NONE', #12424, #21733, #10605, .T. ) ;
#7597 = VERTEX_POINT ( 'NONE', #21981 ) ;
#7598 = DIRECTION ( 'NONE',  ( 0.000000000000000000, 1.000000000000000000, 0.000000000000000000 ) ) ;
#7599 = DIRECTION ( 'NONE',  ( 0.000000000000000000, 1.000000000000000000, 0.000000000000000000 ) ) ;
#7600 = EDGE_LOOP ( 'NONE', ( #11237, #10210, #24794, #19867 ) ) ;
#7601 = TOROIDAL_SURFACE ( 'NONE', #20630, 29.91857981989999971, 10.00000000000000000 ) ;
#7602 = CARTESIAN_POINT ( 'NONE',  ( -12.95621714570000016, -27.03158182010000132, 19.72987597090000023 ) ) ;
#7603 = CARTESIAN_POINT ( 'NONE',  ( -5.873419970429999637, -101.3150705500000157, 15.15334666360000071 ) ) ;
#7604 = EDGE_CURVE ( 'NONE', #26673, #12661, #3915, .T. ) ;
#7605 = VERTEX_POINT ( 'NONE', #15104 ) ;
#7606 = CIRCLE ( 'NONE', #24308, 0.5000000000000027756 ) ;
#7607 = CARTESIAN_POINT ( 'NONE',  ( 6.483702463809999749E-15, -84.50000000000000000, -40.00000000000000000 ) ) ;
#7608 = EDGE_CURVE ( 'NONE', #9894, #7605, #21814, .T. ) ;
#7609 = CARTESIAN_POINT ( 'NONE',  ( 40.70731707320000226, -74.50000000000000000, 7.215414233289999757 ) ) ;
#7610 = CARTESIAN_POINT ( 'NONE',  ( -20.22328559685182370, -94.79580598126329960, 12.30740073859241157 ) ) ;
#7611 = CARTESIAN_POINT ( 'NONE',  ( -13.09202710664791880, -101.6077248516953091, -9.250658545580620284 ) ) ;
#7612 = CARTESIAN_POINT ( 'NONE',  ( 7.610177731959999470, -101.4231532209999926, 14.04048934709999941 ) ) ;
#7613 = CARTESIAN_POINT ( 'NONE',  ( 46.96553338548562095, -79.70204288960100314, -2.546098179092394886 ) ) ;
#7614 = ORIENTED_EDGE ( 'NONE', *, *, #13110, .T. ) ;
#7615 = CARTESIAN_POINT ( 'NONE',  ( 12.88056670439999962, -94.79581646409999962, -19.86310537439999990 ) ) ;
#7616 = CARTESIAN_POINT ( 'NONE',  ( 0.000000000000000000, -16.10310889129999623, 0.000000000000000000 ) ) ;
#7617 = DIRECTION ( 'NONE',  ( 0.09756097560976655092, 0.000000000000000000, -0.9952295494196655712 ) ) ;
#7618 = FACE_OUTER_BOUND ( 'NONE', #12692, .T. ) ;
#7619 = ORIENTED_EDGE ( 'NONE', *, *, #7841, .F. ) ;
#7620 = CONICAL_SURFACE ( 'NONE', #22016, 53.75557630319999447, 1.380808038880000144 ) ;
#7621 = CARTESIAN_POINT ( 'NONE',  ( -0.7490697104619999935, -79.69325168709998763, 47.25079635160000180 ) ) ;
#7622 = CARTESIAN_POINT ( 'NONE',  ( 22.35420140607709527, -19.18584080450712648, 9.881343207706809295 ) ) ;
#7623 = VERTEX_POINT ( 'NONE', #12916 ) ;
#7624 = DIRECTION ( 'NONE',  ( 1.000000000000000000, 0.000000000000000000, 0.000000000000000000 ) ) ;
#7625 = VECTOR ( 'NONE', #7834, 1000.000000000000000 ) ;
#7626 = CARTESIAN_POINT ( 'NONE',  ( -19.88518777170000007, -26.02764329579999725, 14.47991441779999988 ) ) ;
#7627 = CARTESIAN_POINT ( 'NONE',  ( 0.000000000000000000, -26.29689110869999880, 0.000000000000000000 ) ) ;
#7628 = CARTESIAN_POINT ( 'NONE',  ( -38.21231771845751268, -65.71847493511126004, 1.315734964525751671 ) ) ;
#7629 = CARTESIAN_POINT ( 'NONE',  ( 22.76484527320000240, -58.91972909429999561, -9.111819319440000342 ) ) ;
#7630 = CIRCLE ( 'NONE', #23871, 0.5000000000000004441 ) ;
#7631 = EDGE_CURVE ( 'NONE', #21711, #17492, #26831, .T. ) ;
#7632 = ORIENTED_EDGE ( 'NONE', *, *, #26451, .F. ) ;
#7633 = LINE ( 'NONE', #16350, #1207 ) ;
#7634 = CONICAL_SURFACE ( 'NONE', #2500, 21.99999999999999645, 0.03490658503990158590 ) ;
#7635 = CARTESIAN_POINT ( 'NONE',  ( 21.22368013470000037, -36.46178979729999980, -8.714942773269999776 ) ) ;
#7636 = VERTEX_POINT ( 'NONE', #2314 ) ;
#7637 = CARTESIAN_POINT ( 'NONE',  ( -38.51944941322620508, -63.07121106307049274, 2.875522221976945403 ) ) ;
#7638 = CARTESIAN_POINT ( 'NONE',  ( 47.19280574540000117, -74.66665734379999719, -1.149945984370000174 ) ) ;
#7639 = EDGE_CURVE ( 'NONE', #23549, #2616, #10117, .T. ) ;
#7640 = CARTESIAN_POINT ( 'NONE',  ( -18.05095942279999832, -92.84292204339999444, -23.30076308079999592 ) ) ;
#7641 = CYLINDRICAL_SURFACE ( 'NONE', #22692, 7.250000000000004441 ) ;
#7642 = CARTESIAN_POINT ( 'NONE',  ( 7.843434090700001526, -40.74566548840000024, -21.60733108830000049 ) ) ;
#7643 = TOROIDAL_SURFACE ( 'NONE', #5300, 7.000000000000000000, 1.000000000000000000 ) ;
#7644 = CARTESIAN_POINT ( 'NONE',  ( 7.614853083119999866, -101.6475450410000008, 14.07253421090000067 ) ) ;
#7645 = ORIENTED_EDGE ( 'NONE', *, *, #22086, .T. ) ;
#7646 = DIRECTION ( 'NONE',  ( 0.000000000000000000, 1.000000000000000000, 0.000000000000000000 ) ) ;
#7647 = DIRECTION ( 'NONE',  ( 1.000000000000000000, 0.000000000000000000, 0.000000000000000000 ) ) ;
#7648 = CARTESIAN_POINT ( 'NONE',  ( -13.39873670630472446, -19.49660132354000197, 20.21730935084874048 ) ) ;
#7649 = CARTESIAN_POINT ( 'NONE',  ( 11.89990227600000061, -99.62155223610000121, -13.11868328289999930 ) ) ;
#7650 = VERTEX_POINT ( 'NONE', #24454 ) ;
#7651 = CARTESIAN_POINT ( 'NONE',  ( 19.47999862770000234, -18.50000000000000000, -7.780772602109999880 ) ) ;
#7652 = CARTESIAN_POINT ( 'NONE',  ( 11.39953095620000134, -101.1130130960000031, -10.39219190439999885 ) ) ;
#7653 = CARTESIAN_POINT ( 'NONE',  ( 0.000000000000000000, -15.49681045920000066, 0.000000000000000000 ) ) ;
#7654 = CARTESIAN_POINT ( 'NONE',  ( -4.500000000000000000, -13.00000000000000000, 50.00000000000000000 ) ) ;
#7655 = AXIS2_PLACEMENT_3D ( 'NONE', #15560, #8425, #21991 ) ;
#7656 = DIRECTION ( 'NONE',  ( 0.000000000000000000, -1.000000000000000000, 0.000000000000000000 ) ) ;
#7657 = CIRCLE ( 'NONE', #20184, 11.00000000000000000 ) ;
#7658 = FACE_OUTER_BOUND ( 'NONE', #25367, .T. ) ;
#7659 = CARTESIAN_POINT ( 'NONE',  ( 21.46720264400000033, -36.56420440560000173, -7.810721578089999895 ) ) ;
#7660 = DIRECTION ( 'NONE',  ( 1.000000000000000000, 0.000000000000000000, 0.000000000000000000 ) ) ;
#7661 = DIRECTION ( 'NONE',  ( 1.000000000000000000, 0.000000000000000000, 0.000000000000000000 ) ) ;
#7662 = ORIENTED_EDGE ( 'NONE', *, *, #11222, .F. ) ;
#7663 = CARTESIAN_POINT ( 'NONE',  ( -32.73892505050000068, -74.50000000299999670, -22.13232332930000013 ) ) ;
#7664 = CARTESIAN_POINT ( 'NONE',  ( 47.16620867047740973, -74.55684918557169283, -1.099331675085676086 ) ) ;
#7665 = EDGE_CURVE ( 'NONE', #1616, #22947, #12419, .T. ) ;
#7666 = CARTESIAN_POINT ( 'NONE',  ( 7.473372113619999979, -101.1715639399999986, 13.35082447569999964 ) ) ;
#7667 = VECTOR ( 'NONE', #8701, 1000.000000000000114 ) ;
#7668 = EDGE_CURVE ( 'NONE', #15688, #27211, #21734, .T. ) ;
#7669 = CARTESIAN_POINT ( 'NONE',  ( -11.27251375949999890, -95.14587498419999179, -21.35311122079999890 ) ) ;
#7670 = CARTESIAN_POINT ( 'NONE',  ( 21.32186554389999600, -35.14390151279999230, -7.472189324920000431 ) ) ;
#7671 = CARTESIAN_POINT ( 'NONE',  ( 7.242474372560842255, -73.77182148714507548, 39.65872146204866056 ) ) ;
#7672 = CARTESIAN_POINT ( 'NONE',  ( -14.19074604640000103, -64.47177095450000195, 21.84081649480000209 ) ) ;
#7673 = EDGE_CURVE ( 'NONE', #7380, #20895, #17095, .T. ) ;
#7674 = DIRECTION ( 'NONE',  ( 0.000000000000000000, 1.000000000000000000, 0.000000000000000000 ) ) ;
#7675 = ADVANCED_FACE ( 'NONE', ( #13364 ), #24543, .F. ) ;
#7676 = ORIENTED_EDGE ( 'NONE', *, *, #25458, .T. ) ;
#7677 = AXIS2_PLACEMENT_3D ( 'NONE', #9584, #1915, #15275 ) ;
#7678 = CARTESIAN_POINT ( 'NONE',  ( -0.9701750278467260458, -66.11532767438119151, -25.60589888208034992 ) ) ;
#7679 = CARTESIAN_POINT ( 'NONE',  ( -12.30070879700853581, -60.59571579695742827, -20.16720528227978804 ) ) ;
#7680 = ORIENTED_EDGE ( 'NONE', *, *, #17536, .F. ) ;
#7681 = FACE_OUTER_BOUND ( 'NONE', #4695, .T. ) ;
#7682 = B_SPLINE_CURVE_WITH_KNOTS ( 'NONE', 5,
 ( #9363, #26864, #27302, #18264, #22497, #27157 ),
 .UNSPECIFIED., .F., .F.,
 ( 6, 6 ),
 ( 0.000000000000000000, 1.000000000000000000 ),
 .UNSPECIFIED. ) ;
#7683 = CARTESIAN_POINT ( 'NONE',  ( 7.772412540220105193, -93.00000166546708158, -27.92889321292422977 ) ) ;
#7684 = CARTESIAN_POINT ( 'NONE',  ( 6.186462384450000407, -100.1275643909999928, 15.45527146859999945 ) ) ;
#7685 = DIRECTION ( 'NONE',  ( 0.000000000000000000, -1.000000000000000000, 0.000000000000000000 ) ) ;
#7686 = FACE_OUTER_BOUND ( 'NONE', #4050, .T. ) ;
#7687 = AXIS2_PLACEMENT_3D ( 'NONE', #3308, #9850, #1146 ) ;
#7688 = CARTESIAN_POINT ( 'NONE',  ( 27.75394116159999669, -74.50000000000000000, -27.75394116159999669 ) ) ;
#7689 = DIRECTION ( 'NONE',  ( 0.000000000000000000, 0.000000000000000000, -1.000000000000000000 ) ) ;
#7690 = CARTESIAN_POINT ( 'NONE',  ( -13.85848666890000125, -57.40875702409999803, 21.24403892489999990 ) ) ;
#7691 = CIRCLE ( 'NONE', #24887, 30.50381168839999901 ) ;
#7692 = DIRECTION ( 'NONE',  ( 0.4794255386042040046, 0.000000000000000000, 0.8775825618903722036 ) ) ;
#7693 = CARTESIAN_POINT ( 'NONE',  ( 7.704476223350000375, -25.49730309679999607, -20.86759468720000044 ) ) ;
#7694 = DIRECTION ( 'NONE',  ( 0.000000000000000000, 1.000000000000000000, 0.000000000000000000 ) ) ;
#7695 = SURFACE_SIDE_STYLE ('',( #18757 ) ) ;
#7696 = ORIENTED_EDGE ( 'NONE', *, *, #11528, .F. ) ;
#7697 = AXIS2_PLACEMENT_3D ( 'NONE', #3128, #9938, #14597 ) ;
#7698 = ORIENTED_EDGE ( 'NONE', *, *, #8829, .T. ) ;
#7699 = EDGE_CURVE ( 'NONE', #321, #27403, #4534, .T. ) ;
#7700 = CARTESIAN_POINT ( 'NONE',  ( 50.00000000000000000, -15.00000000000000000, 1.865174681369999824E-14 ) ) ;
#7701 = CARTESIAN_POINT ( 'NONE',  ( -28.93075099380000026, -92.79907188619999658, 3.128477965899999713 ) ) ;
#7702 = CARTESIAN_POINT ( 'NONE',  ( 9.374849361280000792, -94.98812477599999227, -22.63660904189999812 ) ) ;
#7703 = ORIENTED_EDGE ( 'NONE', *, *, #13945, .T. ) ;
#7704 = AXIS2_PLACEMENT_3D ( 'NONE', #28588, #8754, #18109 ) ;
#7705 = ORIENTED_EDGE ( 'NONE', *, *, #16495, .T. ) ;
#7706 = CARTESIAN_POINT ( 'NONE',  ( -28.54678744650632893, -93.15741110514920820, 2.281750724203968073 ) ) ;
#7707 = ORIENTED_EDGE ( 'NONE', *, *, #23738, .F. ) ;
#7708 = CARTESIAN_POINT ( 'NONE',  ( 9.226666976270866627, -71.28737387527178271, -26.41755886876856252 ) ) ;
#7709 = CARTESIAN_POINT ( 'NONE',  ( -11.19714568606054250, -58.31259697909283801, 20.53605202907456828 ) ) ;
#7710 = CARTESIAN_POINT ( 'NONE',  ( 7.202169761539999548, -101.2530994060000040, 13.37848089600000101 ) ) ;
#7711 = CARTESIAN_POINT ( 'NONE',  ( -3.564772898129999756, -71.37991020869999659, -28.09246512229999837 ) ) ;
#7712 = AXIS2_PLACEMENT_3D ( 'NONE', #5348, #2883, #5202 ) ;
#7713 = CARTESIAN_POINT ( 'NONE',  ( -13.83118819819999956, -101.1889999979999999, 21.42307711379999802 ) ) ;
#7714 = ORIENTED_EDGE ( 'NONE', *, *, #7668, .F. ) ;
#7715 = DIRECTION ( 'NONE',  ( -0.9249989688977252600, 0.000000000000000000, -0.3799696139668871098 ) ) ;
#7716 = CARTESIAN_POINT ( 'NONE',  ( -15.77992973249999942, -100.6801306890000092, 2.860126966069999721 ) ) ;
#7717 = CARTESIAN_POINT ( 'NONE',  ( 25.49275922260000016, -60.21420103860000239, 1.382187155250000243 ) ) ;
#7718 = CARTESIAN_POINT ( 'NONE',  ( -6.033294948010268222, -101.1604341566371090, 14.12216738089541401 ) ) ;
#7719 = EDGE_CURVE ( 'NONE', #27440, #17051, #9288, .T. ) ;
#7720 = ORIENTED_EDGE ( 'NONE', *, *, #22928, .F. ) ;
#7721 = DIRECTION ( 'NONE',  ( 1.000000000000000000, 0.000000000000000000, 0.000000000000000000 ) ) ;
#7722 = CARTESIAN_POINT ( 'NONE',  ( 18.94592262313601339, -19.18584073473548557, -9.024080787555618599 ) ) ;
#7723 = CARTESIAN_POINT ( 'NONE',  ( -7.913737673819251306, -100.3041487039959350, 15.11134560035235630 ) ) ;
#7724 = ORIENTED_EDGE ( 'NONE', *, *, #24293, .F. ) ;
#7725 = DIRECTION ( 'NONE',  ( 0.000000000000000000, 1.000000000000000000, 0.000000000000000000 ) ) ;
#7726 = CARTESIAN_POINT ( 'NONE',  ( -31.99184496219999829, -74.00000000000000000, -21.97155633679999909 ) ) ;
#7727 = DIRECTION ( 'NONE',  ( 1.000000000000000000, 0.000000000000000000, 0.000000000000000000 ) ) ;
#7728 = CARTESIAN_POINT ( 'NONE',  ( -2.131628207280000317E-15, -89.50000000000000000, 3.042011087470000117E-15 ) ) ;
#7729 = ORIENTED_EDGE ( 'NONE', *, *, #12974, .F. ) ;
#7730 = ADVANCED_FACE ( 'NONE', ( #13222 ), #23149, .F. ) ;
#7731 = UNCERTAINTY_MEASURE_WITH_UNIT (LENGTH_MEASURE( 1.000000000000000082E-05 ), #6474, 'distance_accuracy_value', 'NONE');
#7732 = CARTESIAN_POINT ( 'NONE',  ( -12.38417342259999998, -18.50000000000000000, 18.05449715319999981 ) ) ;
#7733 = CARTESIAN_POINT ( 'NONE',  ( -14.76023875769999982, -79.50000000000000000, 45.51464203040000456 ) ) ;
#7734 = ORIENTED_EDGE ( 'NONE', *, *, #27637, .T. ) ;
#7735 = LINE ( 'NONE', #25780, #19764 ) ;
#7736 = EDGE_CURVE ( 'NONE', #212, #13629, #2171, .T. ) ;
#7737 = ORIENTED_EDGE ( 'NONE', *, *, #9030, .T. ) ;
#7738 = CARTESIAN_POINT ( 'NONE',  ( -12.91055359849999995, -19.42972397700000187, 19.51083068160000167 ) ) ;
#7739 = CARTESIAN_POINT ( 'NONE',  ( -5.893649827409999986, -101.1042759770000004, 14.64611091109999919 ) ) ;
#7740 = VERTEX_POINT ( 'NONE', #9215 ) ;
#7741 = CARTESIAN_POINT ( 'NONE',  ( -18.06041830838391249, -92.73900887645281443, -23.35381297765049169 ) ) ;
#7742 = DIRECTION ( 'NONE',  ( 0.000000000000000000, 1.000000000000000000, 0.000000000000000000 ) ) ;
#7743 = CARTESIAN_POINT ( 'NONE',  ( 40.00088822930000276, -74.03376264999999989, 7.260991986090000516 ) ) ;
#7744 = FACE_OUTER_BOUND ( 'NONE', #15804, .T. ) ;
#7745 = CARTESIAN_POINT ( 'NONE',  ( 23.25684281378446983, -94.57749869811812005, -6.685465864614543285 ) ) ;
#7746 = CARTESIAN_POINT ( 'NONE',  ( -11.63786782471469472, -61.15154959429087000, -22.95545206538188765 ) ) ;
#7747 = DIRECTION ( 'NONE',  ( 0.000000000000000000, 1.000000000000000000, 0.000000000000000000 ) ) ;
#7748 = ORIENTED_EDGE ( 'NONE', *, *, #1851, .F. ) ;
#7749 = CARTESIAN_POINT ( 'NONE',  ( -32.63463619529999704, -80.04555047089999675, -21.80756975740000314 ) ) ;
#7750 = CARTESIAN_POINT ( 'NONE',  ( 8.805019331468974642, -34.63244845351142942, -20.36793970997746683 ) ) ;
#7751 = EDGE_CURVE ( 'NONE', #400, #1187, #20350, .T. ) ;
#7752 = DIRECTION ( 'NONE',  ( 0.000000000000000000, 1.000000000000000000, 0.000000000000000000 ) ) ;
#7753 = VERTEX_POINT ( 'NONE', #19923 ) ;
#7754 = EDGE_CURVE ( 'NONE', #12707, #18811, #15691, .T. ) ;
#7755 = B_SPLINE_CURVE_WITH_KNOTS ( 'NONE', 5,
 ( #17138, #23430, #16865, #3741, #26028, #6052, #10542, #4018, #3467, #14934, #8111, #1290, #17000, #26177, #25754, #5781, #12460, #12746 ),
 .UNSPECIFIED., .F., .F.,
 ( 6, 3, 3, 3, 3, 6 ),
 ( 0.000000000000000000, 1.124498255620000053, 2.252774941530000241, 3.380756636300000118, 4.508382774210000221, 5.576981603840000190 ),
 .UNSPECIFIED. ) ;
#7756 = CONICAL_SURFACE ( 'NONE', #26815, 55.67692378859999280, 1.047197551199999799 ) ;
#7757 = CARTESIAN_POINT ( 'NONE',  ( -2.677182103140000132E-13, -79.50000000000000000, 47.25000000000000000 ) ) ;
#7758 = CARTESIAN_POINT ( 'NONE',  ( -14.55867152370000106, -64.24504444460001196, 22.15151623919999935 ) ) ;
#7759 = EDGE_LOOP ( 'NONE', ( #16606, #21561, #15892, #17329 ) ) ;
#7760 = CARTESIAN_POINT ( 'NONE',  ( -15.50938341620000216, -101.3150683030000039, 4.855931779240000523 ) ) ;
#7761 = DIRECTION ( 'NONE',  ( 0.000000000000000000, 1.000000000000000000, 0.000000000000000000 ) ) ;
#7762 = CARTESIAN_POINT ( 'NONE',  ( -38.21017963042245214, -65.72001381778288476, 1.308254260898115140 ) ) ;
#7763 = EDGE_CURVE ( 'NONE', #9163, #5413, #24601, .T. ) ;
#7764 = CARTESIAN_POINT ( 'NONE',  ( -14.47093452609578534, -74.09305993903939225, 36.25954071149890012 ) ) ;
#7765 = CARTESIAN_POINT ( 'NONE',  ( 26.33945410830000000, -66.61054971519999413, 1.262719925200000093 ) ) ;
#7766 = EDGE_LOOP ( 'NONE', ( #15982, #19942, #20352, #27101 ) ) ;
#7767 = CARTESIAN_POINT ( 'NONE',  ( 0.000000000000000000, -101.1889999979999999, 0.000000000000000000 ) ) ;
#7768 = CARTESIAN_POINT ( 'NONE',  ( -21.81265874808163829, -79.50000017620000392, -32.68025371919490141 ) ) ;
#7769 = ORIENTED_EDGE ( 'NONE', *, *, #19606, .T. ) ;
#7770 = CARTESIAN_POINT ( 'NONE',  ( -13.36314309979999848, -101.1461874320000049, -9.085681040479999027 ) ) ;
#7771 = CARTESIAN_POINT ( 'NONE',  ( -38.25000000000000000, -63.07912966450000880, -2.684678751729999480 ) ) ;
#7772 = CARTESIAN_POINT ( 'NONE',  ( 9.325629373129999067, -40.69288195509999895, -22.74921183549999881 ) ) ;
#7773 = CARTESIAN_POINT ( 'NONE',  ( 7.288000680640000617, -101.1840739500000126, 13.43345668080000088 ) ) ;
#7774 = ORIENTED_EDGE ( 'NONE', *, *, #21515, .T. ) ;
#7775 = CARTESIAN_POINT ( 'NONE',  ( -39.52985788725224126, -73.70809116064897637, 7.234868202893387945 ) ) ;
#7776 = CARTESIAN_POINT ( 'NONE',  ( -27.23152091140000053, -92.68419354089999729, -4.429291780269999812 ) ) ;
#7777 = CARTESIAN_POINT ( 'NONE',  ( 10.70182951049999964, -96.07623048470000526, -20.38439291359999928 ) ) ;
#7778 = VERTEX_POINT ( 'NONE', #15695 ) ;
#7779 = CARTESIAN_POINT ( 'NONE',  ( 0.000000000000000000, -90.50000000000000000, 0.000000000000000000 ) ) ;
#7780 = EDGE_CURVE ( 'NONE', #9549, #5628, #7385, .T. ) ;
#7781 = DIRECTION ( 'NONE',  ( 1.000000000000000000, 0.000000000000000000, 0.000000000000000000 ) ) ;
#7782 = CARTESIAN_POINT ( 'NONE',  ( -2.619967198309999912, -19.39383846079999785, -24.29735868990000114 ) ) ;
#7783 = DIRECTION ( 'NONE',  ( -0.9704142011833033488, 0.000000000000000000, 0.2414462220490755373 ) ) ;
#7784 = EDGE_CURVE ( 'NONE', #10898, #6598, #2615, .T. ) ;
#7785 = CARTESIAN_POINT ( 'NONE',  ( -1.324264341383242671, -74.17281256843145343, 47.12808568046521174 ) ) ;
#7786 = CARTESIAN_POINT ( 'NONE',  ( -14.42556421679999978, -93.00000000000000000, -2.978755036369999942 ) ) ;
#7787 = CARTESIAN_POINT ( 'NONE',  ( 22.74921183549999881, -40.69288195330000235, -9.325629373219999962 ) ) ;
#7788 = ADVANCED_FACE ( 'NONE', ( #27085 ), #19421, .F. ) ;
#7789 = CARTESIAN_POINT ( 'NONE',  ( 19.97576656849999921, -38.00000000000000000, -19.97576656849999921 ) ) ;
#7790 = DIRECTION ( 'NONE',  ( 0.4794255386042041156, 0.000000000000000000, 0.8775825618903722036 ) ) ;
#7791 = ORIENTED_EDGE ( 'NONE', *, *, #16493, .T. ) ;
#7792 = ADVANCED_FACE ( 'NONE', ( #13811 ), #6373, .F. ) ;
#7793 = CARTESIAN_POINT ( 'NONE',  ( 7.088263367210000609, -101.4254868729999970, 14.30958083260000002 ) ) ;
#7794 = DIRECTION ( 'NONE',  ( 0.000000000000000000, 1.000000000000000000, 0.000000000000000000 ) ) ;
#7795 = CARTESIAN_POINT ( 'NONE',  ( -11.42656773010000038, -94.70364946070000656, -21.14532863000000162 ) ) ;
#7796 = CARTESIAN_POINT ( 'NONE',  ( 19.48147788520000034, -35.35038603809999813, -8.986868840649998802 ) ) ;
#7797 = CARTESIAN_POINT ( 'NONE',  ( 26.77683864449999973, -33.79999999999999716, 49.01467436490000296 ) ) ;
#7798 = CARTESIAN_POINT ( 'NONE',  ( -14.55867152370000106, -64.24504444460001196, 22.15151623919999935 ) ) ;
#7799 = DIRECTION ( 'NONE',  ( -0.9704142011833033488, 0.000000000000000000, 0.2414462220490755373 ) ) ;
#7800 = CIRCLE ( 'NONE', #11489, 0.5000000000000004441 ) ;
#7801 = CARTESIAN_POINT ( 'NONE',  ( 20.54345333939999918, -28.54983945669999912, -8.512196249269999626 ) ) ;
#7802 = EDGE_LOOP ( 'NONE', ( #24667, #13799, #19675, #28616 ) ) ;
#7803 = CARTESIAN_POINT ( 'NONE',  ( -0.8905265619203176497, -65.59529214041724288, -25.37156426618551563 ) ) ;
#7804 = CARTESIAN_POINT ( 'NONE',  ( -4.459621975350000156, -72.00000000000000000, -28.73485931899999812 ) ) ;
#7805 = ORIENTED_EDGE ( 'NONE', *, *, #9736, .F. ) ;
#7806 = CARTESIAN_POINT ( 'NONE',  ( 40.65508461000000295, -75.00000000000000000, -14.75000000000000000 ) ) ;
#7807 = CARTESIAN_POINT ( 'NONE',  ( 0.5792533394982878336, -100.3266728692868384, -17.03019214104271484 ) ) ;
#7808 = CARTESIAN_POINT ( 'NONE',  ( -7.191786296970000159, -73.49999903349998931, 39.02948049420000132 ) ) ;
#7809 = DIRECTION ( 'NONE',  ( 0.000000000000000000, -1.000000000000000000, 0.000000000000000000 ) ) ;
#7810 = CARTESIAN_POINT ( 'NONE',  ( -12.49680195650000059, -94.36515553520000310, -21.45929620349999567 ) ) ;
#7811 = TOROIDAL_SURFACE ( 'NONE', #20835, 10.50000000000000000, 0.5000000000000000000 ) ;
#7812 = CARTESIAN_POINT ( 'NONE',  ( 27.75394116159999669, -74.50000000000000000, -27.75394116159999669 ) ) ;
#7813 = ADVANCED_FACE ( 'NONE', ( #881 ), #26366, .T. ) ;
#7814 = CARTESIAN_POINT ( 'NONE',  ( -22.60001347469999899, -71.86394619589999877, 17.39035019129999782 ) ) ;
#7815 = CARTESIAN_POINT ( 'NONE',  ( 14.36321081490000040, -97.53592492880000009, -14.01782339449999881 ) ) ;
#7816 = B_SPLINE_SURFACE_WITH_KNOTS ( 'NONE', 5, 5, ( 
 ( #14319, #24964, #7339, #9933, #27156, #4995 ),
 ( #13883, #27859, #14994, #8043, #19527, #12391 ),
 ( #17061, #19389, #16788, #10340, #4082, #1354 ),
 ( #23627, #25955, #16931, #8448, #17350, #14592 ),
 ( #3667, #28142, #21863, #23908, #26244, #10065 ),
 ( #21719, #14861, #1500, #12809, #21302, #23765 ) ),
 .UNSPECIFIED., .F., .F., .F.,
 ( 6, 6 ),
 ( 6, 6 ),
 ( 7.179431121690000417, 23.44689954090000228 ),
 ( 0.000000000000000000, 0.5000000000000000000 ),
 .UNSPECIFIED. ) ;
#7817 = B_SPLINE_CURVE_WITH_KNOTS ( 'NONE', 5,
 ( #12260, #5147, #27602, #18976, #18555, #23079 ),
 .UNSPECIFIED., .F., .F.,
 ( 6, 6 ),
 ( 0.000000000000000000, 1.000000000000000000 ),
 .UNSPECIFIED. ) ;
#7818 = CARTESIAN_POINT ( 'NONE',  ( -14.83395525719950570, -101.1411475039999317, 4.096596759523888132 ) ) ;
#7819 = DIRECTION ( 'NONE',  ( 1.000000000000000000, 0.000000000000000000, 0.000000000000000000 ) ) ;
#7820 = FACE_OUTER_BOUND ( 'NONE', #28238, .T. ) ;
#7821 = DIRECTION ( 'NONE',  ( 0.000000000000000000, 1.000000000000000000, 0.000000000000000000 ) ) ;
#7822 = ORIENTED_EDGE ( 'NONE', *, *, #16181, .T. ) ;
#7823 = EDGE_CURVE ( 'NONE', #20072, #16053, #2906, .T. ) ;
#7824 = CARTESIAN_POINT ( 'NONE',  ( 25.26718046270000073, -19.50000000000000000, 6.129403842640000377 ) ) ;
#7825 = AXIS2_PLACEMENT_3D ( 'NONE', #28198, #7830, #23830 ) ;
#7826 = VERTEX_POINT ( 'NONE', #16136 ) ;
#7827 = LINE ( 'NONE', #20662, #20216 ) ;
#7828 = AXIS2_PLACEMENT_3D ( 'NONE', #13527, #27104, #4945 ) ;
#7829 = CARTESIAN_POINT ( 'NONE',  ( -28.60727976599999778, -92.54807930229999613, 3.225833196760000021 ) ) ;
#7830 = DIRECTION ( 'NONE',  ( 0.000000000000000000, -1.000000000000000000, 0.000000000000000000 ) ) ;
#7831 = CYLINDRICAL_SURFACE ( 'NONE', #15321, 0.5000000000000004441 ) ;
#7832 = CARTESIAN_POINT ( 'NONE',  ( -11.26036340160000115, -74.00000000000000000, 46.75000000000000000 ) ) ;
#7833 = VERTEX_POINT ( 'NONE', #11768 ) ;
#7834 = DIRECTION ( 'NONE',  ( 0.000000000000000000, 1.000000000000000000, 0.000000000000000000 ) ) ;
#7835 = CARTESIAN_POINT ( 'NONE',  ( 7.879643458700000380, -36.30219044630000269, -21.38844997820000060 ) ) ;
#7836 = CIRCLE ( 'NONE', #20891, 5.000000000000000888 ) ;
#7837 = CARTESIAN_POINT ( 'NONE',  ( -41.75000000000000000, -65.19264941160000149, 2.595760183509999930 ) ) ;
#7838 = CARTESIAN_POINT ( 'NONE',  ( -22.03254124284932658, -73.99999999999018030, -32.03023314507256458 ) ) ;
#7839 = ORIENTED_EDGE ( 'NONE', *, *, #25700, .F. ) ;
#7840 = CARTESIAN_POINT ( 'NONE',  ( -22.29269500190000386, -94.98812477769999418, -8.065858985560000249 ) ) ;
#7841 = EDGE_CURVE ( 'NONE', #731, #22563, #11915, .T. ) ;
#7842 = CARTESIAN_POINT ( 'NONE',  ( -15.98611562060000146, -101.1238234200000079, 3.186158858430000240 ) ) ;
#7843 = CARTESIAN_POINT ( 'NONE',  ( -20.47152924590000111, -62.13502028410000122, 12.48990793220000128 ) ) ;
#7844 = ORIENTED_EDGE ( 'NONE', *, *, #6042, .F. ) ;
#7845 = CARTESIAN_POINT ( 'NONE',  ( 14.28941763439999946, -111.0000000000000000, -3.575252188409999921 ) ) ;
#7846 = ADVANCED_FACE ( 'NONE', ( #20677 ), #740, .T. ) ;
#7847 = CARTESIAN_POINT ( 'NONE',  ( 18.85230044170000241, -18.50000000000000000, -8.028472989549999994 ) ) ;
#7848 = CARTESIAN_POINT ( 'NONE',  ( 23.53302756460000111, -92.50000000000000000, -18.47479450719999861 ) ) ;
#7849 = VERTEX_POINT ( 'NONE', #27675 ) ;
#7850 = B_SPLINE_CURVE_WITH_KNOTS ( 'NONE', 5,
 ( #6136, #24210, #8741, #3821, #19542, #19684 ),
 .UNSPECIFIED., .F., .F.,
 ( 6, 6 ),
 ( 0.000000000000000000, 1.000000000000000000 ),
 .UNSPECIFIED. ) ;
#7851 = CARTESIAN_POINT ( 'NONE',  ( -50.00000000000000000, -11.00000000000000000, 4.500000000000000000 ) ) ;
#7852 = CARTESIAN_POINT ( 'NONE',  ( 0.000000000000000000, -13.40000000000000036, 0.000000000000000000 ) ) ;
#7853 = CARTESIAN_POINT ( 'NONE',  ( 36.75479982430000092, -80.17662510629999417, -13.92713283259999990 ) ) ;
#7854 = CARTESIAN_POINT ( 'NONE',  ( -3.360703170350179736, -72.70510570383657978, -28.43098690957443253 ) ) ;
#7855 = ORIENTED_EDGE ( 'NONE', *, *, #20104, .F. ) ;
#7856 = B_SPLINE_CURVE_WITH_KNOTS ( 'NONE', 3,
 ( #27268, #14288, #20998, #2795, #20559, #18380, #25081, #23183, #16323, #3092, #1062, #27412, #22903, #3229, #7464, #16172, #11649, #2942, #25234, #5262, #11805, #14149, #11946, #20858, #628, #27705, #917, #9475, #9760, #18671, #27569, #6665, #26785, #11447, #6968 ),
 .UNSPECIFIED., .F., .F.,
 ( 4, 2, 2, 2, 2, 2, 2, 1, 1, 2, 2, 2, 2, 1, 1, 1, 2, 2, 2, 4 ),
 ( 0.000000000000000000, 0.1249999999999768796, 0.1874999999999658051, 0.2187499999999586442, 0.2499999999999514833, 0.3749999999999271694, 0.4374999999999163447, 0.4687499999999097389, 0.4843749999999049649, 0.4921874999999038547, 0.4999999999999027445, 0.6249999999998862021, 0.6874999999998778755, 0.7187499999998737676, 0.7343749999998731015, 0.7421874999998727684, 0.7460937499998714362, 0.7499999999998701039, 0.8749999999999350520, 1.000000000000000000 ),
 .UNSPECIFIED. ) ;
#7857 = CYLINDRICAL_SURFACE ( 'NONE', #23769, 30.50000000000002132 ) ;
#7858 = DIRECTION ( 'NONE',  ( 0.000000000000000000, -1.000000000000000000, 0.000000000000000000 ) ) ;
#7859 = CARTESIAN_POINT ( 'NONE',  ( -0.2062713637372527997, -79.57920433296374085, 47.24999999999999289 ) ) ;
#7860 = VERTEX_POINT ( 'NONE', #16580 ) ;
#7861 = EDGE_CURVE ( 'NONE', #17644, #27454, #3898, .T. ) ;
#7862 = CARTESIAN_POINT ( 'NONE',  ( 47.19280906450000401, -74.66667022419999000, -1.149928383719999836 ) ) ;
#7863 = ORIENTED_EDGE ( 'NONE', *, *, #3255, .F. ) ;
#7864 = CARTESIAN_POINT ( 'NONE',  ( 22.14137210359999841, -52.59522851940000265, 10.05377507689999916 ) ) ;
#7865 = CARTESIAN_POINT ( 'NONE',  ( -5.935386223770000136, -101.3399913430000083, 15.00146626390000115 ) ) ;
#7866 = VERTEX_POINT ( 'NONE', #14798 ) ;
#7867 = CARTESIAN_POINT ( 'NONE',  ( -10.00000000000000000, -89.00000000000000000, 1.224606353819999829E-15 ) ) ;
#7868 = DIRECTION ( 'NONE',  ( 0.4794255386042000078, 0.000000000000000000, 0.8775825618903743131 ) ) ;
#7869 = CIRCLE ( 'NONE', #20925, 23.79684788999999867 ) ;
#7870 = DIRECTION ( 'NONE',  ( 0.8775825618903722036, 0.000000000000000000, -0.4794255386042041156 ) ) ;
#7871 = CARTESIAN_POINT ( 'NONE',  ( 23.93312658989999875, -65.07443093669999712, -7.727579958389999781 ) ) ;
#7872 = CARTESIAN_POINT ( 'NONE',  ( 22.03755794377824273, -95.57586223393636260, -4.946538409496142208 ) ) ;
#7873 = CARTESIAN_POINT ( 'NONE',  ( 46.71300948029226419, -79.88636854212663252, -3.440413976676875762 ) ) ;
#7874 = ORIENTED_EDGE ( 'NONE', *, *, #2284, .T. ) ;
#7875 = CIRCLE ( 'NONE', #15754, 55.50192378860000275 ) ;
#7876 = CARTESIAN_POINT ( 'NONE',  ( -15.01486654579999858, -98.65110728940000229, -11.06499187650000060 ) ) ;
#7877 = EDGE_CURVE ( 'NONE', #9232, #9396, #22398, .T. ) ;
#7878 = DIRECTION ( 'NONE',  ( 0.000000000000000000, 1.000000000000000000, 0.000000000000000000 ) ) ;
#7879 = AXIS2_PLACEMENT_3D ( 'NONE', #22610, #11505, #13852 ) ;
#7880 = DIRECTION ( 'NONE',  ( 1.000000000000000000, 0.000000000000000000, 0.000000000000000000 ) ) ;
#7881 = CARTESIAN_POINT ( 'NONE',  ( 15.16019776770000149, -100.8023006570000035, 4.366346884840000442 ) ) ;
#7882 = ORIENTED_EDGE ( 'NONE', *, *, #18238, .F. ) ;
#7883 = AXIS2_PLACEMENT_3D ( 'NONE', #21071, #9833, #18740 ) ;
#7884 = CARTESIAN_POINT ( 'NONE',  ( -0.7391264416729999009, -79.72071032069999319, 47.25072614749999644 ) ) ;
#7885 = DIRECTION ( 'NONE',  ( 1.000000000000000000, 0.000000000000000000, 0.000000000000000000 ) ) ;
#7886 = ORIENTED_EDGE ( 'NONE', *, *, #8998, .F. ) ;
#7887 = CARTESIAN_POINT ( 'NONE',  ( -17.80822692750000158, -93.00000000000000000, -18.25149456069999943 ) ) ;
#7888 = FACE_OUTER_BOUND ( 'NONE', #18880, .T. ) ;
#7889 = CARTESIAN_POINT ( 'NONE',  ( 4.882943008269999509E-15, -74.50000000000000000, -40.00000000000000000 ) ) ;
#7890 = CARTESIAN_POINT ( 'NONE',  ( 30.10554275930000045, -74.00208038259998489, -25.08120035429999817 ) ) ;
#7891 = CARTESIAN_POINT ( 'NONE',  ( 0.000000000000000000, -92.50000000000000000, 0.000000000000000000 ) ) ;
#7892 = DIRECTION ( 'NONE',  ( 0.4794255386042040601, 0.000000000000000000, 0.8775825618903720926 ) ) ;
#7893 = VECTOR ( 'NONE', #7027, 1000.000000000000000 ) ;
#7894 = DIRECTION ( 'NONE',  ( 0.4794255386042000078, 0.000000000000000000, 0.8775825618903743131 ) ) ;
#7895 = AXIS2_PLACEMENT_3D ( 'NONE', #16057, #2532, #17962 ) ;
#7896 = AXIS2_PLACEMENT_3D ( 'NONE', #3097, #9480, #16329 ) ;
#7897 = ORIENTED_EDGE ( 'NONE', *, *, #19984, .T. ) ;
#7898 = EDGE_CURVE ( 'NONE', #18837, #7960, #24394, .T. ) ;
#7899 = CARTESIAN_POINT ( 'NONE',  ( 9.510880446319999848, -36.06003250090000023, -20.82958080039999871 ) ) ;
#7900 = CARTESIAN_POINT ( 'NONE',  ( -40.28268501247167421, -74.17548517140301101, -7.244487271028503983 ) ) ;
#7901 = CARTESIAN_POINT ( 'NONE',  ( 21.72762743530000051, -37.33446486360000449, -8.509936561279999978 ) ) ;
#7902 = CARTESIAN_POINT ( 'NONE',  ( 19.64032682080000214, -94.52419709919999491, 13.82579343989999998 ) ) ;
#7903 = ORIENTED_EDGE ( 'NONE', *, *, #18637, .F. ) ;
#7904 = CARTESIAN_POINT ( 'NONE',  ( -12.78466493160000006, -101.0848057460000007, -8.608125847929999352 ) ) ;
#7905 = FACE_OUTER_BOUND ( 'NONE', #9447, .T. ) ;
#7906 = CARTESIAN_POINT ( 'NONE',  ( -7.696682359570000465, -100.6809449770000100, 14.52276816779999891 ) ) ;
#7907 = FACE_OUTER_BOUND ( 'NONE', #5471, .T. ) ;
#7908 = FACE_OUTER_BOUND ( 'NONE', #24839, .T. ) ;
#7909 = CARTESIAN_POINT ( 'NONE',  ( 7.483210945499999767, -101.1711668239999966, 13.84080871329999773 ) ) ;
#7910 = ORIENTED_EDGE ( 'NONE', *, *, #7325, .T. ) ;
#7911 = CARTESIAN_POINT ( 'NONE',  ( -40.29875214199796574, -74.18716007598280271, 7.243843118860064934 ) ) ;
#7912 = CARTESIAN_POINT ( 'NONE',  ( -23.97050053409999748, -93.63284696379999161, -7.388385114300000112 ) ) ;
#7913 = CARTESIAN_POINT ( 'NONE',  ( 23.30859914190000026, -49.64525644009999894, -9.491876184740000610 ) ) ;
#7914 = ORIENTED_EDGE ( 'NONE', *, *, #26886, .T. ) ;
#7915 = DIRECTION ( 'NONE',  ( 0.4151946956541399669, 0.5000000000001689759, 0.7600087925152558821 ) ) ;
#7916 = CARTESIAN_POINT ( 'NONE',  ( 11.71858627609999992, -101.1499348409999897, -10.52473037210000051 ) ) ;
#7917 = CARTESIAN_POINT ( 'NONE',  ( -14.27099507389999999, -74.08594823550001252, 36.51725837320000068 ) ) ;
#7918 = CARTESIAN_POINT ( 'NONE',  ( -2.640278312650000014, -19.41837863920000018, -23.60024879370000050 ) ) ;
#7919 = CARTESIAN_POINT ( 'NONE',  ( -17.21128535244866242, -92.77481473473854123, 25.17988932136048064 ) ) ;
#7920 = VECTOR ( 'NONE', #14895, 1000.000000000000000 ) ;
#7921 = AXIS2_PLACEMENT_3D ( 'NONE', #136, #25028, #11603 ) ;
#7922 = CARTESIAN_POINT ( 'NONE',  ( -0.01895569543850000177, -101.5216621940000152, -16.01048889870000025 ) ) ;
#7923 = CARTESIAN_POINT ( 'NONE',  ( 0.000000000000000000, -16.50000000000000000, 0.000000000000000000 ) ) ;
#7924 = CARTESIAN_POINT ( 'NONE',  ( -39.23631980030000221, -73.50064222389998747, -7.229366192830000593 ) ) ;
#7925 = CARTESIAN_POINT ( 'NONE',  ( 8.185346967789998374, -101.3150701389999995, 14.03998109830000018 ) ) ;
#7926 = CARTESIAN_POINT ( 'NONE',  ( -10.58792824859999904, -27.05112424559999695, -20.39366723639999890 ) ) ;
#7927 = ORIENTED_EDGE ( 'NONE', *, *, #3723, .F. ) ;
#7928 = CARTESIAN_POINT ( 'NONE',  ( 6.749096951940000366, -101.2063419769999939, 14.49232149449999874 ) ) ;
#7929 = CARTESIAN_POINT ( 'NONE',  ( 13.87577342641885103, -97.43430234697039793, -15.18291532359526919 ) ) ;
#7930 = CARTESIAN_POINT ( 'NONE',  ( -10.20110288159999890, -80.00000000000000000, 41.00000000000000000 ) ) ;
#7931 = CARTESIAN_POINT ( 'NONE',  ( 36.24656994149999889, -79.27200282849999269, -15.05817610060000078 ) ) ;
#7932 = DIRECTION ( 'NONE',  ( 1.000000000000000000, 0.000000000000000000, 0.000000000000000000 ) ) ;
#7933 = CIRCLE ( 'NONE', #39, 8.000000000000000000 ) ;
#7935 = ADVANCED_FACE ( 'NONE', ( #6347 ), #9825, .T. ) ;
#7934 = AXIS2_PLACEMENT_3D ( 'NONE', #13101, #17349, #19388 ) ;
#7936 = TOROIDAL_SURFACE ( 'NONE', #1008, 10.50000000000000000, 0.5000000000000000000 ) ;
#7937 = CYLINDRICAL_SURFACE ( 'NONE', #27996, 61.34999999999998721 ) ;
#7938 = ORIENTED_EDGE ( 'NONE', *, *, #22270, .T. ) ;
#7939 = CARTESIAN_POINT ( 'NONE',  ( -24.63993737860000266, -72.00000000000000000, 17.98210258840000009 ) ) ;
#7940 = DIRECTION ( 'NONE',  ( 0.000000000000000000, -1.000000000000000000, 0.000000000000000000 ) ) ;
#7941 = VERTEX_POINT ( 'NONE', #19053 ) ;
#7942 = EDGE_CURVE ( 'NONE', #10479, #5689, #7755, .T. ) ;
#7943 = DIRECTION ( 'NONE',  ( 0.000000000000000000, 1.000000000000000000, 0.000000000000000000 ) ) ;
#7944 = EDGE_CURVE ( 'NONE', #23662, #17905, #18531, .T. ) ;
#7945 = VERTEX_POINT ( 'NONE', #3597 ) ;
#7946 = CARTESIAN_POINT ( 'NONE',  ( 0.5907866879554720674, -100.3796496172627144, -16.98725527372521782 ) ) ;
#7947 = CARTESIAN_POINT ( 'NONE',  ( 6.355965434729999863, -99.91102932029998840, 15.68918534660000041 ) ) ;
#7948 = DIRECTION ( 'NONE',  ( 1.000000000000000000, 0.000000000000000000, 0.000000000000000000 ) ) ;
#7949 = CARTESIAN_POINT ( 'NONE',  ( 23.57688669830000094, -73.34335239639999315, -30.75933940510000042 ) ) ;
#7950 = DIRECTION ( 'NONE',  ( -0.9408314849018032389, 0.000000000000000000, 0.3388747807339287932 ) ) ;
#7951 = CARTESIAN_POINT ( 'NONE',  ( 20.51721036366772921, -93.01584921895947389, 16.65400312716379005 ) ) ;
#7952 = CARTESIAN_POINT ( 'NONE',  ( 23.92053897610000135, -111.0000000000000000, -18.92241567810000191 ) ) ;
#7953 = CARTESIAN_POINT ( 'NONE',  ( 0.000000000000000000, -10.95575221240000019, 0.000000000000000000 ) ) ;
#7954 = CARTESIAN_POINT ( 'NONE',  ( -41.45000000000000284, -63.07912966450000880, 2.857883832489999776 ) ) ;
#7955 = CIRCLE ( 'NONE', #5623, 0.4999999999999990008 ) ;
#7956 = VERTEX_POINT ( 'NONE', #21373 ) ;
#7957 = CIRCLE ( 'NONE', #16339, 4.750000000000000000 ) ;
#7958 = CARTESIAN_POINT ( 'NONE',  ( -41.37299426109999700, -65.19264941160000149, 2.813424548390000002 ) ) ;
#7959 = VECTOR ( 'NONE', #2688, 1000.000000000000000 ) ;
#7960 = VERTEX_POINT ( 'NONE', #19185 ) ;
#7961 = DIRECTION ( 'NONE',  ( 0.000000000000000000, 1.000000000000000000, 0.000000000000000000 ) ) ;
#7962 = CARTESIAN_POINT ( 'NONE',  ( -27.88330092360000023, -92.65715406920001840, 1.774534369700000003 ) ) ;
#7963 = LINE ( 'NONE', #25745, #4066 ) ;
#7964 = EDGE_CURVE ( 'NONE', #9320, #21728, #25890, .T. ) ;
#7965 = ORIENTED_EDGE ( 'NONE', *, *, #12776, .T. ) ;
#7966 = B_SPLINE_CURVE_WITH_KNOTS ( 'NONE', 3,
 ( #4640, #26942, #20084, #17467, #6985, #6689, #28529, #26353, #19639, #13518, #4491, #26646 ),
 .UNSPECIFIED., .F., .F.,
 ( 4, 2, 2, 2, 2, 4 ),
 ( 0.000000000000000000, 0.2500000000000262568, 0.3750000000000481837, 0.4375000000000474065, 0.5000000000000466294, 1.000000000000000000 ),
 .UNSPECIFIED. ) ;
#7967 = DIRECTION ( 'NONE',  ( 1.000000000000000000, 0.000000000000000000, 0.000000000000000000 ) ) ;
#7968 = DIRECTION ( 'NONE',  ( 1.000000000000000000, 0.000000000000000000, 3.652049423109066841E-16 ) ) ;
#7969 = ORIENTED_EDGE ( 'NONE', *, *, #6439, .T. ) ;
#7970 = TOROIDAL_SURFACE ( 'NONE', #9840, 21.14285714289999873, 0.5000000000000000000 ) ;
#7971 = CARTESIAN_POINT ( 'NONE',  ( 9.720255118479999012, -72.82938648530000592, -26.98670296669999757 ) ) ;
#7972 = CARTESIAN_POINT ( 'NONE',  ( 7.356933664330000511, -36.56811125370000326, -21.47791242339999940 ) ) ;
#7973 = AXIS2_PLACEMENT_3D ( 'NONE', #25497, #25368, #22894 ) ;
#7974 = EDGE_CURVE ( 'NONE', #11046, #2039, #13538, .T. ) ;
#7975 = CARTESIAN_POINT ( 'NONE',  ( -22.13524825866949897, -74.09417207393364890, -32.44781384942801594 ) ) ;
#7976 = ORIENTED_EDGE ( 'NONE', *, *, #12380, .F. ) ;
#7977 = CARTESIAN_POINT ( 'NONE',  ( -15.39442787059999951, -101.4333525140000063, 4.601335728080000465 ) ) ;
#7978 = CARTESIAN_POINT ( 'NONE',  ( -16.54845023329999876, -100.2711349300000023, 3.073083695130000237 ) ) ;
#7979 = CARTESIAN_POINT ( 'NONE',  ( -32.74238892021038083, -74.28135380449873537, -22.20662981729911323 ) ) ;
#7980 = CARTESIAN_POINT ( 'NONE',  ( -6.285925807789999986, -101.6484611540000031, 14.71350185169999847 ) ) ;
#7981 = ORIENTED_EDGE ( 'NONE', *, *, #11049, .F. ) ;
#7982 = DIRECTION ( 'NONE',  ( 1.000000000000000000, 0.000000000000000000, 0.000000000000000000 ) ) ;
#7983 = CARTESIAN_POINT ( 'NONE',  ( -40.00000000000000000, -94.00000000000000000, 0.000000000000000000 ) ) ;
#7984 = CARTESIAN_POINT ( 'NONE',  ( -1.420008363560000042, -19.15770089200000115, -22.10039692550000012 ) ) ;
#7985 = CARTESIAN_POINT ( 'NONE',  ( -7.685338361321690570, -100.9510322833058495, 14.64991780641961938 ) ) ;
#7986 = ORIENTED_EDGE ( 'NONE', *, *, #14662, .F. ) ;
#7987 = CARTESIAN_POINT ( 'NONE',  ( -37.75000000000000000, -64.47022873560000278, 0.7216878364859999895 ) ) ;
#7988 = FACE_OUTER_BOUND ( 'NONE', #17148, .T. ) ;
#7989 = CARTESIAN_POINT ( 'NONE',  ( 36.70830968599999977, -79.00000000000000000, -14.75000000000000000 ) ) ;
#7990 = EDGE_LOOP ( 'NONE', ( #27218, #16604, #23206, #10724 ) ) ;
#7991 = VECTOR ( 'NONE', #16337, 1000.000000000000000 ) ;
#7992 = CIRCLE ( 'NONE', #26604, 4.750000000000000888 ) ;
#7993 = EDGE_CURVE ( 'NONE', #27297, #12297, #20057, .T. ) ;
#7994 = CARTESIAN_POINT ( 'NONE',  ( 36.76713440047162607, -79.42549758800066684, -14.65509726804374679 ) ) ;
#7995 = CARTESIAN_POINT ( 'NONE',  ( 6.661118870793237612, -100.9616911410331994, 15.13395055016176016 ) ) ;
#7996 = DIRECTION ( 'NONE',  ( -1.000000000000000000, 0.000000000000000000, 0.000000000000000000 ) ) ;
#7997 = VERTEX_POINT ( 'NONE', #6499 ) ;
#7998 = ADVANCED_FACE ( 'NONE', ( #6949 ), #111, .F. ) ;
#7999 = CARTESIAN_POINT ( 'NONE',  ( 46.72780802417965162, -73.83257802372662582, -2.701702527458963665 ) ) ;
#8000 = ORIENTED_EDGE ( 'NONE', *, *, #15909, .T. ) ;
#8001 = FACE_OUTER_BOUND ( 'NONE', #20329, .T. ) ;
#8002 = CARTESIAN_POINT ( 'NONE',  ( -5.912079742529999571, -101.4309749570000037, 15.04392878760000052 ) ) ;
#8003 = ORIENTED_EDGE ( 'NONE', *, *, #15980, .F. ) ;
#8004 = EDGE_CURVE ( 'NONE', #18698, #3896, #15870, .T. ) ;
#8005 = PLANE ( 'NONE',  #1104 ) ;
#8006 = CARTESIAN_POINT ( 'NONE',  ( 47.25008975959999447, -74.83017303949999643, -0.5756401097749999085 ) ) ;
#8007 = EDGE_CURVE ( 'NONE', #22875, #12945, #7529, .T. ) ;
#8008 = CARTESIAN_POINT ( 'NONE',  ( 40.70731707320000226, -74.50000000000000000, 7.215414233289999757 ) ) ;
#8009 = CARTESIAN_POINT ( 'NONE',  ( 9.644866014229998896, -36.00000000000000000, -20.16453884109999706 ) ) ;
#8010 = CARTESIAN_POINT ( 'NONE',  ( -11.73327706972289697, -62.33680847863706731, -23.17541252891790649 ) ) ;
#8011 = DIRECTION ( 'NONE',  ( 1.000000000000000000, 0.000000000000000000, 0.000000000000000000 ) ) ;
#8012 = ORIENTED_EDGE ( 'NONE', *, *, #15980, .T. ) ;
#8013 = CARTESIAN_POINT ( 'NONE',  ( -13.14564498500000056, -99.53431242750001218, -11.42100405340000080 ) ) ;
#8014 = FACE_OUTER_BOUND ( 'NONE', #12387, .T. ) ;
#8015 = CARTESIAN_POINT ( 'NONE',  ( -20.20033130439999880, -94.89196636830000386, 12.35535293270000068 ) ) ;
#8016 = CARTESIAN_POINT ( 'NONE',  ( 24.76017301490000122, -92.96321827549999739, -15.38621121709999962 ) ) ;
#8017 = CARTESIAN_POINT ( 'NONE',  ( -2.580650340169999613, -54.98594849529999351, -25.17323918700000362 ) ) ;
#8018 = CARTESIAN_POINT ( 'NONE',  ( 29.72507353699757715, -92.83865970264098166, 6.831545584289306028 ) ) ;
#8019 = DIRECTION ( 'NONE',  ( 0.4794255386042036715, 0.000000000000000000, 0.8775825618903724257 ) ) ;
#8020 = ORIENTED_EDGE ( 'NONE', *, *, #14353, .T. ) ;
#8021 = CARTESIAN_POINT ( 'NONE',  ( -15.48259164459999937, -101.2306293330000102, 4.813005033020000489 ) ) ;
#8022 = FACE_OUTER_BOUND ( 'NONE', #27548, .T. ) ;
#8023 = CARTESIAN_POINT ( 'NONE',  ( 6.089256317429503795, -92.55389105863930865, 29.05547583162038805 ) ) ;
#8024 = CARTESIAN_POINT ( 'NONE',  ( 29.84865827459999821, -73.21937500890000194, -25.22286250999999879 ) ) ;
#8025 = CARTESIAN_POINT ( 'NONE',  ( -16.01432518157788465, -72.70510571236322050, 23.73092384619475936 ) ) ;
#8026 = AXIS2_PLACEMENT_3D ( 'NONE', #4155, #12873, #24266 ) ;
#8027 = AXIS2_PLACEMENT_3D ( 'NONE', #3344, #27689, #3483 ) ;
#8028 = B_SPLINE_CURVE_WITH_KNOTS ( 'NONE', 3,
 ( #8410, #15102, #8561, #28234, #13068, #17316 ),
 .UNSPECIFIED., .F., .F.,
 ( 4, 2, 4 ),
 ( 0.000000000000000000, 0.5000000000000000000, 1.000000000000000000 ),
 .UNSPECIFIED. ) ;
#8029 = CIRCLE ( 'NONE', #11748, 6.750000000000000000 ) ;
#8031 = ORIENTED_EDGE ( 'NONE', *, *, #22080, .F. ) ;
#8030 = EDGE_CURVE ( 'NONE', #20122, #8526, #20195, .T. ) ;
#8032 = ADVANCED_FACE ( 'NONE', ( #6800, #24720, #26466, #15358, #19747, #2434 ), #2138, .T. ) ;
#8033 = CARTESIAN_POINT ( 'NONE',  ( -39.79858521607874167, -73.85166138383344503, -7.247217007272896971 ) ) ;
#8034 = B_SPLINE_CURVE_WITH_KNOTS ( 'NONE', 5,
 ( #7225, #16233, #835, #4887, #14217, #11716, #4738, #14061, #22814 ),
 .UNSPECIFIED., .F., .F.,
 ( 6, 3, 6 ),
 ( 0.000000000000000000, 0.5000000000000000000, 1.000000000000000000 ),
 .UNSPECIFIED. ) ;
#8035 = DIRECTION ( 'NONE',  ( 1.000000000000000000, 0.000000000000000000, 0.000000000000000000 ) ) ;
#8036 = CARTESIAN_POINT ( 'NONE',  ( 19.60651811670000200, -94.52293512109999085, 13.72233059890000106 ) ) ;
#8037 = EDGE_LOOP ( 'NONE', ( #6049, #18145, #26210, #12524 ) ) ;
#8038 = CARTESIAN_POINT ( 'NONE',  ( 9.119802927630001221, -98.28914429610000525, 16.69368728350000097 ) ) ;
#8039 = B_SPLINE_SURFACE_WITH_KNOTS ( 'NONE', 5, 5, ( 
 ( #13220, #9138, #24898, #11462, #4789, #16676, #4636, #24753, #26797 ),
 ( #28658, #10867, #17607, #4929, #6829, #22421, #2027, #26495, #2467 ),
 ( #15392, #2169, #26938, #13667, #11005, #8843, #26639, #17322, #10447 ),
 ( #26501, #10872, #14970, #6538, #8696, #14834, #12783, #15107, #4353 ),
 ( #15246, #23882, #19782, #12919, #28664, #21835, #8566, #23736, #21691 ),
 ( #13225, #15398, #3918, #24313, #3780, #22133, #1889, #1739, #13075 ),
 ( #6383, #5950, #10580, #26064, #17177, #19640, #12641, #4052, #21984 ),
 ( #17612, #19501, #2174, #10726, #19225, #8277, #2032, #28113, #17037 ),
 ( #8150, #25927, #21554, #1609, #24167, #19366, #28385, #17469, #28241 ),
 ( #8416, #26216, #6244, #24019, #6092, #28530, #26354, #4200, #11327 ),
 ( #8848, #6691, #13815, #15998, #16140, #6834, #22720, #18348, #15553 ),
 ( #20085, #4795, #9293, #17909, #1, #2319, #26802, #2473, #2620 ) ),
 .UNSPECIFIED., .F., .F., .F.,
 ( 6, 3, 3, 6 ),
 ( 6, 3, 6 ),
 ( 3.852920539479999906, 4.834764074430000669, 6.134713715070000184, 8.383984506250000024 ),
 ( 0.000000000000000000, 0.2500000000000000000, 0.5000000000000000000 ),
 .UNSPECIFIED. ) ;
#8040 = CARTESIAN_POINT ( 'NONE',  ( -18.11118464990000021, -92.50000169800000549, -23.63835352659999955 ) ) ;
#8041 = CARTESIAN_POINT ( 'NONE',  ( -8.238075515089999357, -99.92384627689999377, 14.76899840829999988 ) ) ;
#8042 = ORIENTED_EDGE ( 'NONE', *, *, #21842, .T. ) ;
#8043 = CARTESIAN_POINT ( 'NONE',  ( 3.892082198189999787, -92.58502644590001296, 28.36234172580000390 ) ) ;
#8044 = DIRECTION ( 'NONE',  ( 0.4794255386042040601, 0.000000000000000000, 0.8775825618903720926 ) ) ;
#8045 = CARTESIAN_POINT ( 'NONE',  ( 7.563340576460000797, -101.3249909679999945, 13.99392069269999972 ) ) ;
#8046 = ORIENTED_EDGE ( 'NONE', *, *, #5733, .T. ) ;
#8047 = DIRECTION ( 'NONE',  ( 1.000000000000000000, 0.000000000000000000, 0.000000000000000000 ) ) ;
#8048 = DIRECTION ( 'NONE',  ( 1.000000000000000000, 0.000000000000000000, 0.000000000000000000 ) ) ;
#8049 = CARTESIAN_POINT ( 'NONE',  ( 25.72091892060000262, -71.70959084179999365, 11.50978681670000014 ) ) ;
#8050 = DIRECTION ( 'NONE',  ( 0.4794255386042033384, 0.000000000000000000, 0.8775825618903726477 ) ) ;
#8051 = ORIENTED_EDGE ( 'NONE', *, *, #5118, .T. ) ;
#8052 = CARTESIAN_POINT ( 'NONE',  ( 9.356041104380000917, -74.50000000000000000, 37.60355029590000697 ) ) ;
#8053 = CIRCLE ( 'NONE', #25736, 59.33923303830000151 ) ;
#8054 = AXIS2_PLACEMENT_3D ( 'NONE', #18776, #27672, #27227 ) ;
#8055 = DIRECTION ( 'NONE',  ( 1.000000000000000000, 0.000000000000000000, 0.000000000000000000 ) ) ;
#8056 = CARTESIAN_POINT ( 'NONE',  ( -18.17993916029999824, -94.51629284240000572, 17.35042103430000182 ) ) ;
#8057 = EDGE_LOOP ( 'NONE', ( #21977, #24714, #6438, #28620 ) ) ;
#8058 = DIRECTION ( 'NONE',  ( 0.000000000000000000, -1.000000000000000000, 0.000000000000000000 ) ) ;
#8059 = EDGE_CURVE ( 'NONE', #14426, #1856, #23776, .T. ) ;
#8060 = CARTESIAN_POINT ( 'NONE',  ( -0.1769176043900000106, -101.3256027139999986, -15.90570293400000246 ) ) ;
#8061 = CARTESIAN_POINT ( 'NONE',  ( 7.859713442080000334, -62.11705451429999414, -22.72424446479999816 ) ) ;
#8062 = CARTESIAN_POINT ( 'NONE',  ( -39.18035607909999385, -73.62951539690000402, -7.219507042800000107 ) ) ;
#8063 = DIRECTION ( 'NONE',  ( 0.000000000000000000, -1.000000000000000000, 0.000000000000000000 ) ) ;
#8064 = CARTESIAN_POINT ( 'NONE',  ( 3.355978770230000130, 4.440892098500000496E-16, 6.143077933229999843 ) ) ;
#8065 = ORIENTED_EDGE ( 'NONE', *, *, #4911, .F. ) ;
#8066 = CARTESIAN_POINT ( 'NONE',  ( 6.641904396630000207, -100.8746138070000029, 15.21662664139999954 ) ) ;
#8067 = CARTESIAN_POINT ( 'NONE',  ( -17.01539865379871586, -92.51381484706730873, -23.94002819195306841 ) ) ;
#8068 = TOROIDAL_SURFACE ( 'NONE', #28069, 39.75000000000000000, 0.5000000000000000000 ) ;
#8069 = CARTESIAN_POINT ( 'NONE',  ( -5.520527781993984640, -97.05288879771497079, 20.32268517453738710 ) ) ;
#8070 = EDGE_CURVE ( 'NONE', #9249, #3079, #22232, .T. ) ;
#8071 = FACE_OUTER_BOUND ( 'NONE', #14249, .T. ) ;
#8072 = DIRECTION ( 'NONE',  ( -0.09756097560976667582, 0.000000000000000000, -0.9952295494196654602 ) ) ;
#8073 = CARTESIAN_POINT ( 'NONE',  ( 4.413832159080181228, -92.82044061125340306, -30.17893592457920349 ) ) ;
#8074 = CARTESIAN_POINT ( 'NONE',  ( -6.595572254019999470, -97.73638926229999413, 18.83567684839999856 ) ) ;
#8075 = AXIS2_PLACEMENT_3D ( 'NONE', #4095, #28571, #8606 ) ;
#8076 = CARTESIAN_POINT ( 'NONE',  ( 6.595758072439999786, -93.30149055180000062, -26.35103330869999994 ) ) ;
#8077 = CARTESIAN_POINT ( 'NONE',  ( 21.92880668189999938, -37.95796630759999601, -8.677144286330001677 ) ) ;
#8078 = DIRECTION ( 'NONE',  ( 1.000000000000000000, 0.000000000000000000, 0.000000000000000000 ) ) ;
#8079 = ORIENTED_EDGE ( 'NONE', *, *, #14230, .F. ) ;
#8080 = CARTESIAN_POINT ( 'NONE',  ( -12.47307327141018263, -62.13475794627616011, -20.48184207972035864 ) ) ;
#8081 = ORIENTED_EDGE ( 'NONE', *, *, #19348, .T. ) ;
#8082 = CARTESIAN_POINT ( 'NONE',  ( -0.9804619217829999567, -101.6095085860000040, -16.00001407889999783 ) ) ;
#8083 = CARTESIAN_POINT ( 'NONE',  ( -17.00715350810000004, -111.0000000000000000, 3.484608414699999823 ) ) ;
#8084 = AXIS2_PLACEMENT_3D ( 'NONE', #28737, #6459, #26575 ) ;
#8085 = CARTESIAN_POINT ( 'NONE',  ( 13.19216279811974424, -92.83865970264201906, 27.49939731263290099 ) ) ;
#8086 = DIRECTION ( 'NONE',  ( 1.000000000000000000, 0.000000000000000000, 0.000000000000000000 ) ) ;
#8087 = CARTESIAN_POINT ( 'NONE',  ( 21.98819667889999963, -72.24515058779999777, -30.92234068899999855 ) ) ;
#8088 = CARTESIAN_POINT ( 'NONE',  ( -22.96356986949999879, -71.26873020080000742, 15.97477082700000217 ) ) ;
#8089 = CARTESIAN_POINT ( 'NONE',  ( 19.97576656849999921, -36.00000000000000000, -19.97576656849999921 ) ) ;
#8090 = FACE_OUTER_BOUND ( 'NONE', #17030, .T. ) ;
#8091 = AXIS2_PLACEMENT_3D ( 'NONE', #20657, #7821, #5763 ) ;
#8092 = DIRECTION ( 'NONE',  ( 0.7600087925152557711, 0.5000000000001688649, 0.4151946956541399114 ) ) ;
#8093 = VERTEX_POINT ( 'NONE', #24273 ) ;
#8094 = EDGE_CURVE ( 'NONE', #3189, #23988, #268, .T. ) ;
#8095 = CARTESIAN_POINT ( 'NONE',  ( -10.93437413680000070, -19.50000027030000282, -21.85842452360000010 ) ) ;
#8096 = ORIENTED_EDGE ( 'NONE', *, *, #21049, .T. ) ;
#8097 = ADVANCED_FACE ( 'NONE', ( #2282 ), #4312, .F. ) ;
#8098 = AXIS2_PLACEMENT_3D ( 'NONE', #6182, #20832, #8223 ) ;
#8099 = CARTESIAN_POINT ( 'NONE',  ( -2.453168467159999810, -64.58097839929999395, -25.72104876729999745 ) ) ;
#8100 = AXIS2_PLACEMENT_3D ( 'NONE', #13040, #28776, #26324 ) ;
#8101 = DIRECTION ( 'NONE',  ( 0.000000000000000000, 1.000000000000000000, 0.000000000000000000 ) ) ;
#8102 = CARTESIAN_POINT ( 'NONE',  ( -19.49041480450000208, -52.62618816519999854, 12.93508487010000074 ) ) ;
#8103 = CARTESIAN_POINT ( 'NONE',  ( 2.798556025240000070E-15, -74.00000000000000000, 3.175502518160000051E-15 ) ) ;
#8104 = ORIENTED_EDGE ( 'NONE', *, *, #23213, .T. ) ;
#8105 = DIRECTION ( 'NONE',  ( -0.8775825618903722036, 0.000000000000000000, 0.4794255386042041156 ) ) ;
#8106 = VERTEX_POINT ( 'NONE', #405 ) ;
#8107 = CIRCLE ( 'NONE', #11831, 0.7500000000000006661 ) ;
#8108 = DIRECTION ( 'NONE',  ( 0.9704142011833034598, 0.000000000000000000, -0.2414462220490750377 ) ) ;
#8109 = CARTESIAN_POINT ( 'NONE',  ( -14.59815756470000103, -79.67649849320000044, 36.63377403959999867 ) ) ;
#8110 = AXIS2_PLACEMENT_3D ( 'NONE', #18138, #4588, #27037 ) ;
#8111 = CARTESIAN_POINT ( 'NONE',  ( -17.49621775540000002, -18.50000000000000000, 12.96682185270000076 ) ) ;
#8112 = ADVANCED_BREP_SHAPE_REPRESENTATION ( '', ( #25398, #26433 ), #4100 ) ;
#8113 = CARTESIAN_POINT ( 'NONE',  ( -15.52809674979999954, -101.4254868729999970, 3.726364514469999722 ) ) ;
#8114 = FACE_OUTER_BOUND ( 'NONE', #15441, .T. ) ;
#8115 = CARTESIAN_POINT ( 'NONE',  ( -19.84213263739999888, -59.03816558840000539, 12.43676266369999972 ) ) ;
#8116 = VERTEX_POINT ( 'NONE', #13188 ) ;
#8117 = DIRECTION ( 'NONE',  ( 1.000000000000000000, 0.000000000000000000, 0.000000000000000000 ) ) ;
#8118 = CARTESIAN_POINT ( 'NONE',  ( -12.44238872350000058, -101.2251655520000071, -10.41030240340000113 ) ) ;
#8119 = EDGE_CURVE ( 'NONE', #9278, #13587, #27441, .T. ) ;
#8120 = SURFACE_STYLE_FILL_AREA ( #13046 ) ;
#8121 = CARTESIAN_POINT ( 'NONE',  ( -7.896941525246588434, -100.4103893717344960, 15.02389615286374180 ) ) ;
#8122 = EDGE_LOOP ( 'NONE', ( #11737, #10330, #28260, #6641 ) ) ;
#8123 = EDGE_CURVE ( 'NONE', #7539, #77, #19953, .T. ) ;
#8124 = CARTESIAN_POINT ( 'NONE',  ( -41.68250231393139416, -65.09619745166486382, -2.836002908389325672 ) ) ;
#8125 = CARTESIAN_POINT ( 'NONE',  ( 1.509903313490000218E-14, -80.50000000000000000, 40.00000000000000000 ) ) ;
#8126 = CARTESIAN_POINT ( 'NONE',  ( 36.54853060579999635, -79.95823378070001297, -14.43173195999999869 ) ) ;
#8127 = ORIENTED_EDGE ( 'NONE', *, *, #11125, .F. ) ;
#8128 = ADVANCED_FACE ( 'NONE', ( #27052 ), #12066, .T. ) ;
#8129 = ADVANCED_FACE ( 'NONE', ( #24421 ), #4623, .T. ) ;
#8130 = AXIS2_PLACEMENT_3D ( 'NONE', #26487, #17307, #13211 ) ;
#8131 = CARTESIAN_POINT ( 'NONE',  ( 0.000000000000000000, -108.5000000000000000, 0.000000000000000000 ) ) ;
#8132 = CARTESIAN_POINT ( 'NONE',  ( 6.860655828344782492, -100.3379349521298565, 15.58801274157079320 ) ) ;
#8133 = CARTESIAN_POINT ( 'NONE',  ( 16.73195129730000374, -83.75000000000000000, 30.62763141000000289 ) ) ;
#8134 = ORIENTED_EDGE ( 'NONE', *, *, #5861, .F. ) ;
#8135 = CARTESIAN_POINT ( 'NONE',  ( 46.45856493942430632, -73.64909968962108167, -3.295201590591422924 ) ) ;
#8136 = VERTEX_POINT ( 'NONE', #18010 ) ;
#8137 = AXIS2_PLACEMENT_3D ( 'NONE', #5959, #28121, #27584 ) ;
#8138 = CARTESIAN_POINT ( 'NONE',  ( 21.01614117329999942, -55.04870336940000186, 10.45594076380000104 ) ) ;
#8139 = B_SPLINE_CURVE_WITH_KNOTS ( 'NONE', 5,
 ( #11711, #16382, #22962, #25292, #19004, #16227 ),
 .UNSPECIFIED., .F., .F.,
 ( 6, 6 ),
 ( 0.000000000000000000, 1.000000000000000000 ),
 .UNSPECIFIED. ) ;
#8140 = CARTESIAN_POINT ( 'NONE',  ( 7.215414233289999757, -74.50000000000000000, 40.70731707320000226 ) ) ;
#8141 = VERTEX_POINT ( 'NONE', #12018 ) ;
#8142 = CARTESIAN_POINT ( 'NONE',  ( -38.62788938250000115, -74.00000000000000000, -7.627566167509999495 ) ) ;
#8143 = FACE_OUTER_BOUND ( 'NONE', #4850, .T. ) ;
#8144 = ORIENTED_EDGE ( 'NONE', *, *, #2493, .T. ) ;
#8145 = CARTESIAN_POINT ( 'NONE',  ( 22.97877291159999658, -37.99999999279999230, -9.393614097370001303 ) ) ;
#8146 = CARTESIAN_POINT ( 'NONE',  ( 7.318052426040000391, -101.1822553929999913, 13.41977313900000013 ) ) ;
#8147 = CARTESIAN_POINT ( 'NONE',  ( 25.49721913128534823, -67.92876907154627020, 10.87395732963725692 ) ) ;
#8148 = VERTEX_POINT ( 'NONE', #25448 ) ;
#8149 = CARTESIAN_POINT ( 'NONE',  ( -1.604070449259999753, -100.9197075889999979, -15.54198650660000069 ) ) ;
#8150 = CARTESIAN_POINT ( 'NONE',  ( 13.58694672230000045, -100.5229262450000078, -10.01978713429999956 ) ) ;
#8151 = DIRECTION ( 'NONE',  ( 0.000000000000000000, -1.000000000000000000, 0.000000000000000000 ) ) ;
#8152 = CARTESIAN_POINT ( 'NONE',  ( 24.28845093110000164, -92.54030566109999256, -15.30821873470000050 ) ) ;
#8153 = ORIENTED_EDGE ( 'NONE', *, *, #20622, .F. ) ;
#8154 = AXIS2_PLACEMENT_3D ( 'NONE', #17040, #26218, #1741 ) ;
#8155 = CARTESIAN_POINT ( 'NONE',  ( -2.901718461300000218, -80.37804848140000047, 46.68757613950000263 ) ) ;
#8156 = CARTESIAN_POINT ( 'NONE',  ( -18.96815154839999806, -18.50000000000000000, 15.18612143080000010 ) ) ;
#8157 = ORIENTED_EDGE ( 'NONE', *, *, #24133, .F. ) ;
#8158 = ADVANCED_FACE ( 'NONE', ( #14366, #5479 ), #24585, .F. ) ;
#8159 = CARTESIAN_POINT ( 'NONE',  ( -15.03194159329999913, -100.8816813800000034, 4.847769557329999479 ) ) ;
#8160 = CARTESIAN_POINT ( 'NONE',  ( -16.13266937400000245, -83.75000000000000000, -29.53065320760000034 ) ) ;
#8161 = CARTESIAN_POINT ( 'NONE',  ( 38.70686962976383683, -73.76099270142834996, 7.188502612221721932 ) ) ;
#8162 = FACE_OUTER_BOUND ( 'NONE', #23640, .T. ) ;
#8163 = CARTESIAN_POINT ( 'NONE',  ( 23.74158351679999868, -72.51566206409999893, -30.51711889939999978 ) ) ;
#8164 = EDGE_CURVE ( 'NONE', #4271, #18220, #16246, .T. ) ;
#8165 = ORIENTED_EDGE ( 'NONE', *, *, #1947, .F. ) ;
#8166 = CARTESIAN_POINT ( 'NONE',  ( 21.07002592539999952, -35.62472953780000040, -8.346733960690000842 ) ) ;
#8167 = CIRCLE ( 'NONE', #28184, 7.249999999999999112 ) ;
#8168 = EDGE_LOOP ( 'NONE', ( #4070, #15592 ) ) ;
#8169 = DIRECTION ( 'NONE',  ( 0.000000000000000000, -1.000000000000000000, 0.000000000000000000 ) ) ;
#8170 = PLANE ( 'NONE',  #1861 ) ;
#8171 = ORIENTED_EDGE ( 'NONE', *, *, #1141, .F. ) ;
#8172 = CARTESIAN_POINT ( 'NONE',  ( -12.87035238900000067, -101.3256027139999986, -9.347551286109998969 ) ) ;
#8173 = CARTESIAN_POINT ( 'NONE',  ( -15.07852873310000064, -92.61407321170000273, -23.93835657210000178 ) ) ;
#8174 = CARTESIAN_POINT ( 'NONE',  ( -0.5824085402257914712, -18.95847994161702132, -21.90536633182652437 ) ) ;
#8175 = ORIENTED_EDGE ( 'NONE', *, *, #11974, .T. ) ;
#8176 = CARTESIAN_POINT ( 'NONE',  ( -1.271815980439999993, -100.9405338520000015, -15.89396502050000137 ) ) ;
#8177 = CARTESIAN_POINT ( 'NONE',  ( -11.35954001540000036, -77.00000000000000000, 45.25000000000000000 ) ) ;
#8178 = CIRCLE ( 'NONE', #17500, 22.39904313779999612 ) ;
#8179 = CARTESIAN_POINT ( 'NONE',  ( -39.74894630217540481, -65.71742637285102262, 2.207278035994531429 ) ) ;
#8180 = VERTEX_POINT ( 'NONE', #2015 ) ;
#8181 = DIRECTION ( 'NONE',  ( 0.000000000000000000, 1.000000000000000000, 0.000000000000000000 ) ) ;
#8182 = CARTESIAN_POINT ( 'NONE',  ( -37.60355029590000697, -74.00000000000000000, 9.356041104380000917 ) ) ;
#8183 = CARTESIAN_POINT ( 'NONE',  ( 39.40310785678461514, -73.65029154566123282, 7.225850277551550960 ) ) ;
#8184 = ORIENTED_EDGE ( 'NONE', *, *, #6592, .F. ) ;
#8185 = CARTESIAN_POINT ( 'NONE',  ( 19.27348047750000148, -18.62200670700000060, -8.616470594819999107 ) ) ;
#8186 = CARTESIAN_POINT ( 'NONE',  ( -14.66608903329999869, -74.46648494389999939, 36.47374631129999756 ) ) ;
#8187 = CARTESIAN_POINT ( 'NONE',  ( -17.35994848780000055, -93.69758091459999605, 18.14149070599999902 ) ) ;
#8188 = DIRECTION ( 'NONE',  ( 1.000000000000000000, 0.000000000000000000, -1.887379141859999189E-15 ) ) ;
#8189 = VERTEX_POINT ( 'NONE', #8981 ) ;
#8190 = EDGE_CURVE ( 'NONE', #25683, #14668, #18155, .T. ) ;
#8191 = CARTESIAN_POINT ( 'NONE',  ( -11.74592569580000045, -11.00000000000000000, -21.50077276629999901 ) ) ;
#8192 = CARTESIAN_POINT ( 'NONE',  ( 0.04086140067849999835, -101.3852859389999992, -15.99338919589999719 ) ) ;
#8193 = CARTESIAN_POINT ( 'NONE',  ( 9.526335912539998674, -60.27919896120000232, -23.43111588329999861 ) ) ;
#8194 = CARTESIAN_POINT ( 'NONE',  ( -39.59129699350000209, -73.90055525910000256, -7.279149876960000931 ) ) ;
#8195 = CARTESIAN_POINT ( 'NONE',  ( 7.355131038309999703, -34.88462684899999999, -21.34291130700000139 ) ) ;
#8196 = CARTESIAN_POINT ( 'NONE',  ( -10.70711398520000124, -19.40595403629999893, -21.59314527720000143 ) ) ;
#8197 = ORIENTED_EDGE ( 'NONE', *, *, #14848, .T. ) ;
#8198 = EDGE_CURVE ( 'NONE', #17518, #14137, #3691, .T. ) ;
#8199 = CARTESIAN_POINT ( 'NONE',  ( 6.634701928220000156, -100.3517545579999961, 15.38134052770000082 ) ) ;
#8200 = CARTESIAN_POINT ( 'NONE',  ( 15.06296946009999971, -101.0147083550000104, 3.854692841859999941 ) ) ;
#8201 = CARTESIAN_POINT ( 'NONE',  ( -5.909937095737705093, -97.43022994549096438, 19.70649122759998662 ) ) ;
#8202 = CARTESIAN_POINT ( 'NONE',  ( 7.426815359109999903, -35.28814234100000391, -21.34788051319999980 ) ) ;
#8203 = CARTESIAN_POINT ( 'NONE',  ( 21.47791241899999903, -36.56811125080000835, -7.356933755090000027 ) ) ;
#8204 = CARTESIAN_POINT ( 'NONE',  ( -13.48313256510000002, -64.78279493179998383, 21.61455522920000050 ) ) ;
#8205 = EDGE_LOOP ( 'NONE', ( #26928, #21662, #25226 ) ) ;
#8206 = CARTESIAN_POINT ( 'NONE',  ( 3.339696405680000257, -92.65997669530000280, -28.81024678410000206 ) ) ;
#8207 = ADVANCED_FACE ( 'NONE', ( #6520 ), #19766, .F. ) ;
#8208 = CARTESIAN_POINT ( 'NONE',  ( -32.75000000000000000, -69.50000000000000000, 6.890159016250000695E-16 ) ) ;
#8209 = DIRECTION ( 'NONE',  ( -0.5000000000009400258, 0.000000000000000000, -0.8660254037838960306 ) ) ;
#8210 = ORIENTED_EDGE ( 'NONE', *, *, #16324, .F. ) ;
#8211 = DIRECTION ( 'NONE',  ( -0.01257738078990017563, -0.9996558222130138560, -0.02302274110720029660 ) ) ;
#8212 = PLANE ( 'NONE',  #5061 ) ;
#8213 = ORIENTED_EDGE ( 'NONE', *, *, #17200, .T. ) ;
#8214 = CARTESIAN_POINT ( 'NONE',  ( -1.469243280769999993, -101.0356131030000029, -15.40539586329999899 ) ) ;
#8215 = CARTESIAN_POINT ( 'NONE',  ( -7.135466578850000019, -73.50000064450000536, 38.71640869449999656 ) ) ;
#8216 = CARTESIAN_POINT ( 'NONE',  ( 36.40080305694491614, -74.58594345823078697, -14.77956079794565980 ) ) ;
#8217 = CARTESIAN_POINT ( 'NONE',  ( 23.56306528260000022, -73.81141447500000652, -31.03614770169999915 ) ) ;
#8218 = EDGE_CURVE ( 'NONE', #4593, #6398, #2157, .T. ) ;
#8219 = CARTESIAN_POINT ( 'NONE',  ( -22.71590082970000068, -71.15593401950000896, 16.24045227410000081 ) ) ;
#8220 = CARTESIAN_POINT ( 'NONE',  ( -15.33274302073847828, -101.3256032149999299, 4.234343774312764985 ) ) ;
#8221 = CARTESIAN_POINT ( 'NONE',  ( -19.41155612407374420, -19.49371746088979762, 14.25750765975674739 ) ) ;
#8222 = CARTESIAN_POINT ( 'NONE',  ( 6.850353628289999719, -36.56979901409999911, -21.56931449510000220 ) ) ;
#8223 = DIRECTION ( 'NONE',  ( 1.000000000000000000, 0.000000000000000000, 0.000000000000000000 ) ) ;
#8224 = EDGE_LOOP ( 'NONE', ( #18461, #14100 ) ) ;
#8225 = CARTESIAN_POINT ( 'NONE',  ( -10.93437490840835480, -19.23820060856186487, -21.85842320415198614 ) ) ;
#8226 = ORIENTED_EDGE ( 'NONE', *, *, #1571, .F. ) ;
#8227 = CARTESIAN_POINT ( 'NONE',  ( 22.39433382880000067, -37.06245928150000424, -9.379298933899999469 ) ) ;
#8228 = CARTESIAN_POINT ( 'NONE',  ( -2.565688225440000192, -58.62494694620000502, -24.98236248359999934 ) ) ;
#8229 = CARTESIAN_POINT ( 'NONE',  ( 9.379298533759998335, -37.06245930440000080, -22.39433306820000169 ) ) ;
#8230 = FACE_OUTER_BOUND ( 'NONE', #12781, .T. ) ;
#8231 = CARTESIAN_POINT ( 'NONE',  ( -0.6842253573819999657, -101.2530993000000024, -15.17849927279999989 ) ) ;
#8232 = DIRECTION ( 'NONE',  ( 1.000000000000000000, 0.000000000000000000, 0.000000000000000000 ) ) ;
#8233 = ADVANCED_FACE ( 'NONE', ( #23999 ), #24290, .F. ) ;
#8234 = CARTESIAN_POINT ( 'NONE',  ( 15.93242396329999977, -100.7430069139999915, 4.261870627000000411 ) ) ;
#8235 = CARTESIAN_POINT ( 'NONE',  ( 21.48235967180000117, -35.71220925649999600, -7.023816322830000125 ) ) ;
#8236 = VECTOR ( 'NONE', #3648, 1000.000000000000000 ) ;
#8237 = CARTESIAN_POINT ( 'NONE',  ( -13.85848666890000125, -57.40875702409999803, 21.24403892489999990 ) ) ;
#8238 = ORIENTED_EDGE ( 'NONE', *, *, #13476, .T. ) ;
#8239 = CARTESIAN_POINT ( 'NONE',  ( 26.77683864449999973, -19.40000000000000213, 49.01467436490000296 ) ) ;
#8240 = VERTEX_POINT ( 'NONE', #10855 ) ;
#8241 = EDGE_CURVE ( 'NONE', #20661, #13365, #2299, .T. ) ;
#8242 = CARTESIAN_POINT ( 'NONE',  ( -7.441474466189999859, -94.70873790539999959, -22.49465953780000049 ) ) ;
#8243 = AXIS2_PLACEMENT_3D ( 'NONE', #17246, #19427, #19154 ) ;
#8244 = CARTESIAN_POINT ( 'NONE',  ( -14.81560312829999937, -101.2530993080000030, 3.374019817609999805 ) ) ;
#8245 = CARTESIAN_POINT ( 'NONE',  ( -32.19741970148672294, -74.02576585426132283, -22.07384625748134255 ) ) ;
#8246 = CARTESIAN_POINT ( 'NONE',  ( 40.50000000000000000, -15.00000000000000000, 4.500000000000000000 ) ) ;
#8247 = ORIENTED_EDGE ( 'NONE', *, *, #9030, .F. ) ;
#8248 = CARTESIAN_POINT ( 'NONE',  ( 17.74427621692063894, -100.1470170784672149, 1.201385877241859967 ) ) ;
#8249 = CARTESIAN_POINT ( 'NONE',  ( -12.45064030709999869, -101.3090757639999993, -10.46249930100000114 ) ) ;
#8250 = CARTESIAN_POINT ( 'NONE',  ( 20.34398966297630196, -93.66270333196790432, 16.17952385861759979 ) ) ;
#8251 = CARTESIAN_POINT ( 'NONE',  ( -6.858401400031342909, -101.6484611539999747, 14.45577953271265059 ) ) ;
#8252 = ORIENTED_EDGE ( 'NONE', *, *, #24639, .T. ) ;
#8253 = DIRECTION ( 'NONE',  ( 0.000000000000000000, 1.000000000000000000, 0.000000000000000000 ) ) ;
#8254 = CARTESIAN_POINT ( 'NONE',  ( -1.865174681369999824E-14, -15.00000000000000000, 31.00000000000000000 ) ) ;
#8255 = ORIENTED_EDGE ( 'NONE', *, *, #19373, .F. ) ;
#8256 = B_SPLINE_SURFACE_WITH_KNOTS ( 'NONE', 5, 5, ( 
 ( #20943, #15185, #26441, #16983, #8509, #26304 ),
 ( #12440, #28471, #15335, #15054, #8646, #12858 ),
 ( #13012, #24252, #26004, #5897, #14775, #3997 ),
 ( #6181, #21495, #23676, #12724, #3720, #10393 ),
 ( #23964, #1686, #21776, #1551, #21636, #28328 ),
 ( #1827, #10670, #26157, #12580, #19167, #8222 ) ),
 .UNSPECIFIED., .F., .F., .F.,
 ( 6, 6 ),
 ( 6, 6 ),
 ( 7.598609845240000382, 9.882010082849999932 ),
 ( 1.678547873260000101, 2.000000000000000000 ),
 .UNSPECIFIED. ) ;
#8257 = DIRECTION ( 'NONE',  ( -1.000000000000000000, 0.000000000000000000, -7.486357007659997978E-17 ) ) ;
#8258 = CARTESIAN_POINT ( 'NONE',  ( -1.559612570125768594, -80.07450989126839147, 47.08089326071244329 ) ) ;
#8259 = ORIENTED_EDGE ( 'NONE', *, *, #21359, .T. ) ;
#8260 = CIRCLE ( 'NONE', #7825, 7.249999999999999112 ) ;
#8261 = CARTESIAN_POINT ( 'NONE',  ( 47.25003036660000788, -74.81280582019999770, -0.5683001369479999676 ) ) ;
#8262 = CONICAL_SURFACE ( 'NONE', #24570, 11.99999999999999822, 0.02623728384790100648 ) ;
#8263 = ORIENTED_EDGE ( 'NONE', *, *, #19373, .T. ) ;
#8264 = CARTESIAN_POINT ( 'NONE',  ( 20.73443730799999685, -53.84184168659999870, 10.63482208240000126 ) ) ;
#8265 = CARTESIAN_POINT ( 'NONE',  ( -38.38202296894133525, -63.05366661936223949, 2.876041293754835859 ) ) ;
#8266 = ORIENTED_EDGE ( 'NONE', *, *, #5285, .T. ) ;
#8267 = DIRECTION ( 'NONE',  ( 0.000000000000000000, 1.000000000000000000, 0.000000000000000000 ) ) ;
#8268 = CARTESIAN_POINT ( 'NONE',  ( 33.25000000000000000, -69.00000000000000000, -2.691640454479999860E-15 ) ) ;
#8269 = ADVANCED_FACE ( 'NONE', ( #15377 ), #21953, .F. ) ;
#8270 = CARTESIAN_POINT ( 'NONE',  ( 10.33698648600000070, -72.00000000000000000, -28.69894938910000093 ) ) ;
#8271 = EDGE_CURVE ( 'NONE', #8526, #4628, #721, .T. ) ;
#8272 = CARTESIAN_POINT ( 'NONE',  ( 21.75659477429999811, -93.00000000000000000, -13.30039788230000042 ) ) ;
#8273 = CARTESIAN_POINT ( 'NONE',  ( -0.6409979960822642653, -79.61491260298355144, 47.25010901152391796 ) ) ;
#8274 = ORIENTED_EDGE ( 'NONE', *, *, #18840, .T. ) ;
#8275 = EDGE_CURVE ( 'NONE', #12701, #18300, #26498, .T. ) ;
#8276 = CARTESIAN_POINT ( 'NONE',  ( -14.99536030859999869, -98.58303758080000989, -11.15547849020000015 ) ) ;
#8277 = CARTESIAN_POINT ( 'NONE',  ( 13.21950097729999918, -100.5027207520000019, -9.453354134850000534 ) ) ;
#8278 = CARTESIAN_POINT ( 'NONE',  ( -19.58495966999999993, -92.85282696620001275, 20.69528026369999907 ) ) ;
#8279 = CARTESIAN_POINT ( 'NONE',  ( 24.70831025289999872, -92.79907188629998416, -15.37124366699999989 ) ) ;
#8280 = CARTESIAN_POINT ( 'NONE',  ( -1.158253037809999997, -52.63055504209999924, -23.23212522879999753 ) ) ;
#8281 = CARTESIAN_POINT ( 'NONE',  ( 10.09279242184272718, -72.75205755911096617, -26.86115544024559298 ) ) ;
#8282 = CARTESIAN_POINT ( 'NONE',  ( -12.07243358760000085, -67.46050599719998786, -24.77970463289999969 ) ) ;
#8283 = VERTEX_POINT ( 'NONE', #18329 ) ;
#8284 = CIRCLE ( 'NONE', #16667, 5.000000000000000888 ) ;
#8285 = DIRECTION ( 'NONE',  ( 0.000000000000000000, 1.000000000000000000, 0.000000000000000000 ) ) ;
#8286 = DIRECTION ( 'NONE',  ( 0.4794255386042040046, 0.000000000000000000, 0.8775825618903722036 ) ) ;
#8287 = DIRECTION ( 'NONE',  ( 1.000000000000000000, 0.000000000000000000, 0.000000000000000000 ) ) ;
#8288 = CARTESIAN_POINT ( 'NONE',  ( 18.69415571529999909, -18.50000000000000000, 9.686494650060000211 ) ) ;
#8289 = CARTESIAN_POINT ( 'NONE',  ( -17.13033212710000086, -72.00000000000000000, 23.49748962700000021 ) ) ;
#8290 = B_SPLINE_CURVE_WITH_KNOTS ( 'NONE', 3,
 ( #21952, #1999, #10841, #19750, #10281, #9406, #22545, #20199, #18315, #24868, #2728, #13637, #272, #27059, #24568, #9114, #26772, #22392, #27203, #11583, #13191, #17730, #7243, #7101, #15964, #16108, #26913, #6804, #19895, #17873, #18160, #26613, #6653, #2287, #2589, #15815, #4902, #22099, #25008, #15665, #2142, #18014, #8814, #24727, #13484, #15516, #6953, #20052, #115, #4761, #11436, #10979 ),
 .UNSPECIFIED., .F., .F.,
 ( 4, 2, 2, 1, 1, 1, 1, 2, 2, 2, 2, 1, 1, 1, 1, 1, 2, 2, 2, 2, 1, 1, 2, 2, 2, 2, 1, 1, 1, 1, 1, 2, 2, 4 ),
 ( 0.000000000000000000, 0.1249999999999993339, 0.1874999999999988343, 0.2187499999999984457, 0.2343749999999982514, 0.2421874999999974742, 0.2460937499999971967, 0.2480468749999965861, 0.2499999999999960032, 0.3750000000000502931, 0.4375000000000773270, 0.4687500000000909273, 0.4843750000000984213, 0.4921875000001021405, 0.4960937500001039724, 0.4980468750001043055, 0.4990234375001045275, 0.5000000000001048051, 0.5625000000001960654, 0.5937500000002408074, 0.6093750000002631229, 0.6171875000002737810, 0.6210937500002799982, 0.6250000000002862155, 0.6875000000003996803, 0.7187500000004555245, 0.7343750000004828360, 0.7421875000004953815, 0.7460937500005029310, 0.7480468750005067058, 0.7490234375005088152, 0.7495117187505085932, 0.7500000000005083711, 1.000000000000000000 ),
 .UNSPECIFIED. ) ;
#8291 = ORIENTED_EDGE ( 'NONE', *, *, #8119, .F. ) ;
#8292 = DIRECTION ( 'NONE',  ( 0.000000000000000000, -1.000000000000000000, 0.000000000000000000 ) ) ;
#8293 = DIRECTION ( 'NONE',  ( 0.000000000000000000, 1.000000000000000000, 0.000000000000000000 ) ) ;
#8294 = EDGE_LOOP ( 'NONE', ( #9467, #16781, #23269, #25085 ) ) ;
#8295 = CARTESIAN_POINT ( 'NONE',  ( 21.31878868039999730, -36.49872739439999947, -8.228180139540000937 ) ) ;
#8296 = CARTESIAN_POINT ( 'NONE',  ( 9.079731074819999748, -35.79879667440000190, -19.54912311329999852 ) ) ;
#8297 = ORIENTED_EDGE ( 'NONE', *, *, #13150, .T. ) ;
#8298 = CARTESIAN_POINT ( 'NONE',  ( -12.73176082490000027, -101.1045726949999874, -8.901570339680000998 ) ) ;
#8300 = EDGE_CURVE ( 'NONE', #14853, #2130, #6487, .T. ) ;
#8299 = AXIS2_PLACEMENT_3D ( 'NONE', #19023, #25997, #10248 ) ;
#8301 = CIRCLE ( 'NONE', #5976, 38.75000000000000000 ) ;
#8302 = CARTESIAN_POINT ( 'NONE',  ( -13.18688158500000007, -93.32822950609998713, -23.58441611189999776 ) ) ;
#8303 = CARTESIAN_POINT ( 'NONE',  ( -2.743624554930000237, -99.80676450699999691, -17.57271110129999769 ) ) ;
#8304 = CARTESIAN_POINT ( 'NONE',  ( 7.633405283620000148, -53.29445792060000286, -21.99751943120000064 ) ) ;
#8305 = DIRECTION ( 'NONE',  ( 0.8960873909912637769, 0.000000000000000000, -0.4438776720071309079 ) ) ;
#8306 = VERTEX_POINT ( 'NONE', #18473 ) ;
#8307 = EDGE_CURVE ( 'NONE', #7391, #11754, #3710, .T. ) ;
#8308 = CARTESIAN_POINT ( 'NONE',  ( 13.11884685345288304, -101.1451610291512964, -9.826322704137346875 ) ) ;
#8309 = CARTESIAN_POINT ( 'NONE',  ( -21.19242592198007813, -64.57498915307851917, 13.11476673155585360 ) ) ;
#8310 = CARTESIAN_POINT ( 'NONE',  ( 0.000000000000000000, -15.49681045920000066, 0.000000000000000000 ) ) ;
#8311 = DIRECTION ( 'NONE',  ( 0.000000000000000000, 1.000000000000000000, 0.000000000000000000 ) ) ;
#8312 = EDGE_LOOP ( 'NONE', ( #25904, #11385, #9181, #6352 ) ) ;
#8313 = FACE_OUTER_BOUND ( 'NONE', #1689, .T. ) ;
#8314 = DIRECTION ( 'NONE',  ( 0.8775825618903719816, 0.000000000000000000, 0.4794255386042042821 ) ) ;
#8315 = CARTESIAN_POINT ( 'NONE',  ( -17.63662161710000120, -94.54718950359999496, 16.06392408140000327 ) ) ;
#8316 = DIRECTION ( 'NONE',  ( -0.9206947212159483085, 0.000000000000000000, 0.3902835255619780952 ) ) ;
#8317 = ORIENTED_EDGE ( 'NONE', *, *, #3212, .T. ) ;
#8318 = CARTESIAN_POINT ( 'NONE',  ( -1.317572430653283666, -74.17424845055897720, 47.12932669921157469 ) ) ;
#8319 = CIRCLE ( 'NONE', #14826, 2.000000000000001776 ) ;
#8320 = CARTESIAN_POINT ( 'NONE',  ( 10.20110288159999890, -84.00000000000000000, -41.00000000000000000 ) ) ;
#8321 = CARTESIAN_POINT ( 'NONE',  ( 8.029264327879999996, -63.60161137440000090, -23.19827344629999999 ) ) ;
#8322 = CARTESIAN_POINT ( 'NONE',  ( 15.81703362330000040, -101.6095085860000040, 2.604458381759999774 ) ) ;
#8323 = CARTESIAN_POINT ( 'NONE',  ( 22.26607236109999732, -57.85578495419999712, 10.13866405869999987 ) ) ;
#8324 = FACE_OUTER_BOUND ( 'NONE', #26506, .T. ) ;
#8325 = ORIENTED_EDGE ( 'NONE', *, *, #18579, .F. ) ;
#8326 = AXIS2_PLACEMENT_3D ( 'NONE', #9904, #18948, #3365 ) ;
#8327 = AXIS2_PLACEMENT_3D ( 'NONE', #13454, #20012, #4432 ) ;
#8328 = CARTESIAN_POINT ( 'NONE',  ( 6.018657797749999538, -100.4792519539999915, 15.03391506150000012 ) ) ;
#8329 = CARTESIAN_POINT ( 'NONE',  ( 15.62063516470000124, -101.5369810359999860, 3.464403400670000188 ) ) ;
#8330 = DIRECTION ( 'NONE',  ( 0.000000000000000000, 1.000000000000000000, 0.000000000000000000 ) ) ;
#8331 = CARTESIAN_POINT ( 'NONE',  ( 6.258798239620000814, -92.50000000000000000, -29.85092033080000107 ) ) ;
#8332 = ADVANCED_FACE ( 'NONE', ( #15977 ), #22995, .T. ) ;
#8333 = CARTESIAN_POINT ( 'NONE',  ( -42.06430546961426842, -65.70894168417346748, -0.8597717761772040168 ) ) ;
#8334 = ORIENTED_EDGE ( 'NONE', *, *, #5188, .F. ) ;
#8335 = CARTESIAN_POINT ( 'NONE',  ( 8.074823624729997817, -93.81709628030000658, -24.47602660240000105 ) ) ;
#8336 = EDGE_CURVE ( 'NONE', #23975, #25484, #28358, .T. ) ;
#8337 = CARTESIAN_POINT ( 'NONE',  ( 19.80394448450000056, -31.61664686670000179, -8.966802299960001221 ) ) ;
#8338 = CARTESIAN_POINT ( 'NONE',  ( -6.807494426549999922, -101.1617736559999940, 14.19398353890000131 ) ) ;
#8339 = ORIENTED_EDGE ( 'NONE', *, *, #6852, .T. ) ;
#8340 = SURFACE_SIDE_STYLE ('',( #16392 ) ) ;
#8341 = EDGE_CURVE ( 'NONE', #21937, #767, #25744, .T. ) ;
#8342 = CARTESIAN_POINT ( 'NONE',  ( -12.60783569927363601, -100.8738282927339043, -10.80472408861342437 ) ) ;
#8343 = ORIENTED_EDGE ( 'NONE', *, *, #8798, .T. ) ;
#8344 = CARTESIAN_POINT ( 'NONE',  ( -10.50000000000000000, -18.50000000000000000, 0.000000000000000000 ) ) ;
#8345 = ORIENTED_EDGE ( 'NONE', *, *, #8900, .F. ) ;
#8346 = AXIS2_PLACEMENT_3D ( 'NONE', #14656, #21096, #23828 ) ;
#8347 = ADVANCED_FACE ( 'NONE', ( #18905 ), #16703, .T. ) ;
#8348 = AXIS2_PLACEMENT_3D ( 'NONE', #22949, #23364, #3407 ) ;
#8349 = CARTESIAN_POINT ( 'NONE',  ( -1.137727369580000092, -101.2490009469999990, -16.04170511839999946 ) ) ;
#8350 = CARTESIAN_POINT ( 'NONE',  ( 22.08965024500000141, -19.46434222019999893, 0.09551833593859999916 ) ) ;
#8351 = DIRECTION ( 'NONE',  ( 0.000000000000000000, -1.000000000000000000, 0.000000000000000000 ) ) ;
#8352 = CARTESIAN_POINT ( 'NONE',  ( 13.12517053680000068, -93.00000000000000000, 27.53143473160000099 ) ) ;
#8353 = CARTESIAN_POINT ( 'NONE',  ( 16.25687204636146177, -94.67499508575106404, 17.23253240788842078 ) ) ;
#8354 = CARTESIAN_POINT ( 'NONE',  ( -22.65531121069999898, -72.00000193540000737, 18.22956418530000278 ) ) ;
#8355 = DIRECTION ( 'NONE',  ( 0.000000000000000000, -1.000000000000000000, 0.000000000000000000 ) ) ;
#8356 = CARTESIAN_POINT ( 'NONE',  ( -19.18665701145497238, -19.48886652642410056, 14.08555375221862427 ) ) ;
#8357 = CARTESIAN_POINT ( 'NONE',  ( 24.32621394512662860, -94.00303307109788875, -9.416846555509286176 ) ) ;
#8358 = CARTESIAN_POINT ( 'NONE',  ( -10.70759194130000047, -18.50000000000000000, 18.17968849400000053 ) ) ;
#8359 = ORIENTED_EDGE ( 'NONE', *, *, #16774, .F. ) ;
#8360 = DIRECTION ( 'NONE',  ( 0.000000000000000000, 1.000000000000000000, 0.000000000000000000 ) ) ;
#8361 = ORIENTED_EDGE ( 'NONE', *, *, #23213, .F. ) ;
#8362 = CARTESIAN_POINT ( 'NONE',  ( 22.27253482889999958, -37.66179417780000449, -9.067412436450000612 ) ) ;
#8363 = VECTOR ( 'NONE', #8712, 1000.000000000000000 ) ;
#8364 = AXIS2_PLACEMENT_3D ( 'NONE', #22633, #13734, #24958 ) ;
#8365 = VERTEX_POINT ( 'NONE', #28197 ) ;
#8366 = CARTESIAN_POINT ( 'NONE',  ( -1.966302623820000095, -61.72813301749999937, -24.36653853009999793 ) ) ;
#8367 = CARTESIAN_POINT ( 'NONE',  ( 16.83483077069999823, -111.0000000000000000, 4.239603657359999112 ) ) ;
#8368 = DIRECTION ( 'NONE',  ( -0.8830706733883036952, -0.000000000000000000, -0.4692400087391608854 ) ) ;
#8369 = FACE_OUTER_BOUND ( 'NONE', #6079, .T. ) ;
#8370 = EDGE_CURVE ( 'NONE', #26269, #23532, #13467, .T. ) ;
#8371 = ADVANCED_FACE ( 'NONE', ( #14515 ), #12449, .T. ) ;
#8372 = ORIENTED_EDGE ( 'NONE', *, *, #16533, .T. ) ;
#8373 = DIRECTION ( 'NONE',  ( 0.000000000000000000, 1.000000000000000000, 0.000000000000000000 ) ) ;
#8374 = CARTESIAN_POINT ( 'NONE',  ( 27.89292634430000106, -74.00000000000000000, 12.34776042340000046 ) ) ;
#8375 = ORIENTED_EDGE ( 'NONE', *, *, #14196, .F. ) ;
#8376 = CARTESIAN_POINT ( 'NONE',  ( 0.000000000000000000, -65.07443093669999712, 0.000000000000000000 ) ) ;
#8377 = AXIS2_PLACEMENT_3D ( 'NONE', #4808, #162, #9015 ) ;
#8378 = CARTESIAN_POINT ( 'NONE',  ( -22.15114526100514070, -74.12004522895882985, -32.51295459047183556 ) ) ;
#8379 = TOROIDAL_SURFACE ( 'NONE', #17239, 7.750000000000000000, 0.5000000000000000000 ) ;
#8380 = VECTOR ( 'NONE', #23162, 1000.000000000000000 ) ;
#8381 = CARTESIAN_POINT ( 'NONE',  ( 22.35420147799999668, -19.18584080579999807, 9.881343264190000752 ) ) ;
#8382 = DIRECTION ( 'NONE',  ( -6.123031769109999188E-17, 0.000000000000000000, 1.000000000000000000 ) ) ;
#8383 = CARTESIAN_POINT ( 'NONE',  ( -19.69730263860000008, -58.97490961110000285, 13.65699954170000119 ) ) ;
#8384 = VERTEX_POINT ( 'NONE', #16990 ) ;
#8385 = FACE_OUTER_BOUND ( 'NONE', #17034, .T. ) ;
#8386 = CARTESIAN_POINT ( 'NONE',  ( -12.05323405150000049, -101.1848541609999899, -9.394733094839999410 ) ) ;
#8387 =( NAMED_UNIT ( * ) SI_UNIT ( $, .STERADIAN. ) SOLID_ANGLE_UNIT ( ) );
#8388 = CARTESIAN_POINT ( 'NONE',  ( -7.679059309326275340, -100.9616911410546578, 14.64373627150416546 ) ) ;
#8389 = VERTEX_POINT ( 'NONE', #3731 ) ;
#8390 = EDGE_CURVE ( 'NONE', #14401, #18033, #27902, .T. ) ;
#8391 = DIRECTION ( 'NONE',  ( 0.000000000000000000, 1.000000000000000000, 0.000000000000000000 ) ) ;
#8392 = CARTESIAN_POINT ( 'NONE',  ( -32.60339417960000219, -74.26163306789999297, -21.76180095249999980 ) ) ;
#8393 = CARTESIAN_POINT ( 'NONE',  ( 37.00134709710000180, -80.06168491079999683, -13.64132839650000051 ) ) ;
#8394 = ORIENTED_EDGE ( 'NONE', *, *, #15047, .T. ) ;
#8395 = CARTESIAN_POINT ( 'NONE',  ( 6.668334764284620242, -100.8945630386159706, 15.18849496292583545 ) ) ;
#8396 = AXIS2_PLACEMENT_3D ( 'NONE', #227, #9074, #1233 ) ;
#8397 = LINE ( 'NONE', #1868, #25960 ) ;
#8398 = CIRCLE ( 'NONE', #24722, 0.5000000000000027756 ) ;
#8399 = ORIENTED_EDGE ( 'NONE', *, *, #17596, .T. ) ;
#8400 = CIRCLE ( 'NONE', #28421, 0.5000000000000004441 ) ;
#8401 = FACE_OUTER_BOUND ( 'NONE', #21697, .T. ) ;
#8402 = ORIENTED_EDGE ( 'NONE', *, *, #11420, .T. ) ;
#8403 = CARTESIAN_POINT ( 'NONE',  ( 22.54171623719999928, -56.21886023140000077, 10.13951573499999981 ) ) ;
#8404 = CARTESIAN_POINT ( 'NONE',  ( 1.678657213230000024E-14, -74.00000000000000000, 7.838174553849999450E-15 ) ) ;
#8405 = AXIS2_PLACEMENT_3D ( 'NONE', #22541, #15661, #21949 ) ;
#8406 = CARTESIAN_POINT ( 'NONE',  ( 8.074115162410000934, -92.66424957140000629, 26.74225754210000261 ) ) ;
#8407 = VERTEX_POINT ( 'NONE', #21362 ) ;
#8408 = CARTESIAN_POINT ( 'NONE',  ( -6.860733622652498198, -95.36087494180328861, -22.20122310548567057 ) ) ;
#8409 = CARTESIAN_POINT ( 'NONE',  ( 19.52063838700000176, -35.55398684600000081, -8.985157197580001309 ) ) ;
#8410 = CARTESIAN_POINT ( 'NONE',  ( -29.91144828099999842, -92.50000000000000000, -0.6532076026720000650 ) ) ;
#8411 = CARTESIAN_POINT ( 'NONE',  ( -18.86782185830000103, -92.76550115769998683, -21.02010845870000111 ) ) ;
#8412 = CARTESIAN_POINT ( 'NONE',  ( 24.46803346076760732, -64.99740952387834625, 10.81838244473379440 ) ) ;
#8413 = EDGE_LOOP ( 'NONE', ( #19457, #1737, #3015, #25741 ) ) ;
#8414 = CARTESIAN_POINT ( 'NONE',  ( -18.73266888770000094, -96.73974214399999028, -10.02540521279999908 ) ) ;
#8415 = VECTOR ( 'NONE', #14354, 1000.000000000000000 ) ;
#8416 = CARTESIAN_POINT ( 'NONE',  ( 13.70361515709999978, -100.3063911739999980, -10.15418389529999921 ) ) ;
#8417 = CARTESIAN_POINT ( 'NONE',  ( 23.40870142566227585, -59.03921358009447573, -0.5708395527905374411 ) ) ;
#8418 = ORIENTED_EDGE ( 'NONE', *, *, #24879, .T. ) ;
#8419 = B_SPLINE_CURVE_WITH_KNOTS ( 'NONE', 3,
 ( #23460, #12358, #16897, #3633, #2310, #294, #11161, #26796, #4191, #11003 ),
 .UNSPECIFIED., .F., .F.,
 ( 4, 2, 2, 2, 4 ),
 ( 0.000000000000000000, 0.2500000000000000000, 0.5000000000000000000, 0.7500000000000000000, 1.000000000000000000 ),
 .UNSPECIFIED. ) ;
#8420 = CIRCLE ( 'NONE', #7545, 1.000000000000000888 ) ;
#8421 = LINE ( 'NONE', #19787, #7667 ) ;
#8422 = CARTESIAN_POINT ( 'NONE',  ( -19.35716650769999703, -18.50000000000000000, 15.34467347940000082 ) ) ;
#8423 = ORIENTED_EDGE ( 'NONE', *, *, #8300, .T. ) ;
#8424 = AXIS2_PLACEMENT_3D ( 'NONE', #26048, #28516, #23863 ) ;
#8425 = DIRECTION ( 'NONE',  ( 0.000000000000000000, -1.000000000000000000, 0.000000000000000000 ) ) ;
#8426 = B_SPLINE_CURVE_WITH_KNOTS ( 'NONE', 3,
 ( #5180, #23384, #12151, #14352, #14063, #23246, #3427, #27482 ),
 .UNSPECIFIED., .F., .F.,
 ( 4, 2, 2, 4 ),
 ( 0.000000000000000000, 0.4999999999999998890, 0.7499999999999998890, 1.000000000000000000 ),
 .UNSPECIFIED. ) ;
#8427 = EDGE_CURVE ( 'NONE', #2153, #2039, #4639, .T. ) ;
#8428 = CARTESIAN_POINT ( 'NONE',  ( -38.25000000000000000, -63.07912966450000880, 2.684678751729999480 ) ) ;
#8429 = CARTESIAN_POINT ( 'NONE',  ( 22.71044028429788852, -95.75133629245080158, -1.098555083257358289 ) ) ;
#8430 = DIRECTION ( 'NONE',  ( 1.000000000000000000, 0.000000000000000000, 0.000000000000000000 ) ) ;
#8431 = CARTESIAN_POINT ( 'NONE',  ( -0.3395873122069730243, -92.62938374248859930, -30.49812602705775078 ) ) ;
#8432 = DIRECTION ( 'NONE',  ( 0.000000000000000000, 1.000000000000000000, 0.000000000000000000 ) ) ;
#8433 = ADVANCED_FACE ( 'NONE', ( #8230 ), #16157, .T. ) ;
#8434 = B_SPLINE_SURFACE_WITH_KNOTS ( 'NONE', 5, 5, ( 
 ( #18423, #22951, #820, #27313, #18570, #2839, #22798, #13751, #2990 ),
 ( #18860, #9662, #20762, #27461, #14198, #24975, #7353, #671, #22651 ),
 ( #1107, #7510, #13895, #25283, #16216, #25130, #2692, #18716, #11698 ),
 ( #27615, #5449, #16655, #16371, #5163, #14044, #23092, #23226, #3135 ),
 ( #11989, #20902, #968, #3274, #11549, #9806, #12131, #9945, #27745 ),
 ( #7782, #5858, #7918, #21456, #12402, #21314, #17073, #5991, #28429 ) ),
 .UNSPECIFIED., .F., .F., .F.,
 ( 6, 6 ),
 ( 6, 3, 6 ),
 ( 0.000000000000000000, 46.92994236210000025 ),
 ( 0.000000000000000000, 1.000000000000000000, 2.000000000000000000 ),
 .UNSPECIFIED. ) ;
#8435 = EDGE_CURVE ( 'NONE', #24426, #19799, #10190, .T. ) ;
#8436 = EDGE_CURVE ( 'NONE', #19835, #3921, #16733, .T. ) ;
#8437 = ORIENTED_EDGE ( 'NONE', *, *, #25122, .T. ) ;
#8438 = CARTESIAN_POINT ( 'NONE',  ( -39.81550290757894572, -73.86170940550850617, -7.247654292443082014 ) ) ;
#8439 = VERTEX_POINT ( 'NONE', #12866 ) ;
#8440 = VECTOR ( 'NONE', #10338, 1000.000000000000000 ) ;
#8441 = CARTESIAN_POINT ( 'NONE',  ( 20.14644966349999677, -35.79581201140000246, -8.987973295479999791 ) ) ;
#8442 = CARTESIAN_POINT ( 'NONE',  ( -35.88566914520000495, -74.00000000000000000, -26.69328098980000163 ) ) ;
#8443 = ORIENTED_EDGE ( 'NONE', *, *, #20569, .T. ) ;
#8444 = CIRCLE ( 'NONE', #22906, 9.000000000000000000 ) ;
#8445 = CARTESIAN_POINT ( 'NONE',  ( -13.08734813130000063, -101.2459394079999981, -9.124757622539998891 ) ) ;
#8446 = PLANE ( 'NONE',  #7934 ) ;
#8447 = EDGE_LOOP ( 'NONE', ( #9986, #1508, #23940, #6403 ) ) ;
#8448 = CARTESIAN_POINT ( 'NONE',  ( -0.07556308132799999244, -93.13207089459999111, 26.24589193079999916 ) ) ;
#8449 = CARTESIAN_POINT ( 'NONE',  ( -30.34790777679999962, -93.00000000000000000, 3.042119914239999723 ) ) ;
#8450 = CARTESIAN_POINT ( 'NONE',  ( -43.20000000000000284, -63.07912966450000880, -0.1732050807570000017 ) ) ;
#8451 = CARTESIAN_POINT ( 'NONE',  ( -29.62058833974716165, -92.58608763742402914, 7.271233193961131214 ) ) ;
#8452 = DIRECTION ( 'NONE',  ( 0.000000000000000000, 1.000000000000000000, 0.000000000000000000 ) ) ;
#8453 = VERTEX_POINT ( 'NONE', #8367 ) ;
#8454 = CARTESIAN_POINT ( 'NONE',  ( 13.07944802186373856, -101.1884902309573704, -9.822393493178296353 ) ) ;
#8455 = CARTESIAN_POINT ( 'NONE',  ( 23.42789372030000195, -57.47571039170000518, 0.04069560979510000037 ) ) ;
#8456 = CARTESIAN_POINT ( 'NONE',  ( 22.66044434279999820, -66.11532834579999474, 11.96275783630000156 ) ) ;
#8457 = CARTESIAN_POINT ( 'NONE',  ( 7.073120017670000870, -99.73367811500000357, 15.79835279589999963 ) ) ;
#8458 = ORIENTED_EDGE ( 'NONE', *, *, #6512, .F. ) ;
#8459 = CARTESIAN_POINT ( 'NONE',  ( 47.16974535660000356, -74.50000000000000000, -1.075756255579999987 ) ) ;
#8460 = CARTESIAN_POINT ( 'NONE',  ( 4.882943008269999509E-15, -73.00000000000000000, -40.00000000000000000 ) ) ;
#8461 = CARTESIAN_POINT ( 'NONE',  ( -41.75000000000000000, -63.07912966450000880, -2.684678751739999925 ) ) ;
#8462 = CARTESIAN_POINT ( 'NONE',  ( -20.43932202180000246, -94.59276292389999696, 12.18704577789999988 ) ) ;
#8463 = EDGE_LOOP ( 'NONE', ( #20502, #16023, #24854, #2061 ) ) ;
#8464 = CARTESIAN_POINT ( 'NONE',  ( 27.39441059460000361, -70.03171919160000414, 1.011203377119999969 ) ) ;
#8465 = B_SPLINE_CURVE_WITH_KNOTS ( 'NONE', 5,
 ( #22040, #8751, #22183, #22325, #11227, #10928, #17669, #19833, #11064 ),
 .UNSPECIFIED., .F., .F.,
 ( 6, 3, 6 ),
 ( 0.000000000000000000, 0.5000000000000000000, 1.000000000000000000 ),
 .UNSPECIFIED. ) ;
#8466 = AXIS2_PLACEMENT_3D ( 'NONE', #26243, #21861, #1913 ) ;
#8467 = CARTESIAN_POINT ( 'NONE',  ( -0.1724647388530000103, -101.1292389600000092, -15.50536992770000033 ) ) ;
#8468 = CARTESIAN_POINT ( 'NONE',  ( 8.007693474490000796, -59.01994772509999621, -22.21260941989999793 ) ) ;
#8469 = CARTESIAN_POINT ( 'NONE',  ( 15.23243409989999897, -101.1130130960000031, 2.433086515549999884 ) ) ;
#8470 = DIRECTION ( 'NONE',  ( 0.000000000000000000, -1.000000000000000000, 0.000000000000000000 ) ) ;
#8471 = DIRECTION ( 'NONE',  ( 0.000000000000000000, 1.000000000000000000, 0.000000000000000000 ) ) ;
#8472 = AXIS2_PLACEMENT_3D ( 'NONE', #20629, #25568, #16819 ) ;
#8473 = EDGE_LOOP ( 'NONE', ( #19051, #780, #5207, #23850 ) ) ;
#8474 = ADVANCED_FACE ( 'NONE', ( #4444 ), #26168, .T. ) ;
#8475 = CARTESIAN_POINT ( 'NONE',  ( 6.410511849489999747, -99.92384627689999377, 15.64910668389999771 ) ) ;
#8476 = CARTESIAN_POINT ( 'NONE',  ( -17.28030528624062967, -92.50821026832076655, -23.91007388581562054 ) ) ;
#8477 = EDGE_CURVE ( 'NONE', #7330, #24436, #17421, .T. ) ;
#8478 = EDGE_CURVE ( 'NONE', #15872, #25683, #7014, .T. ) ;
#8479 = ORIENTED_EDGE ( 'NONE', *, *, #7469, .T. ) ;
#8480 = CARTESIAN_POINT ( 'NONE',  ( -40.33934347143421917, -65.69529750894407982, -2.234392387587928575 ) ) ;
#8481 = CARTESIAN_POINT ( 'NONE',  ( 5.525098516430999140, -92.56492639272521217, -29.99554189593663622 ) ) ;
#8482 = CARTESIAN_POINT ( 'NONE',  ( 7.600472224660162368, -74.00014642295830924, 38.79568063749191253 ) ) ;
#8483 = ORIENTED_EDGE ( 'NONE', *, *, #5068, .F. ) ;
#8484 = CARTESIAN_POINT ( 'NONE',  ( 1.761322637119999923, -92.49537389370000540, -29.34428460070000000 ) ) ;
#8485 = CARTESIAN_POINT ( 'NONE',  ( 19.93464468349999663, -22.49864794700000203, -8.810945045800000486 ) ) ;
#8486 = CARTESIAN_POINT ( 'NONE',  ( -23.50862727400000196, -94.59276292389999696, -3.692480628369999796 ) ) ;
#8487 = CARTESIAN_POINT ( 'NONE',  ( -6.714989711430000341, -101.1700440390000040, 13.74992627059999961 ) ) ;
#8488 = ORIENTED_EDGE ( 'NONE', *, *, #20230, .F. ) ;
#8489 = CARTESIAN_POINT ( 'NONE',  ( -13.15133833870000046, -100.9197081840000010, -8.436152112259998503 ) ) ;
#8490 = VECTOR ( 'NONE', #2309, 1000.000000000000114 ) ;
#8491 = CARTESIAN_POINT ( 'NONE',  ( -12.97150031818777016, -100.3041487039710518, -11.07791448419877511 ) ) ;
#8492 = VERTEX_POINT ( 'NONE', #27183 ) ;
#8493 = CARTESIAN_POINT ( 'NONE',  ( 8.282596154190001059, -36.62694670249999973, -21.35529100209999953 ) ) ;
#8494 = TOROIDAL_SURFACE ( 'NONE', #12227, 55.85192378860000417, 0.3499999999999999778 ) ;
#8495 = CARTESIAN_POINT ( 'NONE',  ( 23.70295720520000060, -94.59276479689999917, -2.111852433950000218 ) ) ;
#8496 = DIRECTION ( 'NONE',  ( 0.8775825618903722036, 0.000000000000000000, -0.4794255386042041156 ) ) ;
#8497 = B_SPLINE_CURVE_WITH_KNOTS ( 'NONE', 3,
 ( #5656, #18646, #12206, #16731, #2916, #7431, #27241, #750, #25626, #9733, #27541, #7585, #25052, #11925, #9446, #7279, #27684, #5084, #14534, #890, #23441, #23020, #3478, #22874, #12341, #20976, #20830, #21250, #25483, #5518, #9595, #25353 ),
 .UNSPECIFIED., .F., .F.,
 ( 4, 2, 2, 1, 2, 2, 2, 2, 1, 2, 2, 2, 2, 1, 1, 2, 2, 4 ),
 ( 0.000000000000000000, 0.1249999999997466194, 0.1874999999996319056, 0.2187499999995851374, 0.2343749999995739519, 0.2499999999995627387, 0.3749999999996432853, 0.4374999999996742051, 0.4687499999996861955, 0.4843749999996909139, 0.4999999999996955768, 0.6249999999998518962, 0.6874999999999206191, 0.7187499999999508171, 0.7343749999999712452, 0.7421874999999767963, 0.7499999999999823475, 1.000000000000000000 ),
 .UNSPECIFIED. ) ;
#8498 = CARTESIAN_POINT ( 'NONE',  ( 22.55445185059999957, -19.16174980609999778, 0.9703951553680000286 ) ) ;
#8499 = CARTESIAN_POINT ( 'NONE',  ( -43.25394995532027309, -63.06523941402085143, 0.1332336900920622347 ) ) ;
#8500 = CARTESIAN_POINT ( 'NONE',  ( -19.85646363226101840, -92.53708507728565280, -23.15107591307967994 ) ) ;
#8501 = VERTEX_POINT ( 'NONE', #7370 ) ;
#8502 = CARTESIAN_POINT ( 'NONE',  ( 0.4184115225550000261, -93.00000000000000000, -30.38020727889999861 ) ) ;
#8503 = CARTESIAN_POINT ( 'NONE',  ( 16.42966103859999905, -94.59276292389999696, 17.21499949629999904 ) ) ;
#8504 = CARTESIAN_POINT ( 'NONE',  ( -36.75626636997765928, -65.12549727759366647, 0.1396600726223675148 ) ) ;
#8505 = B_SPLINE_SURFACE_WITH_KNOTS ( 'NONE', 5, 5, ( 
 ( #7283, #27392, #20385, #2482, #13682, #16009 ),
 ( #2920, #7440, #22589, #24914, #13826, #22731 ),
 ( #2772, #25210, #23025, #27545, #11627, #20537 ),
 ( #11339, #609, #9452, #5243, #11929, #20245 ),
 ( #18358, #26960, #6997, #27246, #11479, #20836 ),
 ( #16454, #894, #18651, #15860, #24770, #18931 ) ),
 .UNSPECIFIED., .F., .F., .F.,
 ( 6, 6 ),
 ( 6, 6 ),
 ( 1.645588054440000114, 2.780179228649999779 ),
 ( 0.000000000000000000, 2.000000000000000000 ),
 .UNSPECIFIED. ) ;
#8507 = ADVANCED_FACE ( 'NONE', ( #3009 ), #12517, .T. ) ;
#8506 = FACE_OUTER_BOUND ( 'NONE', #3783, .T. ) ;
#8508 = CARTESIAN_POINT ( 'NONE',  ( -18.78219790299999659, -19.46510053389999939, 11.52011550950000007 ) ) ;
#8509 = CARTESIAN_POINT ( 'NONE',  ( 7.731040106980000104, -34.67919398040000090, -21.19938061109999694 ) ) ;
#8510 = FACE_BOUND ( 'NONE', #14683, .T. ) ;
#8511 = ORIENTED_EDGE ( 'NONE', *, *, #27087, .F. ) ;
#8512 = ADVANCED_FACE ( 'NONE', ( #15794 ), #18140, .T. ) ;
#8513 = CARTESIAN_POINT ( 'NONE',  ( 36.32450514310000500, -74.54297172050000597, -14.86961494949999896 ) ) ;
#8514 = AXIS2_PLACEMENT_3D ( 'NONE', #23004, #24750, #13955 ) ;
#8515 = CARTESIAN_POINT ( 'NONE',  ( 21.93060288690000093, -36.53320241969999671, -9.504975477409999485 ) ) ;
#8516 = EDGE_CURVE ( 'NONE', #11916, #17492, #9420, .T. ) ;
#8517 = CARTESIAN_POINT ( 'NONE',  ( -2.587281238340000122, -58.59418302210000462, -25.28476856499999670 ) ) ;
#8518 = DIRECTION ( 'NONE',  ( 0.4794255386042040601, 0.000000000000000000, 0.8775825618903720926 ) ) ;
#8519 = CARTESIAN_POINT ( 'NONE',  ( -19.59930190490000257, -56.25996389440000200, 12.99169644580000060 ) ) ;
#8520 = FACE_OUTER_BOUND ( 'NONE', #15092, .T. ) ;
#8521 = CARTESIAN_POINT ( 'NONE',  ( 19.73295371884362837, -19.48431472826634092, -8.781177429089979114 ) ) ;
#8522 = EDGE_LOOP ( 'NONE', ( #26159, #28330, #10907, #2379 ) ) ;
#8523 = AXIS2_PLACEMENT_3D ( 'NONE', #8052, #4643, #11172 ) ;
#8524 = DIRECTION ( 'NONE',  ( 0.4794255386042040046, 0.000000000000000000, 0.8775825618903722036 ) ) ;
#8525 = DIRECTION ( 'NONE',  ( 0.000000000000000000, 1.000000000000000000, 0.000000000000000000 ) ) ;
#8526 = VERTEX_POINT ( 'NONE', #20631 ) ;
#8527 = DIRECTION ( 'NONE',  ( 0.000000000000000000, -1.000000000000000000, 0.000000000000000000 ) ) ;
#8528 = CARTESIAN_POINT ( 'NONE',  ( 19.53322478289999964, -19.46563609400000061, 10.20089682329999903 ) ) ;
#8529 = AXIS2_PLACEMENT_3D ( 'NONE', #26259, #21730, #14007 ) ;
#8530 = CARTESIAN_POINT ( 'NONE',  ( -22.19498675863994563, -74.23482419401921106, -32.69399667229252771 ) ) ;
#8531 = CARTESIAN_POINT ( 'NONE',  ( 20.80373709450000064, -18.50000000000000000, 8.362177511490001436 ) ) ;
#8532 = CARTESIAN_POINT ( 'NONE',  ( -23.50862727400000196, -94.59276292389999696, -3.692480628369999796 ) ) ;
#8533 = CARTESIAN_POINT ( 'NONE',  ( -13.14571786560000000, -100.8733988930000010, -8.628954981190000595 ) ) ;
#8534 = ORIENTED_EDGE ( 'NONE', *, *, #20740, .T. ) ;
#8535 = LINE ( 'NONE', #1857, #9251 ) ;
#8536 = CARTESIAN_POINT ( 'NONE',  ( -11.77131553929999974, -101.2010924020000004, -9.714008462309999814 ) ) ;
#8537 = CARTESIAN_POINT ( 'NONE',  ( -22.65726982507337439, -72.31233190808211475, 17.75628222746567175 ) ) ;
#8538 = CARTESIAN_POINT ( 'NONE',  ( -6.781378104809999030, -101.6484611540000031, 14.49182221120000058 ) ) ;
#8539 = ORIENTED_EDGE ( 'NONE', *, *, #2949, .T. ) ;
#8540 = EDGE_CURVE ( 'NONE', #18713, #4316, #21831, .T. ) ;
#8541 = AXIS2_PLACEMENT_3D ( 'NONE', #11477, #20383, #6842 ) ;
#8542 = AXIS2_PLACEMENT_3D ( 'NONE', #28050, #10106, #16979 ) ;
#8543 = EDGE_CURVE ( 'NONE', #10192, #7301, #22323, .T. ) ;
#8544 = CARTESIAN_POINT ( 'NONE',  ( 46.25000000000000000, -80.00000000000000000, -13.75000000000000000 ) ) ;
#8545 = CARTESIAN_POINT ( 'NONE',  ( -32.51044675360000014, -74.20254482470001278, -21.89358512240000110 ) ) ;
#8546 = CARTESIAN_POINT ( 'NONE',  ( -11.84764223884960010, -93.03217576144683676, -23.86221593305796063 ) ) ;
#8547 = ORIENTED_EDGE ( 'NONE', *, *, #22780, .T. ) ;
#8548 = B_SPLINE_CURVE_WITH_KNOTS ( 'NONE', 3,
 ( #24242, #1543, #8499, #4128, #28462, #22063, #19852, #6022, #6616, #28735 ),
 .UNSPECIFIED., .F., .F.,
 ( 4, 2, 2, 2, 4 ),
 ( 0.000000000000000000, 0.2500000000000000555, 0.5000000000000000000, 0.7500000000000000000, 1.000000000000000000 ),
 .UNSPECIFIED. ) ;
#8549 = DIRECTION ( 'NONE',  ( -0.000000000000000000, 1.000000000000000000, 0.000000000000000000 ) ) ;
#8550 = VECTOR ( 'NONE', #24134, 1000.000000000000000 ) ;
#8551 = ORIENTED_EDGE ( 'NONE', *, *, #17672, .T. ) ;
#8552 = CARTESIAN_POINT ( 'NONE',  ( -16.97479393769052436, -93.48480241359186493, -21.44694654164490188 ) ) ;
#8553 = ORIENTED_EDGE ( 'NONE', *, *, #9238, .F. ) ;
#8554 = CARTESIAN_POINT ( 'NONE',  ( 26.20138505510000115, -92.90721318149999775, 10.82755978760000204 ) ) ;
#8555 = DIRECTION ( 'NONE',  ( -0.2333505288839994030, 1.612292758439994142E-16, -0.9723926833689966465 ) ) ;
#8556 = ORIENTED_EDGE ( 'NONE', *, *, #23044, .F. ) ;
#8557 = CARTESIAN_POINT ( 'NONE',  ( -41.81440164397810122, -65.73344136606142740, 1.233272860631304590 ) ) ;
#8558 = CARTESIAN_POINT ( 'NONE',  ( -21.71458294140000334, -79.77274805400000446, -32.69645410180000056 ) ) ;
#8559 = EDGE_CURVE ( 'NONE', #15352, #27945, #8034, .T. ) ;
#8560 = ORIENTED_EDGE ( 'NONE', *, *, #14386, .F. ) ;
#8561 = CARTESIAN_POINT ( 'NONE',  ( -29.68198139278343461, -92.55389105863635280, -0.5288656702900278450 ) ) ;
#8562 = CARTESIAN_POINT ( 'NONE',  ( -23.36079593639999885, -92.54628605920001405, -19.03433440690000111 ) ) ;
#8563 = CARTESIAN_POINT ( 'NONE',  ( 18.48933855830000184, -18.50000000000000000, 10.02928721039999971 ) ) ;
#8564 = ORIENTED_EDGE ( 'NONE', *, *, #10874, .F. ) ;
#8565 = CARTESIAN_POINT ( 'NONE',  ( -1.271820802479999957, -100.9405348700000076, -15.89396400309999891 ) ) ;
#8566 = CARTESIAN_POINT ( 'NONE',  ( 12.40532806309999891, -101.0147083550000104, -9.373342067159999402 ) ) ;
#8567 = CARTESIAN_POINT ( 'NONE',  ( 0.000000000000000000, -28.69999999999999929, 0.000000000000000000 ) ) ;
#8568 = DIRECTION ( 'NONE',  ( 1.000000000000000000, 0.000000000000000000, 0.000000000000000000 ) ) ;
#8569 = CIRCLE ( 'NONE', #13707, 3.749999999999996447 ) ;
#8570 = CARTESIAN_POINT ( 'NONE',  ( 11.03417617331015776, -72.43641487375192867, -26.87308835027350540 ) ) ;
#8571 = CARTESIAN_POINT ( 'NONE',  ( -19.47450221869999964, -19.18187901349999791, 14.31430793610000052 ) ) ;
#8572 = ORIENTED_EDGE ( 'NONE', *, *, #25638, .T. ) ;
#8574 = EDGE_CURVE ( 'NONE', #24926, #11541, #24022, .T. ) ;
#8573 = CARTESIAN_POINT ( 'NONE',  ( -11.32307664120000013, -93.00000000000000000, 9.421136869679999748 ) ) ;
#8575 = CARTESIAN_POINT ( 'NONE',  ( 8.928661026786835819, -37.96769807237074446, -22.13892078761991300 ) ) ;
#8576 = CARTESIAN_POINT ( 'NONE',  ( -23.79797125454739515, -92.87422005959625437, -19.07634091649623542 ) ) ;
#8577 = CARTESIAN_POINT ( 'NONE',  ( 0.000000000000000000, -2.000000000000000000, 0.000000000000000000 ) ) ;
#8578 = CYLINDRICAL_SURFACE ( 'NONE', #14101, 39.24999999999998579 ) ;
#8579 = APPLICATION_PROTOCOL_DEFINITION ( 'draft international standard', 'automotive_design', 1998, #16492 ) ;
#8580 = AXIS2_PLACEMENT_3D ( 'NONE', #6586, #1785, #17512 ) ;
#8581 = CARTESIAN_POINT ( 'NONE',  ( -11.25326567110000120, -94.84395216780001192, -20.59896464009999661 ) ) ;
#8582 = DIRECTION ( 'NONE',  ( 0.000000000000000000, 1.000000000000000000, 0.000000000000000000 ) ) ;
#8583 = ORIENTED_EDGE ( 'NONE', *, *, #17001, .F. ) ;
#8584 = DIRECTION ( 'NONE',  ( 1.224606353819999829E-16, 0.000000000000000000, -1.000000000000000000 ) ) ;
#8585 = CARTESIAN_POINT ( 'NONE',  ( 15.91666814759999937, -101.0685845459999967, 2.371727654049999856 ) ) ;
#8586 = ORIENTED_EDGE ( 'NONE', *, *, #21224, .T. ) ;
#8587 = CARTESIAN_POINT ( 'NONE',  ( 19.84902281569999971, -35.76462365300000101, -9.046350557000000236 ) ) ;
#8588 = CARTESIAN_POINT ( 'NONE',  ( -7.325370793560000315, -19.50000000000000000, -24.94672208400000102 ) ) ;
#8589 = ORIENTED_EDGE ( 'NONE', *, *, #1377, .F. ) ;
#8590 = CARTESIAN_POINT ( 'NONE',  ( 0.000000000000000000, -16.10310889129999623, 0.000000000000000000 ) ) ;
#8591 = ADVANCED_FACE ( 'NONE', ( #2857 ), #20950, .F. ) ;
#8592 = CARTESIAN_POINT ( 'NONE',  ( -16.07900805970000135, -92.88046764189999749, -23.59102352649999901 ) ) ;
#8593 = AXIS2_PLACEMENT_3D ( 'NONE', #5290, #947, #22931 ) ;
#8594 = CARTESIAN_POINT ( 'NONE',  ( -6.644771110830000715, -97.11988490479998859, -19.57974298529999757 ) ) ;
#8595 = CARTESIAN_POINT ( 'NONE',  ( 0.000000000000000000, -2.000000000000000000, 0.000000000000000000 ) ) ;
#8596 = CARTESIAN_POINT ( 'NONE',  ( 6.931585813929999951, -44.93330283539999925, -21.84994998139999822 ) ) ;
#8597 = CARTESIAN_POINT ( 'NONE',  ( -11.41594964319999939, -19.46510059719999930, -18.84569179369999858 ) ) ;
#8598 = CARTESIAN_POINT ( 'NONE',  ( -40.18309971205388109, -65.73347097105947512, 2.187748804568729888 ) ) ;
#8599 = ORIENTED_EDGE ( 'NONE', *, *, #3531, .T. ) ;
#8600 = CARTESIAN_POINT ( 'NONE',  ( 13.09247055681168348, -101.1742791178134411, -9.823544259465782247 ) ) ;
#8601 = CARTESIAN_POINT ( 'NONE',  ( 23.90022363910000180, -27.02040600870000020, 1.451709836199999826 ) ) ;
#8602 = CARTESIAN_POINT ( 'NONE',  ( 22.40589624629999932, -65.01950563030000296, 11.38001362950000050 ) ) ;
#8603 = CARTESIAN_POINT ( 'NONE',  ( 40.00000000000000000, -84.50000000000000000, 3.574918139289999605E-15 ) ) ;
#8604 = ORIENTED_EDGE ( 'NONE', *, *, #15265, .T. ) ;
#8605 = ADVANCED_FACE ( 'NONE', ( #9237 ), #27479, .T. ) ;
#8606 = DIRECTION ( 'NONE',  ( -1.836909530730000236E-16, 0.000000000000000000, 1.000000000000000000 ) ) ;
#8607 = CARTESIAN_POINT ( 'NONE',  ( -14.34532190269999852, -92.62623300010000094, 26.10005267279999686 ) ) ;
#8608 = CARTESIAN_POINT ( 'NONE',  ( -20.66035133919229949, -93.50335891207949146, 15.02327711490973172 ) ) ;
#8609 = ORIENTED_EDGE ( 'NONE', *, *, #12413, .F. ) ;
#8610 = CARTESIAN_POINT ( 'NONE',  ( 26.98550733189999917, -69.11937516950000315, 0.7853522802169999872 ) ) ;
#8611 = CARTESIAN_POINT ( 'NONE',  ( 0.6965880932790000646, -100.8815367389999977, -15.65919131430000277 ) ) ;
#8612 = CARTESIAN_POINT ( 'NONE',  ( -14.42556421679999978, -111.0000000000000000, -2.978755036369999942 ) ) ;
#8613 = CARTESIAN_POINT ( 'NONE',  ( -12.47069904039999955, -69.15454048580001256, -24.11318545760000021 ) ) ;
#8614 = CARTESIAN_POINT ( 'NONE',  ( 22.44118743279999961, -65.00127796780000722, 11.39886732859999974 ) ) ;
#8615 = CARTESIAN_POINT ( 'NONE',  ( -11.27790836820000031, -42.20269670389999561, -22.30245189869999933 ) ) ;
#8616 = VERTEX_POINT ( 'NONE', #25300 ) ;
#8617 = DIRECTION ( 'NONE',  ( 0.000000000000000000, 0.000000000000000000, -1.000000000000000000 ) ) ;
#8618 = CARTESIAN_POINT ( 'NONE',  ( -15.59566370272417046, -92.58075529924404634, -24.03361414823421072 ) ) ;
#8619 = CARTESIAN_POINT ( 'NONE',  ( 27.81583421292586067, -92.50638022835023833, 12.51200364096112949 ) ) ;
#8620 = CARTESIAN_POINT ( 'NONE',  ( 23.40015495273278034, -60.60830808328032049, 10.49714536420149180 ) ) ;
#8621 = CARTESIAN_POINT ( 'NONE',  ( 3.129685915889999670, -92.55031878719999838, -28.46238550929999889 ) ) ;
#8622 = CARTESIAN_POINT ( 'NONE',  ( 6.766442258106934560, -101.4728631013423268, 14.64836155655668648 ) ) ;
#8623 = VERTEX_POINT ( 'NONE', #25435 ) ;
#8624 = CARTESIAN_POINT ( 'NONE',  ( 7.596414145187134537, -34.80520804250858902, -21.25273119204720018 ) ) ;
#8625 = CARTESIAN_POINT ( 'NONE',  ( -12.78944265896493881, -100.5550990431279672, -10.98195346763384528 ) ) ;
#8626 = ORIENTED_EDGE ( 'NONE', *, *, #18614, .T. ) ;
#8627 = CARTESIAN_POINT ( 'NONE',  ( 8.563236930420002224, -35.95760432990000055, -20.91612140590000024 ) ) ;
#8628 = EDGE_CURVE ( 'NONE', #17884, #8673, #18471, .T. ) ;
#8629 = CARTESIAN_POINT ( 'NONE',  ( -41.75000000000000000, -65.41419836839999391, 2.121055962329999822 ) ) ;
#8630 = ORIENTED_EDGE ( 'NONE', *, *, #16848, .T. ) ;
#8631 = EDGE_CURVE ( 'NONE', #28649, #17366, #1253, .T. ) ;
#8632 = CARTESIAN_POINT ( 'NONE',  ( -1.133529748880000021, -101.1659666750000071, -15.97345870559999881 ) ) ;
#8633 = DIRECTION ( 'NONE',  ( 0.000000000000000000, 1.000000000000000000, 0.000000000000000000 ) ) ;
#8634 = CARTESIAN_POINT ( 'NONE',  ( -40.00000000000000000, -84.50000000000000000, 1.424842520070000199E-16 ) ) ;
#8635 = CARTESIAN_POINT ( 'NONE',  ( -20.78903514689297793, -92.80045754870498342, -22.31742311452316585 ) ) ;
#8636 = ORIENTED_EDGE ( 'NONE', *, *, #12108, .T. ) ;
#8637 = EDGE_CURVE ( 'NONE', #26317, #2654, #27889, .T. ) ;
#8638 = CARTESIAN_POINT ( 'NONE',  ( -15.36545425250000108, -101.4254867220000023, 4.349819274109999689 ) ) ;
#8639 = CARTESIAN_POINT ( 'NONE',  ( -12.83931898810000050, -18.86159962690000214, 19.25717532500000218 ) ) ;
#8640 = CARTESIAN_POINT ( 'NONE',  ( 18.98618457029999718, -18.50000000000000000, -8.015883169030001199 ) ) ;
#8641 = EDGE_CURVE ( 'NONE', #14463, #13115, #4151, .T. ) ;
#8642 = CARTESIAN_POINT ( 'NONE',  ( -36.74920213680079684, -65.12158389260717684, -0.1356225091308175534 ) ) ;
#8643 = CARTESIAN_POINT ( 'NONE',  ( 13.73273575384635414, -100.1994045927716712, -10.26021908260778659 ) ) ;
#8644 = CARTESIAN_POINT ( 'NONE',  ( -12.76535171569999783, -68.20221627489999605, -23.31268819860000008 ) ) ;
#8645 = CARTESIAN_POINT ( 'NONE',  ( 30.97576656850000276, -38.00000000000000000, -19.97576656849999921 ) ) ;
#8646 = CARTESIAN_POINT ( 'NONE',  ( 7.429758031459999579, -34.95414986760000176, -21.31951852479999943 ) ) ;
#8647 = CIRCLE ( 'NONE', #24471, 7.249999999999999112 ) ;
#8648 = CARTESIAN_POINT ( 'NONE',  ( 18.97302707929999599, -20.32897095030000045, -9.021553180059999733 ) ) ;
#8649 = EDGE_LOOP ( 'NONE', ( #26644, #16213, #25374, #10095 ) ) ;
#8650 = CARTESIAN_POINT ( 'NONE',  ( 8.982198732169999644, -19.49132059749999968, -19.39131246359999849 ) ) ;
#8651 = ORIENTED_EDGE ( 'NONE', *, *, #23302, .T. ) ;
#8652 = CARTESIAN_POINT ( 'NONE',  ( -12.47194051069999965, -65.04696943620000127, 21.82660845869999733 ) ) ;
#8653 = CARTESIAN_POINT ( 'NONE',  ( 8.933651848329999368, -37.34495684180000552, -22.03427839560000123 ) ) ;
#8654 = CARTESIAN_POINT ( 'NONE',  ( -24.63095457940000088, -94.45168166349999694, -3.620300214920000315 ) ) ;
#8655 = CARTESIAN_POINT ( 'NONE',  ( -20.45998242170000125, -52.56313962730000355, 14.78974999389999923 ) ) ;
#8656 = B_SPLINE_CURVE_WITH_KNOTS ( 'NONE', 3,
 ( #20599, #658, #9511, #7340, #18413, #25118, #14033, #22939, #2979, #11838, #9651, #18557, #27451, #16932, #19253 ),
 .UNSPECIFIED., .F., .F.,
 ( 4, 2, 2, 1, 1, 1, 2, 2, 4 ),
 ( 0.000000000000000000, 0.2499999999999624745, 0.3749999999999431566, 0.4374999999999333866, 0.4687499999999291123, 0.4843749999999272804, 0.4921874999999277800, 0.4999999999999282796, 1.000000000000000000 ),
 .UNSPECIFIED. ) ;
#8657 = DIRECTION ( 'NONE',  ( 0.000000000000000000, 1.000000000000000000, 0.000000000000000000 ) ) ;
#8658 = ORIENTED_EDGE ( 'NONE', *, *, #26998, .T. ) ;
#8659 = CARTESIAN_POINT ( 'NONE',  ( 21.37164028449999975, -35.51902737180000003, -7.548682025549999786 ) ) ;
#8660 = FACE_OUTER_BOUND ( 'NONE', #8869, .T. ) ;
#8661 = EDGE_LOOP ( 'NONE', ( #716, #24278, #27965, #21098 ) ) ;
#8662 = FACE_OUTER_BOUND ( 'NONE', #6522, .T. ) ;
#8663 = EDGE_CURVE ( 'NONE', #18945, #1175, #17667, .T. ) ;
#8664 = CARTESIAN_POINT ( 'NONE',  ( 20.50323656299999797, -45.99732788909999925, 10.49340800629999926 ) ) ;
#8665 = DIRECTION ( 'NONE',  ( 0.000000000000000000, 1.000000000000000000, 0.000000000000000000 ) ) ;
#8666 = EDGE_CURVE ( 'NONE', #14011, #11658, #5112, .T. ) ;
#8667 = CARTESIAN_POINT ( 'NONE',  ( -15.51746188589999953, -101.3079808070000070, 3.547079192720000052 ) ) ;
#8668 = CARTESIAN_POINT ( 'NONE',  ( 8.271554555860001656, -65.04365450350000799, -23.74272563809999781 ) ) ;
#8669 = ORIENTED_EDGE ( 'NONE', *, *, #18503, .T. ) ;
#8670 = CARTESIAN_POINT ( 'NONE',  ( -12.59478316103309758, -72.72581917438233745, -25.71960458748240086 ) ) ;
#8671 = CARTESIAN_POINT ( 'NONE',  ( -22.97965035359588626, -72.72581917439157451, 17.08983009374688322 ) ) ;
#8672 = CARTESIAN_POINT ( 'NONE',  ( 22.29407657802536846, -58.30792671702914021, -7.076158844936190739 ) ) ;
#8673 = VERTEX_POINT ( 'NONE', #16539 ) ;
#8674 = CARTESIAN_POINT ( 'NONE',  ( 32.75000000000000000, -69.50000000000000000, 3.321731688439999685E-15 ) ) ;
#8675 = CARTESIAN_POINT ( 'NONE',  ( -32.51340285799999918, -74.11800272920001476, -22.15126936060000062 ) ) ;
#8676 = CARTESIAN_POINT ( 'NONE',  ( -22.24051182591864873, -79.62418415837113628, -32.83124725485127726 ) ) ;
#8677 = ORIENTED_EDGE ( 'NONE', *, *, #5478, .F. ) ;
#8678 = CARTESIAN_POINT ( 'NONE',  ( 19.56129018700000088, -35.88702891199999812, -9.158871637020000733 ) ) ;
#8679 = CARTESIAN_POINT ( 'NONE',  ( 12.78866345099999968, -92.54627856989999657, 27.28520986150000027 ) ) ;
#8680 = ORIENTED_EDGE ( 'NONE', *, *, #17561, .F. ) ;
#8681 = CARTESIAN_POINT ( 'NONE',  ( -12.27720009871537776, -94.79128788117789384, -21.50236666293719878 ) ) ;
#8682 = EDGE_LOOP ( 'NONE', ( #7276, #428, #16622, #14130 ) ) ;
#8683 = CARTESIAN_POINT ( 'NONE',  ( 21.12092159740000241, -93.86380950250000410, 13.35475519379999909 ) ) ;
#8684 = CARTESIAN_POINT ( 'NONE',  ( 46.38121015490000332, -73.57738697389999061, -3.489819008620000051 ) ) ;
#8685 = EDGE_LOOP ( 'NONE', ( #8599, #17655, #5673, #26632 ) ) ;
#8686 = CARTESIAN_POINT ( 'NONE',  ( -41.75000000000000000, -65.63577453799999262, 1.587713240270000048 ) ) ;
#8687 = CARTESIAN_POINT ( 'NONE',  ( -22.38372304750000197, -80.07464437650000377, -32.45232253209999840 ) ) ;
#8688 = EDGE_CURVE ( 'NONE', #16619, #26053, #21384, .T. ) ;
#8689 = STYLED_ITEM ( 'NONE', ( #21172 ), #16071 ) ;
#8690 = CARTESIAN_POINT ( 'NONE',  ( 8.522642244679998313, -37.33399608140000225, -21.80457156990000200 ) ) ;
#8691 = CARTESIAN_POINT ( 'NONE',  ( -16.39360122190000268, -92.99570653139998910, -21.25352984659999933 ) ) ;
#8692 = CARTESIAN_POINT ( 'NONE',  ( 27.11492913210000211, -72.00000000000000000, 10.50528373760000100 ) ) ;
#8693 = VERTEX_POINT ( 'NONE', #21063 ) ;
#8694 = EDGE_CURVE ( 'NONE', #24500, #842, #28171, .T. ) ;
#8695 = CARTESIAN_POINT ( 'NONE',  ( 36.22844186549999534, -74.00000000000000000, -13.75000000000000000 ) ) ;
#8696 = CARTESIAN_POINT ( 'NONE',  ( 12.35324891399999991, -101.1417990620000040, -9.783258604670001191 ) ) ;
#8697 = CARTESIAN_POINT ( 'NONE',  ( -24.10762033259999981, -79.50000000000000000, -34.71422205039999653 ) ) ;
#8698 = CARTESIAN_POINT ( 'NONE',  ( -11.80896971761302794, -94.89420224084436484, -21.43714084844935641 ) ) ;
#8699 = CIRCLE ( 'NONE', #22207, 20.64285714289999873 ) ;
#8700 = CARTESIAN_POINT ( 'NONE',  ( 21.92880674030000065, -37.95796630489999757, -8.677144366489999427 ) ) ;
#8701 = DIRECTION ( 'NONE',  ( -0.4707989697561778542, 0.1888473936500709438, -0.8617917335343248109 ) ) ;
#8702 = DIRECTION ( 'NONE',  ( -0.4151946956541399669, 0.5000000000001689759, -0.7600087925152558821 ) ) ;
#8703 = VERTEX_POINT ( 'NONE', #1526 ) ;
#8704 = FACE_OUTER_BOUND ( 'NONE', #2054, .T. ) ;
#8705 = FACE_OUTER_BOUND ( 'NONE', #16353, .T. ) ;
#8706 = CARTESIAN_POINT ( 'NONE',  ( 8.831064126840001194, -94.59276292389999696, -22.09756266850000017 ) ) ;
#8707 = DIRECTION ( 'NONE',  ( 1.000000000000000000, 0.000000000000000000, 0.000000000000000000 ) ) ;
#8708 = CARTESIAN_POINT ( 'NONE',  ( -0.5776010673831374342, -92.56772982776919889, -30.49459145784739533 ) ) ;
#8709 = TOROIDAL_SURFACE ( 'NONE', #15211, 0.5000000000000000000, 0.5000000000000000000 ) ;
#8710 = CARTESIAN_POINT ( 'NONE',  ( 0.000000000000000000, 0.000000000000000000, 0.000000000000000000 ) ) ;
#8711 = AXIS2_PLACEMENT_3D ( 'NONE', #15364, #12883, #19335 ) ;
#8712 = DIRECTION ( 'NONE',  ( 0.000000000000000000, -1.000000000000000000, 0.000000000000000000 ) ) ;
#8713 = VERTEX_POINT ( 'NONE', #9961 ) ;
#8714 = CARTESIAN_POINT ( 'NONE',  ( 22.14044571250000004, -95.71128647349999596, -4.387446428019999622 ) ) ;
#8715 = ORIENTED_EDGE ( 'NONE', *, *, #3151, .F. ) ;
#8716 = B_SPLINE_CURVE_WITH_KNOTS ( 'NONE', 5,
 ( #15739, #14298, #28118, #12239, #21153, #1208 ),
 .UNSPECIFIED., .F., .F.,
 ( 6, 6 ),
 ( 0.000000000000000000, 1.000000000000000000 ),
 .UNSPECIFIED. ) ;
#8717 = CIRCLE ( 'NONE', #13390, 7.750000000000000000 ) ;
#8718 = CARTESIAN_POINT ( 'NONE',  ( -4.500000000000000000, -13.00000000000000000, 31.00000000000000000 ) ) ;
#8719 = DIRECTION ( 'NONE',  ( 0.000000000000000000, 1.000000000000000000, 0.000000000000000000 ) ) ;
#8720 = ORIENTED_EDGE ( 'NONE', *, *, #243, .F. ) ;
#8721 = LINE ( 'NONE', #2345, #3406 ) ;
#8722 = EDGE_CURVE ( 'NONE', #7826, #26140, #13603, .T. ) ;
#8723 = ADVANCED_FACE ( 'NONE', ( #25713 ), #116, .T. ) ;
#8724 = B_SPLINE_CURVE_WITH_KNOTS ( 'NONE', 3,
 ( #19478, #17020, #5804, #3761, #12624, #21536, #22253, #6817, #24439, #20067 ),
 .UNSPECIFIED., .F., .F.,
 ( 4, 2, 2, 2, 4 ),
 ( 0.000000000000000000, 0.2500000000000000000, 0.5000000000000000000, 0.7500000000000000000, 1.000000000000000000 ),
 .UNSPECIFIED. ) ;
#8725 = PRODUCT_DEFINITION_SHAPE ( 'NONE', 'NONE',  #28809 ) ;
#8726 = CARTESIAN_POINT ( 'NONE',  ( -14.08277339220000179, -92.72294953669999984, -23.91615244109999949 ) ) ;
#8727 = CARTESIAN_POINT ( 'NONE',  ( 22.62080797868468451, -64.93834956056363694, 11.20705156649500367 ) ) ;
#8728 = CARTESIAN_POINT ( 'NONE',  ( -26.32352847549999808, -93.13202907830000754, -0.6218978954889999855 ) ) ;
#8729 = CARTESIAN_POINT ( 'NONE',  ( -20.10936447829999807, -95.60043714340001486, 10.20867317439999944 ) ) ;
#8730 = CARTESIAN_POINT ( 'NONE',  ( -29.65790904711468912, -92.62938374240729900, 7.117544636880208664 ) ) ;
#8731 = CARTESIAN_POINT ( 'NONE',  ( 27.49607050420000220, -45.73899999920000425, 1.934818144049999855 ) ) ;
#8732 = ORIENTED_EDGE ( 'NONE', *, *, #28182, .F. ) ;
#8733 = AXIS2_PLACEMENT_3D ( 'NONE', #19930, #11175, #13522 ) ;
#8734 = CARTESIAN_POINT ( 'NONE',  ( 0.000000000000000000, -15.00000000000000000, 0.000000000000000000 ) ) ;
#8735 = CARTESIAN_POINT ( 'NONE',  ( 22.03613531989999785, -19.46548176030000121, -0.1168477070839999965 ) ) ;
#8736 = CARTESIAN_POINT ( 'NONE',  ( -14.48027910668785090, -80.37149491588407102, 36.48148420943337555 ) ) ;
#8737 = FACE_OUTER_BOUND ( 'NONE', #18807, .T. ) ;
#8738 = ORIENTED_EDGE ( 'NONE', *, *, #7719, .T. ) ;
#8739 = CARTESIAN_POINT ( 'NONE',  ( -38.25000000000000000, -63.30468293320000583, -1.587713240270000048 ) ) ;
#8740 = CARTESIAN_POINT ( 'NONE',  ( -15.53919574999999931, -92.59715193510000120, 23.72508021810000045 ) ) ;
#8741 = CARTESIAN_POINT ( 'NONE',  ( 26.58750744064022342, -92.65509297688441848, -7.785012216743809610 ) ) ;
#8742 = EDGE_LOOP ( 'NONE', ( #27458, #2529, #17992 ) ) ;
#8743 = CARTESIAN_POINT ( 'NONE',  ( 38.62788659690000515, -74.00000000000000000, -7.627568735119999666 ) ) ;
#8744 = AXIS2_PLACEMENT_3D ( 'NONE', #3933, #21704, #1755 ) ;
#8745 = CARTESIAN_POINT ( 'NONE',  ( 0.2554224435499999890, -101.2010924020000004, -15.25977029010000052 ) ) ;
#8746 = CARTESIAN_POINT ( 'NONE',  ( 23.33794867324012756, -74.10671401505453559, -31.32117936075259834 ) ) ;
#8747 = CARTESIAN_POINT ( 'NONE',  ( 15.71280846430000366, -101.4254868729999970, 2.848724509360000212 ) ) ;
#8748 = CARTESIAN_POINT ( 'NONE',  ( -11.31871588699999975, -57.41946978100000365, -22.35641894780000172 ) ) ;
#8749 = ORIENTED_EDGE ( 'NONE', *, *, #15481, .T. ) ;
#8750 = EDGE_CURVE ( 'NONE', #14137, #16242, #28591, .T. ) ;
#8751 = CARTESIAN_POINT ( 'NONE',  ( 23.23309277570114162, -57.41957472273993801, -9.464544134220355787 ) ) ;
#8752 = VECTOR ( 'NONE', #17841, 1000.000000000000000 ) ;
#8753 = ORIENTED_EDGE ( 'NONE', *, *, #22668, .F. ) ;
#8754 = DIRECTION ( 'NONE',  ( 1.000000000000000000, 0.000000000000000000, 2.220446049250000002E-16 ) ) ;
#8755 = DIRECTION ( 'NONE',  ( 0.000000000000000000, -1.000000000000000000, 0.000000000000000000 ) ) ;
#8756 = CIRCLE ( 'NONE', #12481, 61.35000000000000142 ) ;
#8757 = CARTESIAN_POINT ( 'NONE',  ( -41.95806561253180433, -65.73717277034926099, -0.9755888848881901776 ) ) ;
#8758 = ORIENTED_EDGE ( 'NONE', *, *, #10051, .T. ) ;
#8759 = CARTESIAN_POINT ( 'NONE',  ( -19.97974349676479378, -95.94979037552315049, 10.41052685295677982 ) ) ;
#8760 = CARTESIAN_POINT ( 'NONE',  ( 2.842170943039999687E-14, -74.00000000000000000, 1.776356839399999804E-15 ) ) ;
#8761 = CARTESIAN_POINT ( 'NONE',  ( 18.94592261899999741, -19.50000000009999823, -9.024080787920000901 ) ) ;
#8762 = CARTESIAN_POINT ( 'NONE',  ( -40.00000000000000000, -77.00000000000000000, 0.000000000000000000 ) ) ;
#8763 = CARTESIAN_POINT ( 'NONE',  ( -6.569756907160000381, -101.2530993010000060, 13.70087252790000143 ) ) ;
#8764 = VERTEX_POINT ( 'NONE', #15309 ) ;
#8765 = DIRECTION ( 'NONE',  ( -0.3687499999999802047, 0.000000000000000000, 0.9295286103719532234 ) ) ;
#8766 = CARTESIAN_POINT ( 'NONE',  ( -13.09565534707698298, -100.1585711159101777, -11.11278395076808501 ) ) ;
#8767 = ORIENTED_EDGE ( 'NONE', *, *, #17642, .F. ) ;
#8768 = FACE_OUTER_BOUND ( 'NONE', #19182, .T. ) ;
#8769 = CARTESIAN_POINT ( 'NONE',  ( 23.58467268920000137, -94.98812656910000385, -2.405348287990000333 ) ) ;
#8770 = CARTESIAN_POINT ( 'NONE',  ( 8.765232847019998275, -98.65049302040000612, 16.41568421879999917 ) ) ;
#8771 = CARTESIAN_POINT ( 'NONE',  ( 21.71614775840000178, -18.61783141309999934, 0.2114479593869999785 ) ) ;
#8772 = DIRECTION ( 'NONE',  ( 0.8775825618903722036, 0.000000000000000000, -0.4794255386042041156 ) ) ;
#8773 = CIRCLE ( 'NONE', #12493, 5.500000000000000000 ) ;
#8774 = CARTESIAN_POINT ( 'NONE',  ( -11.35954001540000036, -74.00000000000000000, 46.75000000000000000 ) ) ;
#8775 = CARTESIAN_POINT ( 'NONE',  ( -14.94683085009999957, -101.1292394720000090, 4.127768892550000679 ) ) ;
#8776 = CARTESIAN_POINT ( 'NONE',  ( -13.92598445589999834, -18.50000000000000000, 19.64619795940000202 ) ) ;
#8777 = DIRECTION ( 'NONE',  ( 0.8479091047340885368, 0.000000000000000000, -0.5301416321220553396 ) ) ;
#8778 = AXIS2_PLACEMENT_3D ( 'NONE', #21078, #27645, #1139 ) ;
#8779 = AXIS2_PLACEMENT_3D ( 'NONE', #11170, #148, #8999 ) ;
#8780 = CARTESIAN_POINT ( 'NONE',  ( -36.79999999999999716, -65.14977478849999670, 0.1732050807570000017 ) ) ;
#8781 = VECTOR ( 'NONE', #2072, 1000.000000000000000 ) ;
#8782 = DIRECTION ( 'NONE',  ( 0.4794255386042040046, 0.000000000000000000, 0.8775825618903722036 ) ) ;
#8783 = CARTESIAN_POINT ( 'NONE',  ( 25.78653733048833274, -61.62289756460010182, 1.407790978842422991 ) ) ;
#8784 = DIRECTION ( 'NONE',  ( 0.000000000000000000, -1.000000000000000000, 0.000000000000000000 ) ) ;
#8785 = CARTESIAN_POINT ( 'NONE',  ( 47.25000000000000000, -82.25000000000000000, 7.327133149349999745E-15 ) ) ;
#8786 = CARTESIAN_POINT ( 'NONE',  ( 22.38748998554977021, -94.04667188344215845, 13.21713613643446550 ) ) ;
#8787 = ORIENTED_EDGE ( 'NONE', *, *, #27284, .T. ) ;
#8788 = CARTESIAN_POINT ( 'NONE',  ( 8.153556109420000197, -19.46889320269999857, -20.47461235829999993 ) ) ;
#8789 = B_SPLINE_CURVE_WITH_KNOTS ( 'NONE', 5,
 ( #18119, #72, #8918, #17828, #24967, #7056, #9209, #24523, #27161 ),
 .UNSPECIFIED., .F., .F.,
 ( 6, 3, 6 ),
 ( 0.000000000000000000, 1.237573681330000008, 1.566718891470000097 ),
 .UNSPECIFIED. ) ;
#8790 = EDGE_CURVE ( 'NONE', #9549, #9768, #7461, .T. ) ;
#8791 = ORIENTED_EDGE ( 'NONE', *, *, #23302, .F. ) ;
#8792 = CARTESIAN_POINT ( 'NONE',  ( -12.70376715600000139, -58.97497545609999747, 20.32514926010000167 ) ) ;
#8793 = CARTESIAN_POINT ( 'NONE',  ( -14.65665288169999947, -79.50000000000000000, 36.94583914790000279 ) ) ;
#8794 = CIRCLE ( 'NONE', #5105, 57.75000000000000000 ) ;
#8795 = EDGE_CURVE ( 'NONE', #22471, #6872, #1795, .T. ) ;
#8796 = CARTESIAN_POINT ( 'NONE',  ( -24.82370543889999936, -93.86380869120000625, -2.868192742509999782 ) ) ;
#8797 = CARTESIAN_POINT ( 'NONE',  ( -19.61382872410000289, -55.05312981980000586, 12.65941854959999979 ) ) ;
#8798 = EDGE_CURVE ( 'NONE', #9643, #17262, #12700, .T. ) ;
#8799 = DIRECTION ( 'NONE',  ( 0.000000000000000000, -1.000000000000000000, 0.000000000000000000 ) ) ;
#8800 = AXIS2_PLACEMENT_3D ( 'NONE', #3046, #7115, #27361 ) ;
#8801 = VECTOR ( 'NONE', #11314, 1000.000000000000000 ) ;
#8802 = CARTESIAN_POINT ( 'NONE',  ( 15.87132499590000023, -100.6809449770000100, 4.272090527209999600 ) ) ;
#8803 = EDGE_LOOP ( 'NONE', ( #16857, #5973, #16449, #17122 ) ) ;
#8804 = CARTESIAN_POINT ( 'NONE',  ( 21.51316767409999997, -36.56981899810000414, -7.049162417470000719 ) ) ;
#8805 = DIRECTION ( 'NONE',  ( 0.000000000000000000, 1.000000000000000000, 0.000000000000000000 ) ) ;
#8806 = ORIENTED_EDGE ( 'NONE', *, *, #15481, .F. ) ;
#8807 = DIRECTION ( 'NONE',  ( 0.000000000000000000, 1.000000000000000000, 0.000000000000000000 ) ) ;
#8808 = ORIENTED_EDGE ( 'NONE', *, *, #5385, .F. ) ;
#8809 = DIRECTION ( 'NONE',  ( 0.7071067811865475727, 0.000000000000000000, 0.7071067811865475727 ) ) ;
#8810 = CARTESIAN_POINT ( 'NONE',  ( 20.22207915179999915, -26.09432050500000244, 9.873638696180000451 ) ) ;
#8811 = DIRECTION ( 'NONE',  ( 0.000000000000000000, 0.000000000000000000, 1.000000000000000000 ) ) ;
#8812 = CARTESIAN_POINT ( 'NONE',  ( -13.94259793059999986, -74.00000000000000000, 36.22705481479999889 ) ) ;
#8813 = CARTESIAN_POINT ( 'NONE',  ( 9.685027244209999608, -66.27232962659999771, -24.54482743630000030 ) ) ;
#8814 = CARTESIAN_POINT ( 'NONE',  ( -16.12089651170244053, -99.24541079440805902, 7.516693469902168800 ) ) ;
#8815 = ORIENTED_EDGE ( 'NONE', *, *, #5891, .T. ) ;
#8816 = DIRECTION ( 'NONE',  ( 0.000000000000000000, -1.000000000000000000, 0.000000000000000000 ) ) ;
#8817 = CARTESIAN_POINT ( 'NONE',  ( -12.27960098470000005, -100.1275643909999928, -11.24051300700000056 ) ) ;
#8818 = CARTESIAN_POINT ( 'NONE',  ( 21.79177587533808236, -19.48886652631049188, 9.573355507166157352 ) ) ;
#8819 = AXIS2_PLACEMENT_3D ( 'NONE', #24429, #6505, #26616 ) ;
#8820 = CARTESIAN_POINT ( 'NONE',  ( 22.91500301472982315, -62.03080628915128614, -7.299858054674131402 ) ) ;
#8821 = ORIENTED_EDGE ( 'NONE', *, *, #18906, .T. ) ;
#8822 = DIRECTION ( 'NONE',  ( 1.000000000000000000, 0.000000000000000000, 0.000000000000000000 ) ) ;
#8823 = CARTESIAN_POINT ( 'NONE',  ( -32.17258283129999796, -74.02008960720000630, -21.87546129999999778 ) ) ;
#8824 = ORIENTED_EDGE ( 'NONE', *, *, #14651, .T. ) ;
#8825 = EDGE_CURVE ( 'NONE', #9115, #5383, #425, .T. ) ;
#8826 = CARTESIAN_POINT ( 'NONE',  ( 26.77683864449999973, -23.00000000000000000, 49.01467436490000296 ) ) ;
#8827 = DIRECTION ( 'NONE',  ( -0.8687683739962963614, -0.3326668106478661846, 0.3668437070977342285 ) ) ;
#8828 = CARTESIAN_POINT ( 'NONE',  ( -18.24886321459684524, -94.80026206438209613, 16.23660667693922477 ) ) ;
#8829 = EDGE_CURVE ( 'NONE', #23155, #9669, #3836, .T. ) ;
#8830 = VERTEX_POINT ( 'NONE', #26278 ) ;
#8831 = DIRECTION ( 'NONE',  ( 0.000000000000000000, 1.000000000000000000, 0.000000000000000000 ) ) ;
#8832 = ORIENTED_EDGE ( 'NONE', *, *, #1406, .T. ) ;
#8833 = CARTESIAN_POINT ( 'NONE',  ( 46.44492052809999905, -73.92805234950000681, -3.607313045449999755 ) ) ;
#8834 = APPLICATION_CONTEXT ( 'automotive_design' ) ;
#8835 = ORIENTED_EDGE ( 'NONE', *, *, #25678, .F. ) ;
#8836 = AXIS2_PLACEMENT_3D ( 'NONE', #22538, #20043, #26765 ) ;
#8837 = CARTESIAN_POINT ( 'NONE',  ( 0.000000000000000000, -82.25000000000000000, 0.000000000000000000 ) ) ;
#8838 = CARTESIAN_POINT ( 'NONE',  ( 20.84246830319968069, -57.47571038088945983, 10.69856926729981872 ) ) ;
#8839 = AXIS2_PLACEMENT_3D ( 'NONE', #21475, #24374, #25988 ) ;
#8840 = CIRCLE ( 'NONE', #3314, 0.9999999999999997780 ) ;
#8841 = ORIENTED_EDGE ( 'NONE', *, *, #1923, .T. ) ;
#8842 = CARTESIAN_POINT ( 'NONE',  ( -10.61287167059999881, -19.46510050329999686, 19.30934957549999709 ) ) ;
#8843 = CARTESIAN_POINT ( 'NONE',  ( 12.14638440039999878, -101.1180794200000008, -9.660115219679999754 ) ) ;
#8844 = CARTESIAN_POINT ( 'NONE',  ( -16.37879490400000293, -92.97898997919999431, -21.15867040639999885 ) ) ;
#8845 = CARTESIAN_POINT ( 'NONE',  ( 0.000000000000000000, -33.49689110869999809, 0.000000000000000000 ) ) ;
#8846 = ORIENTED_EDGE ( 'NONE', *, *, #26245, .T. ) ;
#8847 = LINE ( 'NONE', #302, #26481 ) ;
#8848 = CARTESIAN_POINT ( 'NONE',  ( 13.78612279620000081, -100.0994409990000094, -10.32398801709999958 ) ) ;
#8849 = CARTESIAN_POINT ( 'NONE',  ( -22.09341704730000089, -74.03505044649999434, -32.27636733649999456 ) ) ;
#8850 = CARTESIAN_POINT ( 'NONE',  ( -1.984042180019999879, -56.24740423709999249, -23.80057596580000023 ) ) ;
#8851 = LINE ( 'NONE', #10876, #7387 ) ;
#8852 = CARTESIAN_POINT ( 'NONE',  ( 11.81986579350000000, -72.00000321289999761, -27.35691362350000233 ) ) ;
#8853 = CARTESIAN_POINT ( 'NONE',  ( 21.34788034980000049, -35.28814072549999281, -7.426815654249999454 ) ) ;
#8854 = VERTEX_POINT ( 'NONE', #1667 ) ;
#8855 = CARTESIAN_POINT ( 'NONE',  ( 0.000000000000000000, -92.50000000000000000, 0.000000000000000000 ) ) ;
#8856 = CARTESIAN_POINT ( 'NONE',  ( 20.30256298825100103, -72.52349576872460091, -31.02298866334802341 ) ) ;
#8857 = DIRECTION ( 'NONE',  ( 0.000000000000000000, 1.000000000000000000, 0.000000000000000000 ) ) ;
#8858 = DIRECTION ( 'NONE',  ( -0.9704142011833033488, 0.000000000000000000, -0.2414462220490755373 ) ) ;
#8859 = CARTESIAN_POINT ( 'NONE',  ( -0.8435683774100874999, -92.52640451561843804, -30.48833712424519149 ) ) ;
#8860 = CIRCLE ( 'NONE', #19559, 0.4999999999999995559 ) ;
#8861 = VECTOR ( 'NONE', #433, 999.9999999999998863 ) ;
#8862 = ADVANCED_FACE ( 'NONE', ( #10504 ), #12063, .F. ) ;
#8863 = AXIS2_PLACEMENT_3D ( 'NONE', #2190, #19798, #6558 ) ;
#8864 = PRODUCT_CONTEXT ( 'NONE', #17800, 'mechanical' ) ;
#8865 = CARTESIAN_POINT ( 'NONE',  ( -6.285925807789999986, -101.1889999979999999, 14.71350185169999847 ) ) ;
#8866 = EDGE_CURVE ( 'NONE', #26695, #10529, #10637, .T. ) ;
#8867 = ORIENTED_EDGE ( 'NONE', *, *, #14950, .F. ) ;
#8868 = CARTESIAN_POINT ( 'NONE',  ( 21.03420648150000360, -97.01677119799998650, -2.189672962029999947 ) ) ;
#8869 = EDGE_LOOP ( 'NONE', ( #26986, #26205, #10395, #10328 ) ) ;
#8870 = LINE ( 'NONE', #11196, #25174 ) ;
#8871 = CARTESIAN_POINT ( 'NONE',  ( -16.33619708059999809, -101.1889999979999999, 3.920288885250000188 ) ) ;
#8872 = ORIENTED_EDGE ( 'NONE', *, *, #3030, .T. ) ;
#8873 = CARTESIAN_POINT ( 'NONE',  ( 29.82685776330000138, -73.10703858080000828, -25.25856749939999801 ) ) ;
#8874 = CARTESIAN_POINT ( 'NONE',  ( -4.536235172729999654, -98.62857337580000205, -18.99292533490000068 ) ) ;
#8875 = DIRECTION ( 'NONE',  ( 0.000000000000000000, 0.000000000000000000, -1.000000000000000000 ) ) ;
#8876 = CARTESIAN_POINT ( 'NONE',  ( 1.495914020609999895, -94.52293512119999264, 23.88472631159999793 ) ) ;
#8877 = CARTESIAN_POINT ( 'NONE',  ( -41.75000000000000000, -63.24880261864031183, 1.898084215881414627 ) ) ;
#8878 = DIRECTION ( 'NONE',  ( 0.000000000000000000, 1.000000000000000000, 0.000000000000000000 ) ) ;
#8879 = CIRCLE ( 'NONE', #1919, 39.25000000000000000 ) ;
#8880 = CARTESIAN_POINT ( 'NONE',  ( 21.54175492566420758, -37.57472077364804619, -7.824415534489649993 ) ) ;
#8881 = VERTEX_POINT ( 'NONE', #1801 ) ;
#8882 = CARTESIAN_POINT ( 'NONE',  ( 11.37272679149999988, -93.24058218660000819, -23.59428585010000035 ) ) ;
#8883 = VECTOR ( 'NONE', #20703, 1000.000000000000000 ) ;
#8884 = CARTESIAN_POINT ( 'NONE',  ( -21.35786096709999882, -65.07443093669999712, 13.27975207949999970 ) ) ;
#8885 = CARTESIAN_POINT ( 'NONE',  ( -14.90808802380093567, -79.75935533160925672, 36.30859255103454331 ) ) ;
#8886 = CARTESIAN_POINT ( 'NONE',  ( 40.14660266869234562, -74.07739338297623988, 7.248706349661884651 ) ) ;
#8887 = ORIENTED_EDGE ( 'NONE', *, *, #21049, .F. ) ;
#8888 = CARTESIAN_POINT ( 'NONE',  ( -2.719187424204038805, -64.35840095536138961, -26.13123326132488344 ) ) ;
#8889 = CARTESIAN_POINT ( 'NONE',  ( -18.01708526109999653, -94.13770192399999814, 18.41653692539999909 ) ) ;
#8890 = CARTESIAN_POINT ( 'NONE',  ( 7.082639064089999437, -58.88902008639999508, -22.31331248359999719 ) ) ;
#8891 = EDGE_LOOP ( 'NONE', ( #25499, #14631, #19097, #4308, #21569, #24524, #3674 ) ) ;
#8892 = CARTESIAN_POINT ( 'NONE',  ( 26.57206512919999852, -68.20221323439999139, 0.6012600223039999969 ) ) ;
#8893 = CARTESIAN_POINT ( 'NONE',  ( 0.4823327075950000209, -101.1976625110000043, -16.34256275559999949 ) ) ;
#8894 = CARTESIAN_POINT ( 'NONE',  ( 9.464545271429999573, -57.41957453189999683, -23.23309258220000117 ) ) ;
#8895 = CARTESIAN_POINT ( 'NONE',  ( -12.79700594729999885, -68.93455661459999817, -23.67518218120000384 ) ) ;
#8896 = CARTESIAN_POINT ( 'NONE',  ( -11.10145580579999880, -49.82767789670000269, -21.89191623019999966 ) ) ;
#8897 = EDGE_CURVE ( 'NONE', #3127, #8919, #5565, .T. ) ;
#8898 = DIRECTION ( 'NONE',  ( 0.000000000000000000, -1.000000000000000000, 0.000000000000000000 ) ) ;
#8899 = FACE_OUTER_BOUND ( 'NONE', #2969, .T. ) ;
#8900 = EDGE_CURVE ( 'NONE', #5317, #6780, #478, .T. ) ;
#8901 = VECTOR ( 'NONE', #10317, 1000.000000000000000 ) ;
#8902 = EDGE_CURVE ( 'NONE', #20652, #20862, #24164, .T. ) ;
#8903 = ORIENTED_EDGE ( 'NONE', *, *, #27855, .F. ) ;
#8904 = CARTESIAN_POINT ( 'NONE',  ( 28.43118412462271749, -92.81370807102868525, 11.04165370930220291 ) ) ;
#8905 = CARTESIAN_POINT ( 'NONE',  ( -10.20110288159999890, -80.50000000000000000, 41.00000000000000000 ) ) ;
#8906 = CARTESIAN_POINT ( 'NONE',  ( -4.556385078139999933, -95.60035679210000126, 22.08725204710000156 ) ) ;
#8907 = ORIENTED_EDGE ( 'NONE', *, *, #17445, .T. ) ;
#8908 = CARTESIAN_POINT ( 'NONE',  ( 23.60108036107897789, -92.61393927529991288, -19.31944997532723818 ) ) ;
#8909 = CARTESIAN_POINT ( 'NONE',  ( 26.37318040470000113, -92.84292488370000740, 13.16123784829999899 ) ) ;
#8910 = B_SPLINE_SURFACE_WITH_KNOTS ( 'NONE', 5, 5, ( 
 ( #20824, #1296, #27537, #3066, #886, #23436, #9728, #16444, #10139 ),
 ( #5787, #25347, #9591, #14261, #23154, #19058, #25622, #746, #5513 ),
 ( #7843, #1169, #20972, #3198, #12057, #18788, #14400, #23291, #12199 ),
 ( #21114, #10008, #16726, #3473, #23566, #3604, #12464, #17141, #5918 ),
 ( #28079, #8115, #26030, #1709, #8383, #6057, #26179, #10417, #1577 ),
 ( #10547, #14937, #6502, #17288, #19463, #28352, #21799, #14801, #23841 ) ),
 .UNSPECIFIED., .F., .F., .F.,
 ( 6, 6 ),
 ( 6, 3, 6 ),
 ( 112.4382702900000055, 122.9399824959999989 ),
 ( 0.000000000000000000, 1.000000000000000000, 2.000000000000000000 ),
 .UNSPECIFIED. ) ;
#8911 = CARTESIAN_POINT ( 'NONE',  ( 20.74932100510000055, -22.46373488209999891, -7.718703100189999944 ) ) ;
#8912 = CARTESIAN_POINT ( 'NONE',  ( 22.50268842703188099, -19.46928078220911473, 0.7888462583312775278 ) ) ;
#8913 = CARTESIAN_POINT ( 'NONE',  ( -7.139781038299999771, -101.0403179300000005, 13.72406621880000088 ) ) ;
#8914 = ORIENTED_EDGE ( 'NONE', *, *, #18709, .T. ) ;
#8915 = LINE ( 'NONE', #4419, #18040 ) ;
#8916 = CARTESIAN_POINT ( 'NONE',  ( -12.92645032892205137, -100.3617719037092400, -11.05940935245897627 ) ) ;
#8917 = CARTESIAN_POINT ( 'NONE',  ( 9.385544185329999678, -35.99604478260000207, -19.82171972309999930 ) ) ;
#8918 = CARTESIAN_POINT ( 'NONE',  ( -37.43882116139999994, -65.49083508809999898, -0.5420286502509998883 ) ) ;
#8919 = VERTEX_POINT ( 'NONE', #13429 ) ;
#8920 = CARTESIAN_POINT ( 'NONE',  ( 7.873312524909999333, -99.14867886189999524, 16.15069897069999882 ) ) ;
#8921 = CIRCLE ( 'NONE', #25254, 22.03370205219999889 ) ;
#8922 = EDGE_CURVE ( 'NONE', #21728, #2654, #17683, .T. ) ;
#8923 = CARTESIAN_POINT ( 'NONE',  ( 0.000000000000000000, -38.34400911419999858, 0.000000000000000000 ) ) ;
#8924 = CARTESIAN_POINT ( 'NONE',  ( 21.56931447779999900, -36.56979901409999911, -6.850353625240000355 ) ) ;
#8925 = CARTESIAN_POINT ( 'NONE',  ( 20.30102379280000235, -72.00000000000000000, -30.97095677779999789 ) ) ;
#8926 = ORIENTED_EDGE ( 'NONE', *, *, #6361, .F. ) ;
#8927 = CARTESIAN_POINT ( 'NONE',  ( -40.00000000000000000, -73.00000000000000000, 2.464695114669999848E-15 ) ) ;
#8928 = CONICAL_SURFACE ( 'NONE', #14532, 52.86371681419998936, 1.437659999240000097 ) ;
#8929 = CARTESIAN_POINT ( 'NONE',  ( -27.68682485439999752, -24.80000000000000071, -50.68039294919999804 ) ) ;
#8930 = CARTESIAN_POINT ( 'NONE',  ( 14.59338748251070506, -95.47757552516759461, 17.32730085737816950 ) ) ;
#8931 = DIRECTION ( 'NONE',  ( 0.4478680481951062275, 0.000000000000000000, 0.8940996652532120503 ) ) ;
#8932 = CARTESIAN_POINT ( 'NONE',  ( 26.37318901919999803, -93.00000450890000536, 13.16123549989999830 ) ) ;
#8933 = DIRECTION ( 'NONE',  ( -0.8981584475625417063, 0.000000000000000000, -0.4396719266362648648 ) ) ;
#8934 = DIRECTION ( 'NONE',  ( 0.4794255386042040601, 0.000000000000000000, 0.8775825618903720926 ) ) ;
#8935 = CARTESIAN_POINT ( 'NONE',  ( 23.00000922585108043, -93.86130746320593232, 12.91398536192384050 ) ) ;
#8936 = ORIENTED_EDGE ( 'NONE', *, *, #13271, .F. ) ;
#8937 = CARTESIAN_POINT ( 'NONE',  ( 36.26790001819999532, -74.59539775179999310, -15.00677268220000116 ) ) ;
#8938 = EDGE_CURVE ( 'NONE', #4316, #20825, #11384, .T. ) ;
#8939 = ADVANCED_FACE ( 'NONE', ( #7042 ), #20595, .F. ) ;
#8940 = ORIENTED_EDGE ( 'NONE', *, *, #6978, .F. ) ;
#8941 = CARTESIAN_POINT ( 'NONE',  ( -11.18243286969999950, -57.47855569860000458, 20.51090136460000224 ) ) ;
#8942 = CARTESIAN_POINT ( 'NONE',  ( 40.00000000000000000, -73.50000000000000000, -9.769962616700000205E-15 ) ) ;
#8943 = AXIS2_PLACEMENT_3D ( 'NONE', #2534, #13432, #356 ) ;
#8944 = CARTESIAN_POINT ( 'NONE',  ( -24.26314771630000067, -94.16701134380001292, -3.424815318739999892 ) ) ;
#8945 = AXIS2_PLACEMENT_3D ( 'NONE', #254, #9096, #22527 ) ;
#8946 = CARTESIAN_POINT ( 'NONE',  ( -19.77751067240000182, -52.59522851940000265, 14.14810317790000127 ) ) ;
#8947 = FACE_OUTER_BOUND ( 'NONE', #12800, .T. ) ;
#8948 = CARTESIAN_POINT ( 'NONE',  ( -11.67870406894427937, -57.47571038307907543, -20.30949878506913109 ) ) ;
#8949 = VERTEX_POINT ( 'NONE', #16780 ) ;
#8950 = DIRECTION ( 'NONE',  ( 1.000000000000000000, 0.000000000000000000, 0.000000000000000000 ) ) ;
#8951 = CARTESIAN_POINT ( 'NONE',  ( 7.260231713129999598, -73.74954830080000079, -39.69297836810000035 ) ) ;
#8952 = ORIENTED_EDGE ( 'NONE', *, *, #15580, .T. ) ;
#8953 = CARTESIAN_POINT ( 'NONE',  ( 7.894252205549937784, -92.54383083955175948, 29.46067132498288643 ) ) ;
#8954 = ORIENTED_EDGE ( 'NONE', *, *, #574, .F. ) ;
#8955 = DIRECTION ( 'NONE',  ( -0.3687499999999814260, 0.000000000000000000, 0.9295286103719527793 ) ) ;
#8956 = EDGE_CURVE ( 'NONE', #5288, #10781, #12680, .T. ) ;
#8957 = CARTESIAN_POINT ( 'NONE',  ( 19.98296175649999995, -94.98812477599999227, 14.17692170039999944 ) ) ;
#8958 = AXIS2_PLACEMENT_3D ( 'NONE', #14229, #27199, #7238 ) ;
#8959 = CARTESIAN_POINT ( 'NONE',  ( -9.461931989540000032, -18.50000000000000000, -20.21076900759999972 ) ) ;
#8960 = EDGE_CURVE ( 'NONE', #7866, #6381, #10914, .T. ) ;
#8961 = DIRECTION ( 'NONE',  ( 1.000000000000000000, 0.000000000000000000, 0.000000000000000000 ) ) ;
#8962 = CARTESIAN_POINT ( 'NONE',  ( 24.25366699300000306, -93.99830544900000007, -8.983265665619999396 ) ) ;
#8963 = ADVANCED_FACE ( 'NONE', ( #9789, #11970 ), #23618, .F. ) ;
#8964 = CARTESIAN_POINT ( 'NONE',  ( 4.500000000000000000, -15.00000000000000000, 40.50000000000000000 ) ) ;
#8965 = CARTESIAN_POINT ( 'NONE',  ( 8.873743607099997988, -64.92653621079999482, -23.73262392499999862 ) ) ;
#8966 = CARTESIAN_POINT ( 'NONE',  ( 14.04045377689999796, -98.83667233820000320, -12.27759081110000139 ) ) ;
#8967 = VERTEX_POINT ( 'NONE', #18839 ) ;
#8968 = CIRCLE ( 'NONE', #23866, 0.5000000000000027756 ) ;
#8969 = CARTESIAN_POINT ( 'NONE',  ( -3.252988965690000178, -72.00000000000000000, -30.32986301179999700 ) ) ;
#8970 = DIRECTION ( 'NONE',  ( 0.000000000000000000, 1.000000000000000000, 0.000000000000000000 ) ) ;
#8971 = CARTESIAN_POINT ( 'NONE',  ( -12.85008966630000060, -99.72202992580000114, -11.39236235390000118 ) ) ;
#8972 = EDGE_CURVE ( 'NONE', #1691, #22467, #3660, .T. ) ;
#8973 = CARTESIAN_POINT ( 'NONE',  ( 20.77309584335343118, -19.47370675685051111, 9.491263722772981026 ) ) ;
#8974 = CARTESIAN_POINT ( 'NONE',  ( -40.28438195539999356, -74.37144044069999893, -7.256982118399999848 ) ) ;
#8975 = VERTEX_POINT ( 'NONE', #1348 ) ;
#8976 = DIRECTION ( 'NONE',  ( 0.000000000000000000, 1.000000000000000000, 0.000000000000000000 ) ) ;
#8977 = VERTEX_POINT ( 'NONE', #23488 ) ;
#8978 = PRODUCT_DEFINITION_SHAPE ( 'NONE', 'NONE',  #28804 ) ;
#8979 = DIRECTION ( 'NONE',  ( 0.000000000000000000, 1.000000000000000000, 0.000000000000000000 ) ) ;
#8980 = CARTESIAN_POINT ( 'NONE',  ( 41.47915484300000344, -79.00000000000000000, -14.75000000000000000 ) ) ;
#8981 = CARTESIAN_POINT ( 'NONE',  ( 28.31007805460000171, -40.00000000000000000, 51.82125027960000097 ) ) ;
#8982 = CARTESIAN_POINT ( 'NONE',  ( -0.5436438173659999817, -58.35721741809999941, -23.39762436370000032 ) ) ;
#8983 = ORIENTED_EDGE ( 'NONE', *, *, #13648, .T. ) ;
#8984 = EDGE_LOOP ( 'NONE', ( #13670, #24173, #14841, #22842 ) ) ;
#8985 = CARTESIAN_POINT ( 'NONE',  ( -22.17562918277512907, -67.73307646828385487, 14.25710666000342108 ) ) ;
#8986 = CARTESIAN_POINT ( 'NONE',  ( 19.83535700790000078, -94.71481161159999829, 14.13921680270000003 ) ) ;
#8987 = DIRECTION ( 'NONE',  ( 0.05918472534689767084, 0.000000000000000000, -0.9982470477219616001 ) ) ;
#8988 = ORIENTED_EDGE ( 'NONE', *, *, #3312, .T. ) ;
#8989 = AXIS2_PLACEMENT_3D ( 'NONE', #10545, #24127, #26323 ) ;
#8990 = CARTESIAN_POINT ( 'NONE',  ( 22.01810471777381650, -19.15810975296247776, -0.4634306781688211641 ) ) ;
#8991 = CARTESIAN_POINT ( 'NONE',  ( -22.33048751989999658, -79.95649403670000765, -32.64088387420000004 ) ) ;
#8992 = ORIENTED_EDGE ( 'NONE', *, *, #27253, .F. ) ;
#8993 = FACE_OUTER_BOUND ( 'NONE', #1052, .T. ) ;
#8994 = ADVANCED_FACE ( 'NONE', ( #25262 ), #10061, .T. ) ;
#8995 = CARTESIAN_POINT ( 'NONE',  ( -12.45881531480000071, -94.16309976670001447, -20.99847364200000044 ) ) ;
#8996 = DIRECTION ( 'NONE',  ( 0.3687499999999814260, 0.000000000000000000, -0.9295286103719527793 ) ) ;
#8997 = ORIENTED_EDGE ( 'NONE', *, *, #834, .F. ) ;
#8998 = EDGE_CURVE ( 'NONE', #21862, #7753, #5742, .T. ) ;
#8999 = DIRECTION ( 'NONE',  ( 1.000000000000000000, 0.000000000000000000, 0.000000000000000000 ) ) ;
#9000 = CIRCLE ( 'NONE', #204, 7.250000000000000000 ) ;
#9001 = CARTESIAN_POINT ( 'NONE',  ( -16.94128954410000176, -99.70025030589999915, 2.976402637920000149 ) ) ;
#9002 = CARTESIAN_POINT ( 'NONE',  ( -39.07240670449999698, -73.87254094300001839, 7.323170304809999642 ) ) ;
#9003 = FACE_OUTER_BOUND ( 'NONE', #12213, .T. ) ;
#9004 = CARTESIAN_POINT ( 'NONE',  ( -5.736172046443546613, -98.20750306712106692, -19.47271301003372912 ) ) ;
#9005 = VECTOR ( 'NONE', #7549, 1000.000000000000114 ) ;
#9006 = CARTESIAN_POINT ( 'NONE',  ( -2.876553231629999985, -91.50000000000000000, -5.265495371340000119 ) ) ;
#9007 = ADVANCED_FACE ( 'NONE', ( #21030 ), #24183, .F. ) ;
#9008 = CYLINDRICAL_SURFACE ( 'NONE', #17868, 0.7500000000000003331 ) ;
#9009 = CARTESIAN_POINT ( 'NONE',  ( -17.73225090229999878, -18.50000000000000000, 12.18319217400000021 ) ) ;
#9010 = ORIENTED_EDGE ( 'NONE', *, *, #19339, .F. ) ;
#9011 = EDGE_CURVE ( 'NONE', #9424, #28497, #20969, .T. ) ;
#9012 = CARTESIAN_POINT ( 'NONE',  ( -10.80471582220000037, -93.74976927969998997, -23.35275943390000108 ) ) ;
#9013 = CARTESIAN_POINT ( 'NONE',  ( 9.315656985238685905, -37.99004392730040536, -22.70406351595718064 ) ) ;
#9014 = CARTESIAN_POINT ( 'NONE',  ( -24.08680547314210330, -92.61393927537839943, -18.71036994979779777 ) ) ;
#9015 = DIRECTION ( 'NONE',  ( 0.4794255386042036715, 0.000000000000000000, 0.8775825618903724257 ) ) ;
#9016 = CARTESIAN_POINT ( 'NONE',  ( 0.1125757948539710535, -92.93978723898268868, -30.49979579639168037 ) ) ;
#9017 = CIRCLE ( 'NONE', #25337, 2.000000494510000504 ) ;
#9018 = DIRECTION ( 'NONE',  ( 0.000000000000000000, 0.000000000000000000, 1.000000000000000000 ) ) ;
#9019 = LINE ( 'NONE', #13539, #19589 ) ;
#9020 = ORIENTED_EDGE ( 'NONE', *, *, #14726, .T. ) ;
#9021 = AXIS2_PLACEMENT_3D ( 'NONE', #14206, #18866, #3140 ) ;
#9022 = ORIENTED_EDGE ( 'NONE', *, *, #9610, .F. ) ;
#9023 = CIRCLE ( 'NONE', #9967, 21.14285714290000229 ) ;
#9024 = CARTESIAN_POINT ( 'NONE',  ( -13.40823022979999912, -49.82765297159999562, 20.56009738570000067 ) ) ;
#9025 = DIRECTION ( 'NONE',  ( 0.000000000000000000, -1.000000000000000000, 0.000000000000000000 ) ) ;
#9026 = ORIENTED_EDGE ( 'NONE', *, *, #3188, .T. ) ;
#9027 = DIRECTION ( 'NONE',  ( 0.000000000000000000, 1.000000000000000000, 0.000000000000000000 ) ) ;
#9028 = CARTESIAN_POINT ( 'NONE',  ( 9.038647564319999717, -35.72724395809999720, -19.55068592700000352 ) ) ;
#9029 = CARTESIAN_POINT ( 'NONE',  ( 6.640361864253258695, -93.59825775159440298, -26.19609744338800894 ) ) ;
#9030 = EDGE_CURVE ( 'NONE', #1569, #22412, #17220, .T. ) ;
#9031 = CARTESIAN_POINT ( 'NONE',  ( -27.85075384980000024, -92.68283714880000446, 2.027630021949999861 ) ) ;
#9032 = CARTESIAN_POINT ( 'NONE',  ( -19.98881959580000256, -95.75655295469999828, 10.31208380220000009 ) ) ;
#9033 = VECTOR ( 'NONE', #7517, 1000.000000000000000 ) ;
#9034 = CARTESIAN_POINT ( 'NONE',  ( -9.443564602020002141, -18.50000000000000000, -19.75225778540000121 ) ) ;
#9035 = VERTEX_POINT ( 'NONE', #14179 ) ;
#9036 = ADVANCED_FACE ( 'NONE', ( #27998 ), #28379, .F. ) ;
#9037 = CARTESIAN_POINT ( 'NONE',  ( -20.56694544386164125, -62.25036960902605898, 12.58271708036219572 ) ) ;
#9038 = CARTESIAN_POINT ( 'NONE',  ( 40.28268501200326313, -74.17548517097154104, 7.244487271046783583 ) ) ;
#9039 = EDGE_LOOP ( 'NONE', ( #5701, #12768, #770, #20697 ) ) ;
#9040 = CIRCLE ( 'NONE', #23494, 0.4999999999999988343 ) ;
#9041 = CARTESIAN_POINT ( 'NONE',  ( -37.82842046529857072, -63.32098627082129383, -0.7669639132331649289 ) ) ;
#9042 = CARTESIAN_POINT ( 'NONE',  ( -17.42719211919999722, -93.34960223970000470, 19.28404990989999845 ) ) ;
#9043 = CARTESIAN_POINT ( 'NONE',  ( 10.20110288159999890, -74.50000000000000000, 41.00000000000000000 ) ) ;
#9044 = ORIENTED_EDGE ( 'NONE', *, *, #10755, .T. ) ;
#9045 = EDGE_CURVE ( 'NONE', #17502, #28438, #16637, .T. ) ;
#9046 = CARTESIAN_POINT ( 'NONE',  ( 27.85911644260000131, -71.04728284579999809, 0.9189804863380000022 ) ) ;
#9047 = VECTOR ( 'NONE', #20764, 999.9999999999998863 ) ;
#9048 = CARTESIAN_POINT ( 'NONE',  ( 1.014221318129999938, -99.92384627689999377, -16.88077478359999972 ) ) ;
#9049 = CARTESIAN_POINT ( 'NONE',  ( 24.26411138551022262, -74.17203985465638993, -30.69540152489543772 ) ) ;
#9050 = FACE_OUTER_BOUND ( 'NONE', #18799, .T. ) ;
#9051 = CARTESIAN_POINT ( 'NONE',  ( 23.93313133829999728, -65.07443449820000581, -7.727578191800000162 ) ) ;
#9052 = CARTESIAN_POINT ( 'NONE',  ( 26.46310910940000127, -64.24504445130001784, 1.532420644259999909 ) ) ;
#9053 = CARTESIAN_POINT ( 'NONE',  ( 0.000000000000000000, -16.50000000000000000, 0.000000000000000000 ) ) ;
#9054 = EDGE_LOOP ( 'NONE', ( #15220, #8226 ) ) ;
#9055 = CARTESIAN_POINT ( 'NONE',  ( -2.741827597428787566, -18.87168151092993895, -24.31677555295371462 ) ) ;
#9056 = CARTESIAN_POINT ( 'NONE',  ( -42.71188834620000563, -65.41419836839999391, 0.4550164754559999913 ) ) ;
#9057 = TOROIDAL_SURFACE ( 'NONE', #12760, 38.75000000000000000, 0.5000000000000000000 ) ;
#9058 = CARTESIAN_POINT ( 'NONE',  ( 19.98296746440000149, -94.98812769030000425, 14.17693333179999904 ) ) ;
#9059 = ORIENTED_EDGE ( 'NONE', *, *, #24311, .T. ) ;
#9060 = CARTESIAN_POINT ( 'NONE',  ( 7.135467526410000261, -73.65707963269998970, 38.71641004229999794 ) ) ;
#9061 = CARTESIAN_POINT ( 'NONE',  ( 24.53438756210000093, -92.85282594270000800, 14.48885364650000085 ) ) ;
#9062 = CARTESIAN_POINT ( 'NONE',  ( -18.34989813179999985, -111.0000000000000000, 23.56346505449999995 ) ) ;
#9063 = DIRECTION ( 'NONE',  ( 0.000000000000000000, 1.000000000000000000, 0.000000000000000000 ) ) ;
#9064 = EDGE_LOOP ( 'NONE', ( #8175, #15911 ) ) ;
#9065 = CIRCLE ( 'NONE', #27699, 39.25000000000000000 ) ;
#9066 = CARTESIAN_POINT ( 'NONE',  ( 27.02630527335654165, -72.25875278531135848, -11.40251575530330008 ) ) ;
#9067 = CARTESIAN_POINT ( 'NONE',  ( -12.48345623946794269, -101.5740747342345855, -10.09958814640085478 ) ) ;
#9068 = ORIENTED_EDGE ( 'NONE', *, *, #1888, .F. ) ;
#9069 = CARTESIAN_POINT ( 'NONE',  ( 8.974207715069999480, -36.02836299580000201, -20.55125170219999831 ) ) ;
#9070 = CARTESIAN_POINT ( 'NONE',  ( 8.566533541336891489, -19.47798481066859111, -20.04266833404968651 ) ) ;
#9071 = EDGE_CURVE ( 'NONE', #300, #26598, #21165, .T. ) ;
#9072 = CARTESIAN_POINT ( 'NONE',  ( -15.55828293390000105, -101.1889999979999999, 3.733608462140000306 ) ) ;
#9073 = CARTESIAN_POINT ( 'NONE',  ( -36.70027262279481306, -63.05366291736164186, -0.03679144966704090552 ) ) ;
#9074 = DIRECTION ( 'NONE',  ( 0.000000000000000000, 1.000000000000000000, 0.000000000000000000 ) ) ;
#9075 = CARTESIAN_POINT ( 'NONE',  ( -2.641585765738330593, -19.49371746075303236, -23.93965455194797443 ) ) ;
#9076 = ORIENTED_EDGE ( 'NONE', *, *, #14169, .F. ) ;
#9077 = CARTESIAN_POINT ( 'NONE',  ( 11.85391586600000124, -101.4309749570000037, -10.98895622390000071 ) ) ;
#9078 = CARTESIAN_POINT ( 'NONE',  ( 28.25259359185359642, -69.84715190613960090, 2.434813837803762926 ) ) ;
#9079 = CARTESIAN_POINT ( 'NONE',  ( -18.99420542959347458, -98.09459568842703447, -7.570339228046596425 ) ) ;
#9080 = DIRECTION ( 'NONE',  ( 0.000000000000000000, -1.000000000000000000, 0.000000000000000000 ) ) ;
#9081 = TOROIDAL_SURFACE ( 'NONE', #12343, 19.50000000000000000, 3.000000000000000000 ) ;
#9082 = CARTESIAN_POINT ( 'NONE',  ( 20.33566493080000015, -36.00000000000000000, -9.885503730140001721 ) ) ;
#9083 = DIRECTION ( 'NONE',  ( 0.2414462220490750377, 0.000000000000000000, -0.9704142011833034598 ) ) ;
#9084 = CARTESIAN_POINT ( 'NONE',  ( 5.326862811529999898E-15, -74.50000000000000000, -47.25000000000000000 ) ) ;
#9085 = CARTESIAN_POINT ( 'NONE',  ( 15.19718069640000024, -101.1364147039999892, 2.131293228500000581 ) ) ;
#9086 = CARTESIAN_POINT ( 'NONE',  ( 25.08528495285458249, -93.39299082550714104, 11.62361772614930722 ) ) ;
#9087 = ORIENTED_EDGE ( 'NONE', *, *, #14642, .F. ) ;
#9088 = CARTESIAN_POINT ( 'NONE',  ( -32.61798281429999946, -80.00000000000000000, -22.71848787769999944 ) ) ;
#9089 = ORIENTED_EDGE ( 'NONE', *, *, #22791, .T. ) ;
#9090 = CARTESIAN_POINT ( 'NONE',  ( -14.55866013589999852, -64.24504477300000360, 22.15151183529999912 ) ) ;
#9091 = EDGE_CURVE ( 'NONE', #23386, #19780, #6080, .T. ) ;
#9092 = CYLINDRICAL_SURFACE ( 'NONE', #24402, 0.7499999999999992228 ) ;
#9093 = DIRECTION ( 'NONE',  ( 0.000000000000000000, -1.000000000000000000, 0.000000000000000000 ) ) ;
#9094 = CARTESIAN_POINT ( 'NONE',  ( 26.62370195355942570, -72.37489743482117888, 10.79038948701335698 ) ) ;
#9095 = CARTESIAN_POINT ( 'NONE',  ( 21.55953482829999857, -36.72040100929999795, -8.607507078249998500 ) ) ;
#9096 = DIRECTION ( 'NONE',  ( 0.000000000000000000, -1.000000000000000000, 0.000000000000000000 ) ) ;
#9097 = CARTESIAN_POINT ( 'NONE',  ( 16.44163546059999703, -100.2522625769999962, 4.388208817439999798 ) ) ;
#9098 = ORIENTED_EDGE ( 'NONE', *, *, #23782, .T. ) ;
#9099 = CARTESIAN_POINT ( 'NONE',  ( -7.260602597430000138, -73.82497517469998627, -39.64142120219999299 ) ) ;
#9100 = CARTESIAN_POINT ( 'NONE',  ( -19.72803626430000179, -96.95622423829999548, -6.895699102770000977 ) ) ;
#9101 = ORIENTED_EDGE ( 'NONE', *, *, #9011, .T. ) ;
#9102 = CARTESIAN_POINT ( 'NONE',  ( -1.604070449259999753, -100.9197075889999979, -15.54198650660000069 ) ) ;
#9103 = ORIENTED_EDGE ( 'NONE', *, *, #11114, .T. ) ;
#9104 = EDGE_CURVE ( 'NONE', #13461, #28257, #22348, .T. ) ;
#9105 = EDGE_CURVE ( 'NONE', #20556, #2020, #6264, .T. ) ;
#9106 = CARTESIAN_POINT ( 'NONE',  ( 23.96368475870000125, -93.00000000000000000, 8.717328305520000598 ) ) ;
#9107 = DIRECTION ( 'NONE',  ( 0.000000000000000000, -1.000000000000000000, 0.000000000000000000 ) ) ;
#9108 = CARTESIAN_POINT ( 'NONE',  ( 20.09790167590000109, -39.36582103100000296, 10.61942201829999988 ) ) ;
#9109 = AXIS2_PLACEMENT_3D ( 'NONE', #14442, #22920, #16490 ) ;
#9110 = DIRECTION ( 'NONE',  ( 1.000000000000000000, 0.000000000000000000, 0.000000000000000000 ) ) ;
#9111 = CARTESIAN_POINT ( 'NONE',  ( -7.248796347617021851, -73.89318255918183809, -39.86740956960665727 ) ) ;
#9112 = CARTESIAN_POINT ( 'NONE',  ( 19.24535105649999878, -18.85523519099999845, 10.43937572179999940 ) ) ;
#9113 = CARTESIAN_POINT ( 'NONE',  ( 9.444162208259999858, -68.01046952510000665, -24.98417836379999812 ) ) ;
#9114 = CARTESIAN_POINT ( 'NONE',  ( -17.31257399851914869, -96.95293637055524982, 11.43669896296266586 ) ) ;
#9115 = VERTEX_POINT ( 'NONE', #10601 ) ;
#9116 = DIRECTION ( 'NONE',  ( 0.000000000000000000, 1.000000000000000000, 0.000000000000000000 ) ) ;
#9117 = CARTESIAN_POINT ( 'NONE',  ( -3.663740619795967213, -98.56104012213324950, 19.49859454066769970 ) ) ;
#9118 = CARTESIAN_POINT ( 'NONE',  ( -12.53380938399999955, -99.91102932029998840, -11.37771751150000021 ) ) ;
#9119 = CARTESIAN_POINT ( 'NONE',  ( 21.70557149514094064, -19.48733830550655100, 9.545844344095677059 ) ) ;
#9120 = CARTESIAN_POINT ( 'NONE',  ( -40.37851622809999697, -74.24288085059998821, -7.248115061070000031 ) ) ;
#9121 = ORIENTED_EDGE ( 'NONE', *, *, #14883, .F. ) ;
#9122 = CARTESIAN_POINT ( 'NONE',  ( 27.12516731730879371, -92.50638022835022412, -13.94618822762715027 ) ) ;
#9123 = ORIENTED_EDGE ( 'NONE', *, *, #1753, .T. ) ;
#9124 = EDGE_CURVE ( 'NONE', #6872, #10217, #933, .T. ) ;
#9125 = CARTESIAN_POINT ( 'NONE',  ( -26.69328098980000163, -79.50000000000000000, -35.88566914520000495 ) ) ;
#9126 = CARTESIAN_POINT ( 'NONE',  ( 14.95019707169999990, -101.2530993000000024, 2.710463435110000319 ) ) ;
#9127 = CARTESIAN_POINT ( 'NONE',  ( 19.55068592539999983, -35.72724453810000256, -9.038647860560001135 ) ) ;
#9128 = CARTESIAN_POINT ( 'NONE',  ( 7.999597942409999440, -93.06863555389999476, 27.33126122210000020 ) ) ;
#9129 = EDGE_LOOP ( 'NONE', ( #6200, #4743, #4247, #13492, #6941, #26920 ) ) ;
#9130 = VERTEX_POINT ( 'NONE', #1908 ) ;
#9131 = CARTESIAN_POINT ( 'NONE',  ( -22.99750611650443233, -71.51406819562529904, 16.12010929920209179 ) ) ;
#9132 = CARTESIAN_POINT ( 'NONE',  ( 20.29323830529999739, -94.22763361239999824, 13.32192879709999822 ) ) ;
#9133 = CARTESIAN_POINT ( 'NONE',  ( 45.84677419350000349, -73.65707963269998970, -4.286925650119999709 ) ) ;
#9134 = ADVANCED_FACE ( 'NONE', ( #19947 ), #10750, .F. ) ;
#9135 = ORIENTED_EDGE ( 'NONE', *, *, #7942, .F. ) ;
#9136 = CARTESIAN_POINT ( 'NONE',  ( 16.54057195470140584, -94.89197151649931072, 16.94454422099984114 ) ) ;
#9137 = DIRECTION ( 'NONE',  ( 0.000000000000000000, 1.000000000000000000, 0.000000000000000000 ) ) ;
#9138 = CARTESIAN_POINT ( 'NONE',  ( 12.39757656149999931, -101.5369810359999860, -10.11435096289999969 ) ) ;
#9139 = CARTESIAN_POINT ( 'NONE',  ( -11.69298206670000084, -94.57749572790000059, -21.18607573959999968 ) ) ;
#9140 = DIRECTION ( 'NONE',  ( 1.000000000000000000, 0.000000000000000000, 0.000000000000000000 ) ) ;
#9141 = CARTESIAN_POINT ( 'NONE',  ( -17.94180966909999597, -18.50000000000000000, 18.81731824139999887 ) ) ;
#9142 = CARTESIAN_POINT ( 'NONE',  ( -2.788137124389999943, -64.22080823580000697, -26.35245158480000072 ) ) ;
#9143 = DIRECTION ( 'NONE',  ( 0.4794255386042040601, 0.000000000000000000, 0.8775825618903720926 ) ) ;
#9144 = CARTESIAN_POINT ( 'NONE',  ( -21.99191923020000061, -74.04938808419998963, -32.26547628159999448 ) ) ;
#9145 = CARTESIAN_POINT ( 'NONE',  ( -11.31667057079999950, -95.23931402160000914, -21.36056405359999744 ) ) ;
#9146 = CARTESIAN_POINT ( 'NONE',  ( 21.71672445440000132, -36.72346566049999694, -8.838003628720001004 ) ) ;
#9147 = CARTESIAN_POINT ( 'NONE',  ( 47.25000000000000000, -74.00000000000000000, -14.75000000000000000 ) ) ;
#9148 = CARTESIAN_POINT ( 'NONE',  ( -18.77305955369999779, -19.15810970359999743, 11.51451047569999808 ) ) ;
#9149 = ORIENTED_EDGE ( 'NONE', *, *, #14459, .F. ) ;
#9150 = FACE_OUTER_BOUND ( 'NONE', #2143, .T. ) ;
#9151 = CARTESIAN_POINT ( 'NONE',  ( 22.17953390099999922, -65.07443087359999367, 11.85657298630000156 ) ) ;
#9152 = CARTESIAN_POINT ( 'NONE',  ( -24.64364036189999752, -92.50000000000000000, -17.97055897050000084 ) ) ;
#9153 = CARTESIAN_POINT ( 'NONE',  ( -8.209463884390000743, -99.53431386179998697, 15.35748973489999969 ) ) ;
#9154 = CARTESIAN_POINT ( 'NONE',  ( 46.25000000000000000, -80.00000000000000000, -4.582575694960000057 ) ) ;
#9155 = B_SPLINE_SURFACE_WITH_KNOTS ( 'NONE', 5, 5, ( 
 ( #4864, #15920, #24826, #6613, #13440, #11543 ),
 ( #15625, #11396, #4713, #13745, #224, #521 ),
 ( #9367, #22501, #2687, #8920, #22645, #28733 ),
 ( #26725, #18269, #7201, #16067, #2393, #5000 ),
 ( #24969, #13890, #10943, #8770, #13294, #17685 ),
 ( #15473, #6764, #24525, #24382, #4423, #22198 ) ),
 .UNSPECIFIED., .F., .F., .F.,
 ( 6, 6 ),
 ( 6, 6 ),
 ( 15.82800262790000012, 19.56549066489999689 ),
 ( 0.000000000000000000, 0.5000000000000000000 ),
 .UNSPECIFIED. ) ;
#9156 = CARTESIAN_POINT ( 'NONE',  ( 0.000000000000000000, 0.000000000000000000, 0.000000000000000000 ) ) ;
#9157 = CARTESIAN_POINT ( 'NONE',  ( -11.69946357949999971, -63.04983560140001231, -23.02234151810000284 ) ) ;
#9158 = DIRECTION ( 'NONE',  ( 1.000000000000000000, 0.000000000000000000, 0.000000000000000000 ) ) ;
#9159 = EDGE_CURVE ( 'NONE', #17829, #14525, #15796, .T. ) ;
#9160 = ORIENTED_EDGE ( 'NONE', *, *, #1196, .T. ) ;
#9161 = VECTOR ( 'NONE', #8211, 1000.000000000000000 ) ;
#9162 = CARTESIAN_POINT ( 'NONE',  ( -12.04650752959999949, -69.29982884310000202, -25.46956806489999892 ) ) ;
#9163 = VERTEX_POINT ( 'NONE', #10469 ) ;
#9164 = CARTESIAN_POINT ( 'NONE',  ( -12.06159284910000018, -57.47122623870000524, 20.23241278190000259 ) ) ;
#9165 = CYLINDRICAL_SURFACE ( 'NONE', #9290, 0.7500000000000001110 ) ;
#9166 = EDGE_CURVE ( 'NONE', #24375, #26844, #11614, .T. ) ;
#9167 = ORIENTED_EDGE ( 'NONE', *, *, #19606, .F. ) ;
#9168 = CIRCLE ( 'NONE', #17082, 38.75000000000000000 ) ;
#9169 = DIRECTION ( 'NONE',  ( 1.000000000000000000, 0.000000000000000000, 8.344173797130000142E-16 ) ) ;
#9170 = EDGE_CURVE ( 'NONE', #6525, #16368, #16538, .T. ) ;
#9171 = CIRCLE ( 'NONE', #7356, 10.00000000000000000 ) ;
#9172 = DIRECTION ( 'NONE',  ( 0.000000000000000000, -1.000000000000000000, 0.000000000000000000 ) ) ;
#9173 = CARTESIAN_POINT ( 'NONE',  ( 1.338287881580000116, -94.89420189149998919, 24.43791688079999957 ) ) ;
#9174 = CARTESIAN_POINT ( 'NONE',  ( -18.83859341579999835, -97.73640017439998928, 6.587273628740000220 ) ) ;
#9175 = DIRECTION ( 'NONE',  ( 0.000000000000000000, 1.000000000000000000, 0.000000000000000000 ) ) ;
#9176 = CARTESIAN_POINT ( 'NONE',  ( 23.67408170059999861, -68.20869413019998717, 12.08289283440000084 ) ) ;
#9177 = ORIENTED_EDGE ( 'NONE', *, *, #24416, .F. ) ;
#9178 = DIRECTION ( 'NONE',  ( 1.000000000000000000, 0.000000000000000000, 0.000000000000000000 ) ) ;
#9179 = CARTESIAN_POINT ( 'NONE',  ( -19.97968670135914238, -58.31251141496787938, 12.16213319773063795 ) ) ;
#9180 = CARTESIAN_POINT ( 'NONE',  ( -13.30251043199831607, -92.87422005961661853, 27.44619162654865363 ) ) ;
#9181 = ORIENTED_EDGE ( 'NONE', *, *, #2237, .T. ) ;
#9182 = LINE ( 'NONE', #16040, #17411 ) ;
#9183 = CARTESIAN_POINT ( 'NONE',  ( -15.21475366910000027, -92.78573964340000657, 25.08891424309999962 ) ) ;
#9184 = CARTESIAN_POINT ( 'NONE',  ( -22.52693219800000080, -70.43934371539999972, 17.54847698860000094 ) ) ;
#9185 = ORIENTED_EDGE ( 'NONE', *, *, #14536, .F. ) ;
#9186 = AXIS2_PLACEMENT_3D ( 'NONE', #18705, #3396, #21037 ) ;
#9187 = CARTESIAN_POINT ( 'NONE',  ( -16.97218413830000117, -98.25999569910000275, 8.877871485000001783 ) ) ;
#9188 = CARTESIAN_POINT ( 'NONE',  ( -12.94585355959999973, -101.6484611540000031, -9.402386697720000797 ) ) ;
#9189 = CARTESIAN_POINT ( 'NONE',  ( -20.19582590579999959, -52.57401960330000179, 14.62459034920000001 ) ) ;
#9190 = CARTESIAN_POINT ( 'NONE',  ( 9.307782790770000148, -57.43039233030000190, -22.95932714879999992 ) ) ;
#9191 = DIRECTION ( 'NONE',  ( 0.000000000000000000, 1.000000000000000000, 0.000000000000000000 ) ) ;
#9192 = CARTESIAN_POINT ( 'NONE',  ( 23.16689931189999641, -60.33770510349999938, -9.368374202520000082 ) ) ;
#9193 = CARTESIAN_POINT ( 'NONE',  ( 6.977349081829999911, -99.61736775859999682, 15.87966916429999920 ) ) ;
#9194 = FACE_OUTER_BOUND ( 'NONE', #7333, .T. ) ;
#9195 = EDGE_CURVE ( 'NONE', #2845, #4012, #9781, .T. ) ;
#9196 = ORIENTED_EDGE ( 'NONE', *, *, #10842, .T. ) ;
#9197 = CARTESIAN_POINT ( 'NONE',  ( 27.96987275368786285, -92.54893169919633067, 12.16290556786634092 ) ) ;
#9198 = CARTESIAN_POINT ( 'NONE',  ( -42.89961768690000099, -65.31510159580000163, 0.3466308900760000089 ) ) ;
#9199 = CARTESIAN_POINT ( 'NONE',  ( 8.042002709780000202, -100.9405346150000042, 13.76814507859999814 ) ) ;
#9200 = VERTEX_POINT ( 'NONE', #12803 ) ;
#9201 = CARTESIAN_POINT ( 'NONE',  ( 7.219524535890000649, -73.62955962630000784, 39.18053445169999804 ) ) ;
#9202 = CARTESIAN_POINT ( 'NONE',  ( 9.374849370119999747, -94.98812477599999227, -22.63660903319999562 ) ) ;
#9203 = ADVANCED_FACE ( 'NONE', ( #21713 ), #15320, .T. ) ;
#9204 = CIRCLE ( 'NONE', #18063, 18.64285714289999873 ) ;
#9205 = CARTESIAN_POINT ( 'NONE',  ( 16.73195129730000374, -84.25000000000000000, 30.62763141000000289 ) ) ;
#9206 = CARTESIAN_POINT ( 'NONE',  ( -7.091440874569999941, -101.0151300849999814, 13.93786069769999969 ) ) ;
#9207 = DIRECTION ( 'NONE',  ( 0.000000000000000000, 1.000000000000000000, 0.000000000000000000 ) ) ;
#9208 = CARTESIAN_POINT ( 'NONE',  ( 9.140991624659999815, -36.03656764800000190, -20.50715178119999749 ) ) ;
#9209 = CARTESIAN_POINT ( 'NONE',  ( -36.87700573890000300, -65.19264941160000149, -0.2176643648609999926 ) ) ;
#9210 = EDGE_LOOP ( 'NONE', ( #8252, #6860, #20175, #20035, #23758, #17120, #14073, #10432, #10268, #23100, #11492, #13291, #10266, #15445, #14747, #27980, #3354, #573, #14927, #8325, #3661, #27949, #24632 ) ) ;
#9211 = LINE ( 'NONE', #26867, #27212 ) ;
#9212 = CARTESIAN_POINT ( 'NONE',  ( -36.70952836055239032, -63.05597747387601970, -0.07115400841154578826 ) ) ;
#9213 = FACE_OUTER_BOUND ( 'NONE', #19948, .T. ) ;
#9214 = FACE_OUTER_BOUND ( 'NONE', #10125, .T. ) ;
#9215 = CARTESIAN_POINT ( 'NONE',  ( -5.873418876839999747, -101.3150700380000018, 15.15334698740000086 ) ) ;
#9216 = ORIENTED_EDGE ( 'NONE', *, *, #24144, .F. ) ;
#9217 = CARTESIAN_POINT ( 'NONE',  ( -15.42928178740000078, -101.3399685459999944, 4.712812228389999802 ) ) ;
#9218 = CARTESIAN_POINT ( 'NONE',  ( -13.32719578240000047, -19.17999174859999911, 20.00777489529999897 ) ) ;
#9219 = CARTESIAN_POINT ( 'NONE',  ( -18.19446509544315660, -98.56104011354675265, -7.910728455679111093 ) ) ;
#9220 = CARTESIAN_POINT ( 'NONE',  ( -38.25843370903133689, -63.06504043303794305, -2.752751128791679491 ) ) ;
#9221 = B_SPLINE_CURVE_WITH_KNOTS ( 'NONE', 3,
 ( #417, #18167, #4615, #11140, #13491, #10985 ),
 .UNSPECIFIED., .F., .F.,
 ( 4, 2, 4 ),
 ( 0.000000000000000000, 0.5000000000000000000, 1.000000000000000000 ),
 .UNSPECIFIED. ) ;
#9222 = CARTESIAN_POINT ( 'NONE',  ( 25.67981836682682939, -61.04156242073475624, 1.397343546619608690 ) ) ;
#9223 = DIRECTION ( 'NONE',  ( 0.000000000000000000, 1.000000000000000000, 0.000000000000000000 ) ) ;
#9224 = DIRECTION ( 'NONE',  ( 0.000000000000000000, 1.000000000000000000, 0.000000000000000000 ) ) ;
#9225 = CARTESIAN_POINT ( 'NONE',  ( -10.54576762539999990, -18.85523517670000260, 19.18725863699999934 ) ) ;
#9226 = ORIENTED_EDGE ( 'NONE', *, *, #565, .F. ) ;
#9227 = CARTESIAN_POINT ( 'NONE',  ( 36.37866372090000056, -74.74623938790000466, -14.83127960650000077 ) ) ;
#9228 = CIRCLE ( 'NONE', #12926, 4.499999999999997335 ) ;
#9229 = AXIS2_PLACEMENT_3D ( 'NONE', #18409, #24515, #16201 ) ;
#9230 = CARTESIAN_POINT ( 'NONE',  ( 7.797483723290000057, -101.0407491870000030, 13.41348730009999990 ) ) ;
#9231 = ADVANCED_FACE ( 'NONE', ( #6563 ), #8170, .F. ) ;
#9232 = VERTEX_POINT ( 'NONE', #25948 ) ;
#9233 = DIRECTION ( 'NONE',  ( 1.000000000000000000, 0.000000000000000000, 0.000000000000000000 ) ) ;
#9234 = CARTESIAN_POINT ( 'NONE',  ( -13.94341442410000020, -60.21477618889999661, 21.38633822419999930 ) ) ;
#9235 = DIRECTION ( 'NONE',  ( 1.000000000000000000, 0.000000000000000000, 0.000000000000000000 ) ) ;
#9236 = B_SPLINE_CURVE_WITH_KNOTS ( 'NONE', 3,
 ( #14189, #3400, #5580, #7503, #3268, #25410, #25542, #20896, #12268, #27455, #1231, #5440, #23357, #20755, #21177, #11692, #664, #18561 ),
 .UNSPECIFIED., .F., .F.,
 ( 4, 2, 2, 2, 2, 2, 2, 2, 4 ),
 ( 0.000000000000000000, 0.1249999999999764633, 0.1874999999999647504, 0.2499999999999531486, 0.4999999999999553690, 0.6249999999999564793, 0.6874999999999633626, 0.7499999999999702460, 1.000000000000000000 ),
 .UNSPECIFIED. ) ;
#9237 = FACE_OUTER_BOUND ( 'NONE', #15719, .T. ) ;
#9238 = EDGE_CURVE ( 'NONE', #17644, #21056, #26591, .T. ) ;
#9239 = CARTESIAN_POINT ( 'NONE',  ( 21.77931243370000303, -37.33301741199999668, -8.479935121490001393 ) ) ;
#9240 = CARTESIAN_POINT ( 'NONE',  ( -12.01098287860592428, -65.44960518625730117, -24.07027922927386854 ) ) ;
#9241 = ADVANCED_FACE ( 'NONE', ( #27262 ), #13544, .T. ) ;
#9242 = CARTESIAN_POINT ( 'NONE',  ( 16.58138552489999995, -99.94751438429999268, 4.403722473940000270 ) ) ;
#9243 = VERTEX_POINT ( 'NONE', #7300 ) ;
#9244 = CARTESIAN_POINT ( 'NONE',  ( -7.215414233289999757, -74.50000000000000000, -40.70731707320000226 ) ) ;
#9245 = CARTESIAN_POINT ( 'NONE',  ( 30.65972643183915736, -74.17589974682529430, -24.31452029874836995 ) ) ;
#9246 = CARTESIAN_POINT ( 'NONE',  ( -20.03336705960000330, -97.14975611010000023, -7.249356197820000069 ) ) ;
#9247 = ORIENTED_EDGE ( 'NONE', *, *, #13823, .T. ) ;
#9248 = DIRECTION ( 'NONE',  ( -0.9620897310213631926, 2.431777862510916489E-14, 0.2727331103171030668 ) ) ;
#9249 = VERTEX_POINT ( 'NONE', #17784 ) ;
#9250 = AXIS2_PLACEMENT_3D ( 'NONE', #18043, #15694, #7126 ) ;
#9251 = VECTOR ( 'NONE', #24279, 1000.000000000000000 ) ;
#9252 = CARTESIAN_POINT ( 'NONE',  ( -4.500000000000000000, -12.50000000000000000, -40.50000000000000000 ) ) ;
#9253 = B_SPLINE_CURVE_WITH_KNOTS ( 'NONE', 3,
 ( #13559, #2508, #9329, #27130, #11363, #15890, #24797, #2801, #4834, #13712, #11509, #20416, #18234, #7170, #16036, #24941, #4970, #13856, #11655, #18952 ),
 .UNSPECIFIED., .F., .F.,
 ( 4, 2, 1, 2, 2, 2, 2, 1, 2, 2, 4 ),
 ( 0.000000000000000000, 0.1249999999999999722, 0.1874999999999996669, 0.2187500000000030254, 0.2500000000000064393, 0.5000000000000230926, 0.6250000000000311973, 0.6875000000000350830, 0.7187500000000430767, 0.7500000000000509592, 1.000000000000000000 ),
 .UNSPECIFIED. ) ;
#9254 = FACE_OUTER_BOUND ( 'NONE', #3687, .T. ) ;
#9255 = AXIS2_PLACEMENT_3D ( 'NONE', #14287, #5261, #5676 ) ;
#9256 = LINE ( 'NONE', #24863, #22994 ) ;
#9257 = CARTESIAN_POINT ( 'NONE',  ( 8.235816542629999560E-15, -69.00000000000000000, -40.00000000000000000 ) ) ;
#9258 = CARTESIAN_POINT ( 'NONE',  ( -7.246150394362209646, -73.82038814077014877, -39.74699101873454055 ) ) ;
#9259 = CARTESIAN_POINT ( 'NONE',  ( 19.77433184639999908, -18.50000000000000000, 8.671591744060000551 ) ) ;
#9260 = CARTESIAN_POINT ( 'NONE',  ( 9.895942579337763334, -99.82488179753744362, 13.91669341782708003 ) ) ;
#9261 = CARTESIAN_POINT ( 'NONE',  ( 13.96412840480000028, -99.57787118740000665, -10.31025271900000106 ) ) ;
#9262 = ORIENTED_EDGE ( 'NONE', *, *, #13652, .F. ) ;
#9263 = CARTESIAN_POINT ( 'NONE',  ( -12.02287215850000024, -69.84851671149999675, -25.68298794020000031 ) ) ;
#9264 = DIRECTION ( 'NONE',  ( -1.000000000000000000, 0.000000000000000000, 0.000000000000000000 ) ) ;
#9265 = CARTESIAN_POINT ( 'NONE',  ( -13.25319097760000098, -99.78393592979999482, -11.15464849200000153 ) ) ;
#9266 = CARTESIAN_POINT ( 'NONE',  ( -12.96048168789999977, -101.0356131030000029, -8.456406562079997968 ) ) ;
#9267 = CARTESIAN_POINT ( 'NONE',  ( 23.28519330966129530, -63.31588098632251160, -7.446352683915099746 ) ) ;
#9268 = EDGE_LOOP ( 'NONE', ( #18120, #21821 ) ) ;
#9269 = AXIS2_PLACEMENT_3D ( 'NONE', #7983, #23569, #18240 ) ;
#9270 = DIRECTION ( 'NONE',  ( -1.000000000000000000, 0.000000000000000000, 0.000000000000000000 ) ) ;
#9271 = ORIENTED_EDGE ( 'NONE', *, *, #8094, .F. ) ;
#9272 = AXIS2_PLACEMENT_3D ( 'NONE', #4115, #7332, #22487 ) ;
#9273 = AXIS2_PLACEMENT_3D ( 'NONE', #8734, #17651, #24646 ) ;
#9274 = EDGE_CURVE ( 'NONE', #26586, #10144, #14874, .T. ) ;
#9275 = DIRECTION ( 'NONE',  ( 0.7071067811865492381, 0.000000000000000000, -0.7071067811865457964 ) ) ;
#9276 = CARTESIAN_POINT ( 'NONE',  ( -4.592948295220000254, -99.60591459110000301, 16.75688848409999920 ) ) ;
#9277 = CARTESIAN_POINT ( 'NONE',  ( 4.027230326479999789, -93.61421867219999626, 26.02828154170000019 ) ) ;
#9278 = VERTEX_POINT ( 'NONE', #18222 ) ;
#9279 = ORIENTED_EDGE ( 'NONE', *, *, #21910, .F. ) ;
#9280 = CARTESIAN_POINT ( 'NONE',  ( -22.90496460322411565, -70.97967975433614640, 15.82655954324508762 ) ) ;
#9281 = DIRECTION ( 'NONE',  ( 0.000000000000000000, -1.000000000000000000, 0.000000000000000000 ) ) ;
#9282 = CARTESIAN_POINT ( 'NONE',  ( 47.09727354990000237, -74.46036430799999550, -1.896414880740000086 ) ) ;
#9283 = ORIENTED_EDGE ( 'NONE', *, *, #6468, .F. ) ;
#9284 = FACE_OUTER_BOUND ( 'NONE', #14019, .T. ) ;
#9285 = CARTESIAN_POINT ( 'NONE',  ( -11.44396836898854986, -61.24981953521358236, 20.93040142220293731 ) ) ;
#9286 = CARTESIAN_POINT ( 'NONE',  ( 8.971065451009998526, -36.23955850699999814, -21.20403844530000015 ) ) ;
#9287 = CARTESIAN_POINT ( 'NONE',  ( -11.80897031970000022, -94.89419905519999077, -21.43712780819999963 ) ) ;
#9288 = LINE ( 'NONE', #24900, #9655 ) ;
#9289 = VERTEX_POINT ( 'NONE', #2646 ) ;
#9290 = AXIS2_PLACEMENT_3D ( 'NONE', #2788, #13701, #26672 ) ;
#9291 = CONICAL_SURFACE ( 'NONE', #11615, 25.14975229270001833, 0.4276056667390000787 ) ;
#9292 = CARTESIAN_POINT ( 'NONE',  ( 36.34100412979999817, -74.29447080869999809, -14.83252444919999924 ) ) ;
#9293 = CARTESIAN_POINT ( 'NONE',  ( 13.81202799179999907, -99.83167681540000160, -10.46592613740000210 ) ) ;
#9294 = CARTESIAN_POINT ( 'NONE',  ( -40.70731707320000226, -74.50000000000000000, 7.215414233289999757 ) ) ;
#9295 = CARTESIAN_POINT ( 'NONE',  ( -21.60034937969999902, -74.50000000000000000, -32.77174707999999725 ) ) ;
#9296 = EDGE_CURVE ( 'NONE', #21931, #11437, #17924, .T. ) ;
#9297 = ORIENTED_EDGE ( 'NONE', *, *, #26606, .T. ) ;
#9298 = DIRECTION ( 'NONE',  ( 1.000000000000000000, 0.000000000000000000, 0.000000000000000000 ) ) ;
#9299 = LINE ( 'NONE', #24610, #5323 ) ;
#9300 = CARTESIAN_POINT ( 'NONE',  ( -17.90071848410000399, -18.50000000000000000, 11.63286205439999854 ) ) ;
#9301 = EDGE_LOOP ( 'NONE', ( #25213, #20498, #23248, #20666, #25527 ) ) ;
#9302 = CARTESIAN_POINT ( 'NONE',  ( -13.16777714140000022, -93.19477243160000057, -23.58326759370000048 ) ) ;
#9303 = LINE ( 'NONE', #26402, #26080 ) ;
#9304 = CARTESIAN_POINT ( 'NONE',  ( 16.47431367404465519, -100.3266728692175604, 4.354304509586214067 ) ) ;
#9305 = CARTESIAN_POINT ( 'NONE',  ( 36.70830950850000107, -75.00000000000000000, -14.75000000000000000 ) ) ;
#9306 = ORIENTED_EDGE ( 'NONE', *, *, #20238, .T. ) ;
#9307 = CARTESIAN_POINT ( 'NONE',  ( 46.12332287689999788, -80.00000000000000000, -4.489694494070000097 ) ) ;
#9308 = DIRECTION ( 'NONE',  ( 0.000000000000000000, -1.000000000000000000, 0.000000000000000000 ) ) ;
#9309 = APPLICATION_PROTOCOL_DEFINITION ( 'draft international standard', 'automotive_design', 1998, #14444 ) ;
#9310 = CARTESIAN_POINT ( 'NONE',  ( -11.29976941730000028, -60.38561542509999924, -21.91412512930000034 ) ) ;
#9311 = CIRCLE ( 'NONE', #9796, 55.67692378859999991 ) ;
#9312 = CARTESIAN_POINT ( 'NONE',  ( 26.88013656499999726, -70.45756452349999677, -11.38838362379999936 ) ) ;
#9313 = CARTESIAN_POINT ( 'NONE',  ( 2.936125748261882329, -94.27892262462431461, 25.39667714426032674 ) ) ;
#9314 = VECTOR ( 'NONE', #22785, 1000.000000000000114 ) ;
#9315 = VERTEX_POINT ( 'NONE', #11352 ) ;
#9316 = DIRECTION ( 'NONE',  ( 1.000000000000000000, 0.000000000000000000, 0.000000000000000000 ) ) ;
#9317 = EDGE_LOOP ( 'NONE', ( #13127, #22671, #13592, #28098 ) ) ;
#9318 = CARTESIAN_POINT ( 'NONE',  ( -2.131628207279999844E-14, -80.00000000000000000, 1.776356839399999922E-14 ) ) ;
#9319 = FACE_OUTER_BOUND ( 'NONE', #3940, .T. ) ;
#9320 = VERTEX_POINT ( 'NONE', #323 ) ;
#9321 = CARTESIAN_POINT ( 'NONE',  ( -36.79999999999999716, -65.00000000000000000, 0.1732050807570000017 ) ) ;
#9322 = CARTESIAN_POINT ( 'NONE',  ( 3.287760219085154034, -93.08694455155865910, -28.89923981485827653 ) ) ;
#9323 = CARTESIAN_POINT ( 'NONE',  ( 8.677144207910000517, -37.95796631070000160, -21.92880662259999980 ) ) ;
#9324 = CARTESIAN_POINT ( 'NONE',  ( -19.51835485619999844, -96.93405158080001627, 8.497257209180000714 ) ) ;
#9325 = CARTESIAN_POINT ( 'NONE',  ( -41.33431406180000067, -65.21397798589998729, -2.791092524920000262 ) ) ;
#9326 = CARTESIAN_POINT ( 'NONE',  ( 21.51723897743652358, -37.39664231660807303, -7.698370384452410953 ) ) ;
#9327 = EDGE_LOOP ( 'NONE', ( #11134, #7271, #28043, #24591 ) ) ;
#9328 = DIRECTION ( 'NONE',  ( 0.000000000000000000, 1.000000000000000000, 0.000000000000000000 ) ) ;
#9329 = CARTESIAN_POINT ( 'NONE',  ( -38.24719469161180285, -65.66731758217252946, -1.502316001359380149 ) ) ;
#9330 = ADVANCED_FACE ( 'NONE', ( #24482 ), #2338, .T. ) ;
#9331 = CARTESIAN_POINT ( 'NONE',  ( 39.97648509715650533, -73.96150430830680023, 7.250349464190967375 ) ) ;
#9332 = ORIENTED_EDGE ( 'NONE', *, *, #27264, .T. ) ;
#9333 = AXIS2_PLACEMENT_3D ( 'NONE', #1362, #5582, #18986 ) ;
#9334 = CARTESIAN_POINT ( 'NONE',  ( 37.60355029590000697, -74.00000000000000000, 9.356041104380000917 ) ) ;
#9335 = CARTESIAN_POINT ( 'NONE',  ( -40.00000000000000000, -69.00000000000000000, -8.881784197000000993E-16 ) ) ;
#9336 = CARTESIAN_POINT ( 'NONE',  ( -14.34007285459999892, -80.00000123130000418, 37.07570051250000631 ) ) ;
#9337 = ORIENTED_EDGE ( 'NONE', *, *, #10958, .T. ) ;
#9339 = ADVANCED_FACE ( 'NONE', ( #9319 ), #9165, .T. ) ;
#9338 = AXIS2_PLACEMENT_3D ( 'NONE', #10741, #17338, #12935 ) ;
#9340 = DIRECTION ( 'NONE',  ( 0.000000000000000000, -1.000000000000000000, 0.000000000000000000 ) ) ;
#9341 = AXIS2_PLACEMENT_3D ( 'NONE', #19903, #17738, #13049 ) ;
#9342 = CARTESIAN_POINT ( 'NONE',  ( 0.000000000000000000, -15.49681045920000066, 0.000000000000000000 ) ) ;
#9343 = DIRECTION ( 'NONE',  ( 0.000000000000000000, -1.000000000000000000, 0.000000000000000000 ) ) ;
#9344 = CARTESIAN_POINT ( 'NONE',  ( 32.65605932329999916, -74.00000011560000246, -20.35087570529999823 ) ) ;
#9345 = EDGE_CURVE ( 'NONE', #21714, #5681, #6983, .T. ) ;
#9346 = CARTESIAN_POINT ( 'NONE',  ( 22.13628285439999743, -57.47600047049999716, -7.675802460419999917 ) ) ;
#9347 = ADVANCED_FACE ( 'NONE', ( #18073 ), #14424, .F. ) ;
#9348 = CARTESIAN_POINT ( 'NONE',  ( 27.13958535860000154, -67.66818692689999182, 1.745373480479999850 ) ) ;
#9349 = CARTESIAN_POINT ( 'NONE',  ( 29.70835240799999966, -111.0000000000000000, 6.903897247299999762 ) ) ;
#9350 = ORIENTED_EDGE ( 'NONE', *, *, #6786, .F. ) ;
#9351 = CARTESIAN_POINT ( 'NONE',  ( -38.71640881029999548, -73.50000064450000536, -7.135467304789999687 ) ) ;
#9352 = DIRECTION ( 'NONE',  ( 0.000000000000000000, -1.000000000000000000, 0.000000000000000000 ) ) ;
#9353 = CARTESIAN_POINT ( 'NONE',  ( 12.56967481719999924, -98.60488738940000530, 15.21211751169999893 ) ) ;
#9354 = ORIENTED_EDGE ( 'NONE', *, *, #2125, .F. ) ;
#9355 = AXIS2_PLACEMENT_3D ( 'NONE', #1932, #6283, #12685 ) ;
#9356 = CARTESIAN_POINT ( 'NONE',  ( 7.332335648789999993, -74.23958658489999607, 39.85912817280000553 ) ) ;
#9357 = CARTESIAN_POINT ( 'NONE',  ( 26.40928907389999836, -92.68584525839999344, 13.21124990449999892 ) ) ;
#9358 = VECTOR ( 'NONE', #16541, 1000.000000000000000 ) ;
#9359 = AXIS2_PLACEMENT_3D ( 'NONE', #22911, #20267, #2948 ) ;
#9360 = CARTESIAN_POINT ( 'NONE',  ( 22.02882315030000271, -19.46510050329999686, -0.4636558402470000173 ) ) ;
#9361 = CARTESIAN_POINT ( 'NONE',  ( -7.177518981630000461, -101.0875971110000080, 13.63542055629999972 ) ) ;
#9362 = CARTESIAN_POINT ( 'NONE',  ( 26.82419938582480512, -72.69597502604865724, -10.30336132714409558 ) ) ;
#9363 = CARTESIAN_POINT ( 'NONE',  ( -21.43329341219999762, -64.24504445130001784, 15.59675287610000005 ) ) ;
#9364 = CARTESIAN_POINT ( 'NONE',  ( 8.573564494670000258, -37.04357955609999919, -21.61801021650000010 ) ) ;
#9365 = CARTESIAN_POINT ( 'NONE',  ( 7.635702898730000854, -101.6454117330000031, 14.06304778130000166 ) ) ;
#9366 = ORIENTED_EDGE ( 'NONE', *, *, #28067, .T. ) ;
#9367 = CARTESIAN_POINT ( 'NONE',  ( 8.044160629040000288, -99.43227399260000254, 16.10826361970000065 ) ) ;
#9368 = CARTESIAN_POINT ( 'NONE',  ( 24.39713799250000292, -19.50000027030000282, 1.459766484860000046 ) ) ;
#9369 = CARTESIAN_POINT ( 'NONE',  ( -12.91037659697244599, -19.48298570124567419, 19.57229326679139447 ) ) ;
#9370 = CARTESIAN_POINT ( 'NONE',  ( -0.8840378704480000849, -98.93445099689999722, -18.66589242400000259 ) ) ;
#9371 = CARTESIAN_POINT ( 'NONE',  ( -2.563436409524490589, -19.48585536711892985, -23.48409854323134738 ) ) ;
#9372 = FACE_OUTER_BOUND ( 'NONE', #13853, .T. ) ;
#9373 = LINE ( 'NONE', #7654, #6571 ) ;
#9374 = EDGE_CURVE ( 'NONE', #27229, #1691, #7157, .T. ) ;
#9375 = DIRECTION ( 'NONE',  ( 0.000000000000000000, 1.000000000000000000, 0.000000000000000000 ) ) ;
#9376 = DIRECTION ( 'NONE',  ( 1.000000000000000000, 0.000000000000000000, 0.000000000000000000 ) ) ;
#9377 = EDGE_CURVE ( 'NONE', #3841, #11046, #16287, .T. ) ;
#9378 = CARTESIAN_POINT ( 'NONE',  ( 24.52645331487275016, -93.02765837720220077, -16.48025453447625210 ) ) ;
#9379 = CARTESIAN_POINT ( 'NONE',  ( -14.98639447530000091, -101.1747052350000047, 3.063292548799999793 ) ) ;
#9380 = AXIS2_PLACEMENT_3D ( 'NONE', #20730, #11817, #5275 ) ;
#9381 = ORIENTED_EDGE ( 'NONE', *, *, #28617, .T. ) ;
#9382 = CIRCLE ( 'NONE', #19164, 0.5000000000000004441 ) ;
#9383 = EDGE_CURVE ( 'NONE', #26844, #27945, #11197, .T. ) ;
#9384 = CARTESIAN_POINT ( 'NONE',  ( 36.47623142740000191, -74.84544903709999630, -14.77763247909999933 ) ) ;
#9385 = DIRECTION ( 'NONE',  ( 0.000000000000000000, 1.000000000000000000, 0.000000000000000000 ) ) ;
#9386 = CARTESIAN_POINT ( 'NONE',  ( 7.853421650889998773, -101.2316184180000107, 13.89973574110000065 ) ) ;
#9387 = CARTESIAN_POINT ( 'NONE',  ( 22.60879084260000127, -95.55433883439999931, -0.3969473061980000050 ) ) ;
#9388 = CARTESIAN_POINT ( 'NONE',  ( 21.29431096540000112, -35.00262504610000036, -7.521543753010000444 ) ) ;
#9389 = CARTESIAN_POINT ( 'NONE',  ( -0.8216633941299998911, -65.07442867339999282, -25.13631543320000006 ) ) ;
#9390 = CARTESIAN_POINT ( 'NONE',  ( 20.29323830529999739, -94.22763361239999824, 13.32192879709999822 ) ) ;
#9391 = CARTESIAN_POINT ( 'NONE',  ( 19.36781163719999910, -19.46510053389999939, 10.50580276810000058 ) ) ;
#9392 = DIRECTION ( 'NONE',  ( 1.000000000000000000, 0.000000000000000000, 0.000000000000000000 ) ) ;
#9393 = VERTEX_POINT ( 'NONE', #17931 ) ;
#9394 = CARTESIAN_POINT ( 'NONE',  ( 29.21673098384253109, -74.33752570142104332, -26.16904073697999067 ) ) ;
#9395 = CARTESIAN_POINT ( 'NONE',  ( -24.12300435170000057, -94.89420189139998740, -4.133213877870000275 ) ) ;
#9396 = VERTEX_POINT ( 'NONE', #26825 ) ;
#9397 = CIRCLE ( 'NONE', #28483, 5.000000000000000000 ) ;
#9398 = CARTESIAN_POINT ( 'NONE',  ( 9.117424198366714805, -92.82044061133264279, 29.10537173539315603 ) ) ;
#9399 = CARTESIAN_POINT ( 'NONE',  ( 7.383549334360000493, -18.50000000000000000, -19.69582310909999734 ) ) ;
#9400 = CARTESIAN_POINT ( 'NONE',  ( 0.000000000000000000, -10.00000000000000000, 0.000000000000000000 ) ) ;
#9401 = EDGE_CURVE ( 'NONE', #16196, #27297, #1572, .T. ) ;
#9402 = DIRECTION ( 'NONE',  ( 0.05900121837168146449, 0.000000000000000000, 0.9982579106777251798 ) ) ;
#9403 = EDGE_CURVE ( 'NONE', #7043, #10820, #3726, .T. ) ;
#9404 = CARTESIAN_POINT ( 'NONE',  ( -13.82310862920000005, -74.00000000000000000, 36.20061004779999791 ) ) ;
#9405 = FACE_OUTER_BOUND ( 'NONE', #23408, .T. ) ;
#9406 = CARTESIAN_POINT ( 'NONE',  ( -17.57653423721919950, -95.76346916417317345, 13.69972344651582397 ) ) ;
#9407 = B_SPLINE_SURFACE_WITH_KNOTS ( 'NONE', 5, 5, ( 
 ( #24686, #13894, #4568, #24830, #13750, #4718, #22650, #22353, #18275 ),
 ( #9077, #7352, #22797, #17980, #6912, #2838, #11697, #2691, #78 ),
 ( #11548, #18422, #670, #24389, #4428, #13299, #22203, #2248, #17834 ),
 ( #26732, #23508, #16215, #2989, #7916, #21046, #7652, #16801, #27460 ),
 ( #1105, #16520, #3273, #5308, #21183, #25694, #3134, #19127, #5720 ),
 ( #7509, #3545, #14603, #16370, #20761, #5585, #25281, #1366, #23091 ) ),
 .UNSPECIFIED., .F., .F., .F.,
 ( 6, 6 ),
 ( 6, 3, 6 ),
 ( 4.816191416729999730, 6.255250589880000156 ),
 ( 0.000000000000000000, 0.2500000000000000000, 0.5000000000000000000 ),
 .UNSPECIFIED. ) ;
#9408 = ORIENTED_EDGE ( 'NONE', *, *, #28165, .F. ) ;
#9409 = CARTESIAN_POINT ( 'NONE',  ( -13.16183723350000179, -70.12921532840000793, -24.09258144820000069 ) ) ;
#9410 = FACE_OUTER_BOUND ( 'NONE', #22118, .T. ) ;
#9411 = CARTESIAN_POINT ( 'NONE',  ( 8.093994091077075126, -101.4116343943851177, 14.00832529574788943 ) ) ;
#9412 = CARTESIAN_POINT ( 'NONE',  ( -13.15133833870000046, -100.9197081840000010, -8.436152112259998503 ) ) ;
#9413 = CARTESIAN_POINT ( 'NONE',  ( 15.98190517250000120, -101.1461874320000049, 2.387865266659999985 ) ) ;
#9414 = ORIENTED_EDGE ( 'NONE', *, *, #7751, .T. ) ;
#9415 = ADVANCED_FACE ( 'NONE', ( #25783 ), #5247, .T. ) ;
#9416 = CARTESIAN_POINT ( 'NONE',  ( 26.94419639614420348, -92.55017404142731152, -14.29196685862621941 ) ) ;
#9417 = ORIENTED_EDGE ( 'NONE', *, *, #23715, .T. ) ;
#9418 = VECTOR ( 'NONE', #12258, 1000.000000000000000 ) ;
#9419 = DIRECTION ( 'NONE',  ( 0.000000000000000000, 1.000000000000000000, 0.000000000000000000 ) ) ;
#9420 = B_SPLINE_CURVE_WITH_KNOTS ( 'NONE', 5,
 ( #18295, #20472, #5026, #9094, #15942, #13914 ),
 .UNSPECIFIED., .F., .F.,
 ( 6, 6 ),
 ( 0.000000000000000000, 1.000000000000000000 ),
 .UNSPECIFIED. ) ;
#9421 = CARTESIAN_POINT ( 'NONE',  ( 10.71318590899999990, -36.06167118559999807, -22.60430443919999988 ) ) ;
#9422 = CARTESIAN_POINT ( 'NONE',  ( 28.54979082390000045, -12.59999999999999964, 52.26004156059999417 ) ) ;
#9423 = CARTESIAN_POINT ( 'NONE',  ( 2.608016585090000117, -93.87272511149998877, 25.04074494509999838 ) ) ;
#9424 = VERTEX_POINT ( 'NONE', #1598 ) ;
#9425 = ORIENTED_EDGE ( 'NONE', *, *, #8516, .T. ) ;
#9426 = DIRECTION ( 'NONE',  ( 0.000000000000000000, 1.000000000000000000, 0.000000000000000000 ) ) ;
#9427 = CARTESIAN_POINT ( 'NONE',  ( 27.25648091989999955, -92.50000000000000000, -13.26500883389999963 ) ) ;
#9428 = CARTESIAN_POINT ( 'NONE',  ( 47.11398222799999758, -74.48400604130000602, -1.625803566960000168 ) ) ;
#9429 = ORIENTED_EDGE ( 'NONE', *, *, #5941, .T. ) ;
#9430 = DIRECTION ( 'NONE',  ( 1.000000000000000000, 0.000000000000000000, 1.224606353819999829E-16 ) ) ;
#9431 = CARTESIAN_POINT ( 'NONE',  ( -11.74876062667526355, -63.11832875707892754, 21.36197986565119677 ) ) ;
#9432 = CARTESIAN_POINT ( 'NONE',  ( 23.74633046638808409, -64.47177090206558603, 10.70095004269627914 ) ) ;
#9433 = VECTOR ( 'NONE', #27524, 999.9999999999998863 ) ;
#9434 = CARTESIAN_POINT ( 'NONE',  ( -3.522003140469999849, -68.93885193580000248, -27.83245572350000074 ) ) ;
#9435 = TOROIDAL_SURFACE ( 'NONE', #21543, 52.35000000000000142, 1.000000000000000000 ) ;
#9436 = CARTESIAN_POINT ( 'NONE',  ( -15.00767853189999990, -70.93206804260000808, 23.42916186189999905 ) ) ;
#9437 = ORIENTED_EDGE ( 'NONE', *, *, #9104, .T. ) ;
#9438 = FACE_OUTER_BOUND ( 'NONE', #28177, .T. ) ;
#9439 = EDGE_CURVE ( 'NONE', #3543, #23834, #20343, .T. ) ;
#9440 = CARTESIAN_POINT ( 'NONE',  ( -16.98428476389999631, -99.78393587620000460, 3.406952114930000164 ) ) ;
#9441 = CARTESIAN_POINT ( 'NONE',  ( 24.90655353600000410, -61.83365245859999959, 1.147770447419999895 ) ) ;
#9442 = CARTESIAN_POINT ( 'NONE',  ( -21.99985828019999801, -74.00000000000000000, -31.89935321680000158 ) ) ;
#9443 = EDGE_LOOP ( 'NONE', ( #17794, #5979 ) ) ;
#9444 = CARTESIAN_POINT ( 'NONE',  ( 0.000000000000000000, -92.50000000000000000, 0.000000000000000000 ) ) ;
#9445 = CARTESIAN_POINT ( 'NONE',  ( -7.367678538425209034, -73.99967062276937213, 39.29948535928571118 ) ) ;
#9446 = CARTESIAN_POINT ( 'NONE',  ( 36.63849838837199968, -74.19274952788697419, -14.34036756977614679 ) ) ;
#9447 = EDGE_LOOP ( 'NONE', ( #7155, #24333, #8609, #20413 ) ) ;
#9448 = EDGE_CURVE ( 'NONE', #6476, #14702, #13493, .T. ) ;
#9449 = CARTESIAN_POINT ( 'NONE',  ( -8.456190936129999614, -94.17494422240000063, -22.86729140410000127 ) ) ;
#9450 = CIRCLE ( 'NONE', #24815, 1.000000000000000888 ) ;
#9451 = CARTESIAN_POINT ( 'NONE',  ( -19.16019836899999618, -92.50000000000000000, 22.97842938279999814 ) ) ;
#9452 = CARTESIAN_POINT ( 'NONE',  ( 8.783852041339999417, -35.09305114600000053, -20.45839261020000066 ) ) ;
#9453 = CARTESIAN_POINT ( 'NONE',  ( 15.98584715875140816, -100.9609609849234317, 4.228316488232548132 ) ) ;
#9454 = FACE_OUTER_BOUND ( 'NONE', #14873, .T. ) ;
#9455 = ORIENTED_EDGE ( 'NONE', *, *, #12586, .T. ) ;
#9456 = CARTESIAN_POINT ( 'NONE',  ( 46.41171862319999519, -80.37540335289999405, -3.517809264200000285 ) ) ;
#9457 = DIRECTION ( 'NONE',  ( 0.9551367254897007442, 0.000000000000000000, -0.2961652167639068911 ) ) ;
#9458 = PRODUCT_DEFINITION_CONTEXT ( 'detailed design', #16864, 'design' ) ;
#9459 = APPLICATION_PROTOCOL_DEFINITION ( 'draft international standard', 'automotive_design', 1998, #11839 ) ;
#9460 = CARTESIAN_POINT ( 'NONE',  ( -12.89905543549999933, -65.07442822920000935, -21.58992615660000070 ) ) ;
#9461 = AXIS2_PLACEMENT_3D ( 'NONE', #3668, #10476, #21720 ) ;
#9462 = DIRECTION ( 'NONE',  ( 0.000000000000000000, 1.000000000000000000, 0.000000000000000000 ) ) ;
#9463 = CARTESIAN_POINT ( 'NONE',  ( 9.406883472537318269, -93.09720821804000934, 27.44372935570929428 ) ) ;
#9464 = ORIENTED_EDGE ( 'NONE', *, *, #1151, .T. ) ;
#9465 = ADVANCED_FACE ( 'NONE', ( #26052 ), #6231, .T. ) ;
#9466 = DIRECTION ( 'NONE',  ( -0.5000000000001886269, 0.000000000000000000, -0.8660254037843296837 ) ) ;
#9467 = ORIENTED_EDGE ( 'NONE', *, *, #25606, .F. ) ;
#9468 = FACE_OUTER_BOUND ( 'NONE', #3708, .T. ) ;
#9469 = DIRECTION ( 'NONE',  ( 1.000000000000000000, 0.000000000000000000, 0.000000000000000000 ) ) ;
#9470 = ORIENTED_EDGE ( 'NONE', *, *, #1602, .F. ) ;
#9471 = FACE_OUTER_BOUND ( 'NONE', #8682, .T. ) ;
#9472 = CARTESIAN_POINT ( 'NONE',  ( -31.99658184870000355, -74.50000000000000000, -31.99658184870000355 ) ) ;
#9473 = CONICAL_SURFACE ( 'NONE', #24366, 21.99999999999999645, 0.03490658503990158590 ) ;
#9474 = CARTESIAN_POINT ( 'NONE',  ( 29.41275679339999982, -39.50000000000000000, 53.83969017199999740 ) ) ;
#9475 = CARTESIAN_POINT ( 'NONE',  ( -10.52298218897619186, -19.48483231357551304, -21.08077323561843741 ) ) ;
#9476 = CARTESIAN_POINT ( 'NONE',  ( 22.95301390182565981, -94.52293547160145692, -6.773259248599760696 ) ) ;
#9477 = CARTESIAN_POINT ( 'NONE',  ( -4.500000000000000000, -13.00000000000000000, -31.00000000000000000 ) ) ;
#9478 = CARTESIAN_POINT ( 'NONE',  ( 25.62591688519999877, -71.82672919469999329, 11.84408135179999988 ) ) ;
#9479 = VERTEX_POINT ( 'NONE', #13320 ) ;
#9480 = DIRECTION ( 'NONE',  ( -0.000000000000000000, 1.000000000000000000, 0.000000000000000000 ) ) ;
#9481 = ADVANCED_FACE ( 'NONE', ( #4595, #11118 ), #26899, .F. ) ;
#9482 = CARTESIAN_POINT ( 'NONE',  ( -20.38307042409243408, -61.36262250532579543, 12.44304614358050642 ) ) ;
#9483 = CARTESIAN_POINT ( 'NONE',  ( 9.356041104380000917, -74.00000000000000000, -37.60355029590000697 ) ) ;
#9484 = ORIENTED_EDGE ( 'NONE', *, *, #6748, .T. ) ;
#9485 = AXIS2_PLACEMENT_3D ( 'NONE', #8964, #408, #4900 ) ;
#9486 = DIRECTION ( 'NONE',  ( 0.000000000000000000, -1.000000000000000000, 0.000000000000000000 ) ) ;
#9487 = CARTESIAN_POINT ( 'NONE',  ( 7.727581852389999284, -65.07443093669999712, -23.93312597839999967 ) ) ;
#9488 = CARTESIAN_POINT ( 'NONE',  ( 0.000000000000000000, -92.50000000000000000, 29.91857981989999971 ) ) ;
#9489 = ORIENTED_EDGE ( 'NONE', *, *, #2849, .T. ) ;
#9490 = CARTESIAN_POINT ( 'NONE',  ( -18.48852190589999722, -96.16769445330000110, 13.76947523039999943 ) ) ;
#9491 = ADVANCED_FACE ( 'NONE', ( #1460 ), #25600, .F. ) ;
#9492 = CARTESIAN_POINT ( 'NONE',  ( -19.33917618720000320, -45.99732788909999925, 12.50961972019999990 ) ) ;
#9493 = LINE ( 'NONE', #7481, #10477 ) ;
#9494 = CARTESIAN_POINT ( 'NONE',  ( -11.78425688200000110, -72.00000000000000000, -26.58404760160000180 ) ) ;
#9495 = CARTESIAN_POINT ( 'NONE',  ( 22.26662627150000162, -57.47855597999999588, -7.066909368720000195 ) ) ;
#9496 =( NAMED_UNIT ( * ) SI_UNIT ( $, .STERADIAN. ) SOLID_ANGLE_UNIT ( ) );
#9497 = CARTESIAN_POINT ( 'NONE',  ( -10.49977388490000152, -18.50000000000000000, 18.23111608289999808 ) ) ;
#9498 = AXIS2_PLACEMENT_3D ( 'NONE', #24917, #7145, #20387 ) ;
#9499 = ORIENTED_EDGE ( 'NONE', *, *, #11635, .F. ) ;
#9500 = FACE_BOUND ( 'NONE', #17718, .T. ) ;
#9501 = ADVANCED_FACE ( 'NONE', ( #6790 ), #20101, .T. ) ;
#9502 = CARTESIAN_POINT ( 'NONE',  ( 21.72336075670000000, -37.94103119580000083, -8.348312496720000198 ) ) ;
#9503 = DIRECTION ( 'NONE',  ( 1.000000000000000000, 0.000000000000000000, 0.000000000000000000 ) ) ;
#9504 = VERTEX_POINT ( 'NONE', #25775 ) ;
#9505 = AXIS2_PLACEMENT_3D ( 'NONE', #749, #26807, #22726 ) ;
#9506 = CARTESIAN_POINT ( 'NONE',  ( 7.253647055860000137, -74.31845592130000000, 40.32201634399999790 ) ) ;
#9507 = CARTESIAN_POINT ( 'NONE',  ( 8.001802476509999096, -18.50000000000000000, -19.02938007170000034 ) ) ;
#9508 = CARTESIAN_POINT ( 'NONE',  ( -26.69328098980000163, -74.50000000000000000, -35.88566914520000495 ) ) ;
#9509 = AXIS2_PLACEMENT_3D ( 'NONE', #20354, #10991, #27215 ) ;
#9510 =( NAMED_UNIT ( * ) SI_UNIT ( $, .STERADIAN. ) SOLID_ANGLE_UNIT ( ) );
#9511 = CARTESIAN_POINT ( 'NONE',  ( -12.16062739216652844, -93.49518251413884684, -23.50287856905526596 ) ) ;
#9512 = CARTESIAN_POINT ( 'NONE',  ( 9.476129726630000860, -36.00000000000000000, -20.06309461859999743 ) ) ;
#9513 = ADVANCED_FACE ( 'NONE', ( #14815 ), #17304, .T. ) ;
#9514 = CARTESIAN_POINT ( 'NONE',  ( 21.26981850238844984, -34.71690492586082399, -7.540080587919900879 ) ) ;
#9515 = ORIENTED_EDGE ( 'NONE', *, *, #19917, .T. ) ;
#9516 = CARTESIAN_POINT ( 'NONE',  ( -11.90443957499999961, -64.24504445130001784, -23.68393584109999850 ) ) ;
#9517 = CARTESIAN_POINT ( 'NONE',  ( -36.76944941322930305, -63.07121106306917824, 0.1555666912533766322 ) ) ;
#9518 = CARTESIAN_POINT ( 'NONE',  ( -0.6277499419469999564, -98.58303758080000989, -18.67917185369999800 ) ) ;
#9519 = ORIENTED_EDGE ( 'NONE', *, *, #20842, .T. ) ;
#9520 = AXIS2_PLACEMENT_3D ( 'NONE', #23982, #26463, #28207 ) ;
#9521 = CARTESIAN_POINT ( 'NONE',  ( -2.028994704583232167, -19.47131810280622233, -22.58029175209635397 ) ) ;
#9522 = CARTESIAN_POINT ( 'NONE',  ( -13.85848666890000125, -57.40875702409999803, 21.24403892489999990 ) ) ;
#9523 = FACE_OUTER_BOUND ( 'NONE', #1412, .T. ) ;
#9524 = CARTESIAN_POINT ( 'NONE',  ( 15.55721680684482422, -95.01009333053707451, 17.28868226685500531 ) ) ;
#9525 = CARTESIAN_POINT ( 'NONE',  ( -39.33235237970008313, -73.62392792451801427, 7.219194746715398736 ) ) ;
#9526 = CARTESIAN_POINT ( 'NONE',  ( -2.578307999469999778, -52.56313962710000709, -25.11373953509999879 ) ) ;
#9527 = CARTESIAN_POINT ( 'NONE',  ( 23.17371582640000227, -44.86350384069999819, -9.449797638930000687 ) ) ;
#9528 = DIRECTION ( 'NONE',  ( 0.4151946956541399669, 0.5000000000001689759, 0.7600087925152558821 ) ) ;
#9529 = DIRECTION ( 'NONE',  ( 0.000000000000000000, -1.000000000000000000, 0.000000000000000000 ) ) ;
#9530 = EDGE_LOOP ( 'NONE', ( #718, #21383, #10627, #8361, #23139, #28343 ) ) ;
#9531 = CARTESIAN_POINT ( 'NONE',  ( 6.938098718590000047, -101.3138676899999950, 14.32202409469999971 ) ) ;
#9532 = CARTESIAN_POINT ( 'NONE',  ( 13.87366454287167272, -97.42330309954748202, -15.20396809591327880 ) ) ;
#9533 = AXIS2_PLACEMENT_3D ( 'NONE', #7767, #4986, #4852 ) ;
#9534 = CARTESIAN_POINT ( 'NONE',  ( 8.137534397419999621, -101.2306315539999986, 14.02341335179999859 ) ) ;
#9535 = CARTESIAN_POINT ( 'NONE',  ( 23.56065677060000496, -94.89196973819998959, -2.367188657780000316 ) ) ;
#9536 = CARTESIAN_POINT ( 'NONE',  ( 20.36793975040000149, -34.63244848020000433, -8.805019347009999109 ) ) ;
#9537 = CARTESIAN_POINT ( 'NONE',  ( 23.26234223547589153, -59.45680040906446351, 10.43566352099444750 ) ) ;
#9538 = VECTOR ( 'NONE', #9340, 1000.000000000000000 ) ;
#9539 = CARTESIAN_POINT ( 'NONE',  ( 28.24241828440000290, -92.51331410669999400, 7.994460720630000239 ) ) ;
#9540 = ADVANCED_FACE ( 'NONE', ( #21126 ), #7485, .F. ) ;
#9541 = CARTESIAN_POINT ( 'NONE',  ( 21.80457179460000106, -37.33399608290000060, -8.522642616350001532 ) ) ;
#9542 = CARTESIAN_POINT ( 'NONE',  ( -20.49585304202401304, -93.08996811592636789, -20.60571651767068602 ) ) ;
#9543 = EDGE_CURVE ( 'NONE', #9289, #17308, #25569, .T. ) ;
#9544 = B_SPLINE_CURVE_WITH_KNOTS ( 'NONE', 5,
 ( #20580, #644, #20131, #24658, #15605, #200, #14015, #26995, #15901 ),
 .UNSPECIFIED., .F., .F.,
 ( 6, 3, 6 ),
 ( -6.717368912360000444, -6.039642335889999991, -4.007746616509999527 ),
 .UNSPECIFIED. ) ;
#9545 = CARTESIAN_POINT ( 'NONE',  ( 16.36531008860000114, -100.1459902240000019, 4.432835649019999380 ) ) ;
#9546 = ORIENTED_EDGE ( 'NONE', *, *, #14658, .T. ) ;
#9547 = CARTESIAN_POINT ( 'NONE',  ( -3.058911230670000148, -72.82938648530000592, -28.52031834779999997 ) ) ;
#9548 = CARTESIAN_POINT ( 'NONE',  ( -15.65528393829999843, -99.91547912590000635, -8.850932903340000379 ) ) ;
#9549 = VERTEX_POINT ( 'NONE', #8486 ) ;
#9550 = EDGE_CURVE ( 'NONE', #2397, #20007, #4266, .T. ) ;
#9551 = CARTESIAN_POINT ( 'NONE',  ( -30.47727153658393817, -92.54893169919638751, 1.177273713142487299 ) ) ;
#9552 = EDGE_CURVE ( 'NONE', #27727, #898, #21619, .T. ) ;
#9553 = ORIENTED_EDGE ( 'NONE', *, *, #4752, .F. ) ;
#9554 = FACE_OUTER_BOUND ( 'NONE', #1336, .T. ) ;
#9555 = PLANE ( 'NONE',  #27506 ) ;
#9556 = AXIS2_PLACEMENT_3D ( 'NONE', #13705, #19811, #19958 ) ;
#9557 = CARTESIAN_POINT ( 'NONE',  ( -37.60355029590000697, -84.00000000000000000, -9.356041104380000917 ) ) ;
#9558 = CARTESIAN_POINT ( 'NONE',  ( -7.244146985819436502, -74.18164516872573699, -40.29126735531537662 ) ) ;
#9559 = CARTESIAN_POINT ( 'NONE',  ( -14.42755416139999980, -74.19081742459999873, 36.52101890659999839 ) ) ;
#9560 = CARTESIAN_POINT ( 'NONE',  ( -21.22624868000000120, -65.72101818089998915, 15.03418113859999927 ) ) ;
#9561 = CARTESIAN_POINT ( 'NONE',  ( -36.25000000000000000, -84.50000000000000000, 2.124561919619999789E-15 ) ) ;
#9562 = ORIENTED_EDGE ( 'NONE', *, *, #16252, .T. ) ;
#9563 = CARTESIAN_POINT ( 'NONE',  ( -11.86976558200000120, -71.47032289400000593, -26.35122234239999983 ) ) ;
#9564 = CARTESIAN_POINT ( 'NONE',  ( 8.153551712620000558, -19.43778590579999843, -20.47343976009999977 ) ) ;
#9565 = CARTESIAN_POINT ( 'NONE',  ( -6.717799458580000049, -84.50000000000000000, -40.65853658540000026 ) ) ;
#9566 = FACE_OUTER_BOUND ( 'NONE', #13048, .T. ) ;
#9567 = CARTESIAN_POINT ( 'NONE',  ( 15.38949396259999958, -100.9938510739999913, 2.079911269780000183 ) ) ;
#9568 = ORIENTED_EDGE ( 'NONE', *, *, #2346, .T. ) ;
#9569 = ORIENTED_EDGE ( 'NONE', *, *, #22344, .T. ) ;
#9570 = AXIS2_PLACEMENT_3D ( 'NONE', #6720, #20260, #22607 ) ;
#9571 = CARTESIAN_POINT ( 'NONE',  ( -14.09870646349260603, -80.05388654820464467, 36.88642194476569358 ) ) ;
#9572 = CARTESIAN_POINT ( 'NONE',  ( -3.818589290579999851, -98.24904979169998853, 18.91383438800000150 ) ) ;
#9573 = CARTESIAN_POINT ( 'NONE',  ( 1.375221473979999942, -94.98812079580000045, 24.46248441310000032 ) ) ;
#9574 = ORIENTED_EDGE ( 'NONE', *, *, #22180, .T. ) ;
#9575 = EDGE_CURVE ( 'NONE', #9035, #25958, #19314, .T. ) ;
#9576 = CARTESIAN_POINT ( 'NONE',  ( -27.66915836665225115, -93.38554229045760735, 0.4566536595772645590 ) ) ;
#9577 = DIRECTION ( 'NONE',  ( 0.9295286103719527793, 0.000000000000000000, 0.3687499999999814260 ) ) ;
#9578 = CARTESIAN_POINT ( 'NONE',  ( 47.08605683180000057, -74.34014987910001082, -1.561105320619999848 ) ) ;
#9579 = ORIENTED_EDGE ( 'NONE', *, *, #10688, .T. ) ;
#9580 = AXIS2_PLACEMENT_3D ( 'NONE', #4540, #15747, #2368 ) ;
#9581 = CARTESIAN_POINT ( 'NONE',  ( 7.247933038816999129, -73.86845561477531419, -39.82679900489436164 ) ) ;
#9582 = CARTESIAN_POINT ( 'NONE',  ( -11.45610569668674295, -61.34399254273181867, 20.94869055166078908 ) ) ;
#9583 = EDGE_CURVE ( 'NONE', #9687, #3916, #26516, .T. ) ;
#9584 = CARTESIAN_POINT ( 'NONE',  ( 0.000000000000000000, -1.000000000000000000, 0.000000000000000000 ) ) ;
#9585 = CARTESIAN_POINT ( 'NONE',  ( -2.842096223940000055, -64.76590626960000918, -26.52558581780000324 ) ) ;
#9586 = CARTESIAN_POINT ( 'NONE',  ( -16.42252987980000256, -71.30682482819999279, 23.34985130180000112 ) ) ;
#9587 = ORIENTED_EDGE ( 'NONE', *, *, #9448, .F. ) ;
#9588 = CARTESIAN_POINT ( 'NONE',  ( 36.46839126729999947, -74.19089203260000431, -14.49828573059999925 ) ) ;
#9589 = CARTESIAN_POINT ( 'NONE',  ( -15.69013080879999933, -101.5700432450000079, 3.430602099230000146 ) ) ;
#9590 = CARTESIAN_POINT ( 'NONE',  ( 24.49108460629999939, -63.62177041899999352, -0.2391711755510000093 ) ) ;
#9591 = CARTESIAN_POINT ( 'NONE',  ( -20.62138254979999985, -63.58944626250000454, 13.29929482439999866 ) ) ;
#9592 = ORIENTED_EDGE ( 'NONE', *, *, #4446, .T. ) ;
#9593 = CARTESIAN_POINT ( 'NONE',  ( 28.91458899939999938, -72.00000000000000000, 3.086557976320000396 ) ) ;
#9594 = CARTESIAN_POINT ( 'NONE',  ( 1.100347978140000071, -100.4792519539999915, -16.15648718290000119 ) ) ;
#9595 = CARTESIAN_POINT ( 'NONE',  ( 36.31482215109925704, -74.00000000000000000, -13.86667273340584039 ) ) ;
#9596 = VERTEX_POINT ( 'NONE', #21901 ) ;
#9597 = CARTESIAN_POINT ( 'NONE',  ( -11.95735878380000017, -93.37862425630000018, -23.50938391520000081 ) ) ;
#9598 = CARTESIAN_POINT ( 'NONE',  ( 22.65540084869999760, -61.59774147150000090, 10.37602781989999912 ) ) ;
#9599 = DIRECTION ( 'NONE',  ( 1.000000000000000000, 0.000000000000000000, 0.000000000000000000 ) ) ;
#9600 = CARTESIAN_POINT ( 'NONE',  ( 16.01243526655122196, -100.9229461893936701, 4.244774380830527605 ) ) ;
#9601 = CARTESIAN_POINT ( 'NONE',  ( 19.60651740941162657, -94.52293547161876575, 13.72233081940722599 ) ) ;
#9602 = ORIENTED_EDGE ( 'NONE', *, *, #7098, .T. ) ;
#9603 = CARTESIAN_POINT ( 'NONE',  ( 46.85006010219999695, -80.10037130149999030, -2.646644417630000135 ) ) ;
#9604 = CONTEXT_DEPENDENT_SHAPE_REPRESENTATION ( #19821, #22013 ) ;
#9605 = CARTESIAN_POINT ( 'NONE',  ( -13.35146630740000084, -18.50000000000000000, 18.52320307730000337 ) ) ;
#9606 = CARTESIAN_POINT ( 'NONE',  ( -11.31871641740000101, -57.41946977210000114, -22.35641880389999869 ) ) ;
#9607 = CARTESIAN_POINT ( 'NONE',  ( -7.135467304789999687, -73.50000064450000536, 38.71640881029999548 ) ) ;
#9608 = CARTESIAN_POINT ( 'NONE',  ( -4.794255386040000566, -17.50000000000000000, -8.775825618900000791 ) ) ;
#9609 = EDGE_LOOP ( 'NONE', ( #10098, #12531, #4780, #28448 ) ) ;
#9610 = EDGE_CURVE ( 'NONE', #12917, #23425, #10508, .T. ) ;
#9611 = CARTESIAN_POINT ( 'NONE',  ( -41.75000000000000000, -65.56519245710001087, -1.769653913539999790 ) ) ;
#9612 = ORIENTED_EDGE ( 'NONE', *, *, #6763, .T. ) ;
#9613 = CARTESIAN_POINT ( 'NONE',  ( 22.45957212879999787, -52.58489974430000302, 10.08523539449999973 ) ) ;
#9614 = CARTESIAN_POINT ( 'NONE',  ( -6.005235968310000061, -101.3350617309999961, 14.85412936009999996 ) ) ;
#9615 = ORIENTED_EDGE ( 'NONE', *, *, #7596, .F. ) ;
#9616 = CARTESIAN_POINT ( 'NONE',  ( 46.25000000000000000, -80.00000000000000000, -4.582575694960000057 ) ) ;
#9617 = ADVANCED_FACE ( 'NONE', ( #19424 ), #18169, .T. ) ;
#9618 = CARTESIAN_POINT ( 'NONE',  ( 40.35968420270000223, -74.26794181920000426, 7.250122995559999950 ) ) ;
#9619 = CARTESIAN_POINT ( 'NONE',  ( 0.000000000000000000, -10.00000000000000000, 0.000000000000000000 ) ) ;
#9620 = CARTESIAN_POINT ( 'NONE',  ( 25.52419697193059278, -69.00255572341212940, -8.618219423246786803 ) ) ;
#9621 = DIRECTION ( 'NONE',  ( 0.000000000000000000, 1.000000000000000000, 0.000000000000000000 ) ) ;
#9622 = ORIENTED_EDGE ( 'NONE', *, *, #3758, .F. ) ;
#9623 = CARTESIAN_POINT ( 'NONE',  ( -32.69645379630000548, -79.77277768780000144, -21.71458329359999695 ) ) ;
#9624 = CARTESIAN_POINT ( 'NONE',  ( -19.95527577780000072, -57.47855601759999900, 12.14622656770000120 ) ) ;
#9625 = CYLINDRICAL_SURFACE ( 'NONE', #27523, 34.89999999999999858 ) ;
#9626 = ORIENTED_EDGE ( 'NONE', *, *, #18472, .F. ) ;
#9627 = CARTESIAN_POINT ( 'NONE',  ( 40.00000000000000000, -69.50000000000000000, 2.433892081919999696E-15 ) ) ;
#9628 = CARTESIAN_POINT ( 'NONE',  ( 9.356041104380000917, -84.50000000000000000, -37.60355029590000697 ) ) ;
#9629 = EDGE_LOOP ( 'NONE', ( #10118, #1201, #10272, #10829 ) ) ;
#9630 = CARTESIAN_POINT ( 'NONE',  ( -17.79736829950000043, -96.96042919349999067, 11.10778547589999832 ) ) ;
#9631 = CARTESIAN_POINT ( 'NONE',  ( -19.03577102200000226, -32.73235193859999725, 11.99443138589999869 ) ) ;
#9632 = CARTESIAN_POINT ( 'NONE',  ( 0.000000000000000000, -29.89689110870000022, 0.000000000000000000 ) ) ;
#9633 = DIRECTION ( 'NONE',  ( 0.000000000000000000, 1.000000000000000000, 0.000000000000000000 ) ) ;
#9634 = DIRECTION ( 'NONE',  ( 0.4794255386042040046, 0.000000000000000000, 0.8775825618903722036 ) ) ;
#9635 = CARTESIAN_POINT ( 'NONE',  ( 25.71060173579999741, -66.29767256830000122, 0.2782536591429999318 ) ) ;
#9636 = ORIENTED_EDGE ( 'NONE', *, *, #21671, .F. ) ;
#9637 = EDGE_CURVE ( 'NONE', #22, #9643, #11162, .T. ) ;
#9638 = CARTESIAN_POINT ( 'NONE',  ( 9.014522480169999241, -36.52810941340000284, -21.48399575520000226 ) ) ;
#9639 = CARTESIAN_POINT ( 'NONE',  ( -39.13694367224998416, -73.55869875170414218, -7.198781032002129265 ) ) ;
#9640 = CIRCLE ( 'NONE', #17087, 0.7999999999999986011 ) ;
#9641 = CARTESIAN_POINT ( 'NONE',  ( 21.75704398650000115, -37.63585108239999499, -8.427448657780001184 ) ) ;
#9642 = CARTESIAN_POINT ( 'NONE',  ( 17.29688842079999844, -95.76597000319999609, 14.77140804379999928 ) ) ;
#9643 = VERTEX_POINT ( 'NONE', #4416 ) ;
#9644 = CARTESIAN_POINT ( 'NONE',  ( 21.91842625758061303, -37.33819205718435796, -8.685017703894253316 ) ) ;
#9645 = CARTESIAN_POINT ( 'NONE',  ( 46.77849477899999897, -74.12949171449999142, -3.288587074160000068 ) ) ;
#9646 = EDGE_CURVE ( 'NONE', #22453, #2955, #19969, .T. ) ;
#9647 = B_SPLINE_SURFACE_WITH_KNOTS ( 'NONE', 5, 5, ( 
 ( #17190, #4812, #11346, #16016, #2638, #24922, #5392, #13691, #9460 ),
 ( #16159, #9157, #7148, #5099, #18215, #13980, #22889, #7448, #7291 ),
 ( #25219, #14273, #18365, #20393, #11485, #615, #4952, #26966, #25067 ),
 ( #27252, #11789, #466, #9310, #27110, #11634, #13835, #22738, #5248 ),
 ( #11933, #18506, #2777, #23031, #20548, #2927, #20701, #904, #760 ),
 ( #9746, #9606, #14133, #3081, #17630, #26818, #4658, #12937, #22445 ) ),
 .UNSPECIFIED., .F., .F., .F.,
 ( 6, 6 ),
 ( 6, 3, 6 ),
 ( 8.242378609270000211, 18.74558921099999864 ),
 ( 0.000000000000000000, 1.000000000000000000, 2.000000000000000000 ),
 .UNSPECIFIED. ) ;
#9648 = CARTESIAN_POINT ( 'NONE',  ( 7.010390260919999428E-15, -84.50000000000000000, 36.25000000000000000 ) ) ;
#9649 = CARTESIAN_POINT ( 'NONE',  ( -7.936795339069999677, -100.2522625769999962, 15.05294100799999946 ) ) ;
#9650 = CARTESIAN_POINT ( 'NONE',  ( -7.325370793560000315, -19.50000000000000000, -24.94672208400000102 ) ) ;
#9651 = CARTESIAN_POINT ( 'NONE',  ( -10.29133506492763495, -93.94301621637545452, -23.20339123508392376 ) ) ;
#9652 = DIRECTION ( 'NONE',  ( 0.9704142011833034598, 0.000000000000000000, -0.2414462220490750377 ) ) ;
#9653 = CARTESIAN_POINT ( 'NONE',  ( 7.302962794079999931, -101.1832940899999898, 13.42647164559999950 ) ) ;
#9654 = ORIENTED_EDGE ( 'NONE', *, *, #15229, .F. ) ;
#9655 = VECTOR ( 'NONE', #24309, 1000.000000000000000 ) ;
#9656 = CARTESIAN_POINT ( 'NONE',  ( -39.35783505871010846, -73.63371395844393419, 7.221517031003334530 ) ) ;
#9657 = CARTESIAN_POINT ( 'NONE',  ( -29.47186164440000056, -93.00000450890000536, -0.4149713922389999810 ) ) ;
#9658 = CARTESIAN_POINT ( 'NONE',  ( 11.83897591930000104, -98.30614355250000358, -15.44231161390000118 ) ) ;
#9659 = ORIENTED_EDGE ( 'NONE', *, *, #20031, .T. ) ;
#9660 = CARTESIAN_POINT ( 'NONE',  ( -2.139909113419224074, -19.47322495657797248, -22.70449621793245498 ) ) ;
#9661 = CARTESIAN_POINT ( 'NONE',  ( 1.421085471519999883E-15, -89.50000000000000000, 3.042011087470000117E-15 ) ) ;
#9662 = CARTESIAN_POINT ( 'NONE',  ( -2.572067239809999961, -45.94038128989999592, -24.63225655530000324 ) ) ;
#9663 = CARTESIAN_POINT ( 'NONE',  ( -17.59792109239500846, -92.65976904079671783, 24.91111247217822466 ) ) ;
#9664 = CARTESIAN_POINT ( 'NONE',  ( -38.29236626841033342, -63.05619511568021096, -2.812618181335909462 ) ) ;
#9665 = VECTOR ( 'NONE', #27468, 1000.000000000000000 ) ;
#9666 = CARTESIAN_POINT ( 'NONE',  ( 21.61801161032304819, -37.04357994246159080, -8.573564458946657751 ) ) ;
#9667 = DIRECTION ( 'NONE',  ( 0.000000000000000000, -1.000000000000000000, 0.000000000000000000 ) ) ;
#9668 = LINE ( 'NONE', #27472, #1118 ) ;
#9669 = VERTEX_POINT ( 'NONE', #8208 ) ;
#9670 = CARTESIAN_POINT ( 'NONE',  ( 0.000000000000000000, -86.00000000000000000, 0.000000000000000000 ) ) ;
#9671 = CARTESIAN_POINT ( 'NONE',  ( 13.87165893064168820, -97.41291607268185260, -15.22385153909266187 ) ) ;
#9672 = AXIS2_PLACEMENT_3D ( 'NONE', #13837, #2780, #3083 ) ;
#9673 = CARTESIAN_POINT ( 'NONE',  ( -12.68142862450000052, -66.36586770009999725, 22.39764779240000081 ) ) ;
#9674 = CARTESIAN_POINT ( 'NONE',  ( 19.46718696450000152, -35.19368270689999889, -8.987515577199999939 ) ) ;
#9675 = CARTESIAN_POINT ( 'NONE',  ( 23.15717220300345147, -57.99960184875410363, 10.38505609836370702 ) ) ;
#9676 = CARTESIAN_POINT ( 'NONE',  ( 21.75609418980000243, -93.65024019829999702, 12.77708436150000004 ) ) ;
#9677 = FACE_OUTER_BOUND ( 'NONE', #26334, .T. ) ;
#9678 = CARTESIAN_POINT ( 'NONE',  ( 0.3164238574520000236, -92.54628605920001405, -30.13191910649999983 ) ) ;
#9679 = DIRECTION ( 'NONE',  ( -0.9863585068926601362, 0.000000000000000000, -0.1646113479699435334 ) ) ;
#9680 = CARTESIAN_POINT ( 'NONE',  ( -8.569349526716633747, -80.50000000000000000, 38.48258446242443398 ) ) ;
#9681 = ORIENTED_EDGE ( 'NONE', *, *, #19249, .F. ) ;
#9682 = CARTESIAN_POINT ( 'NONE',  ( -26.60903970598167589, -23.00000000000000000, -48.70752046822583736 ) ) ;
#9683 = TOROIDAL_SURFACE ( 'NONE', #7828, 55.85192378860000417, 0.3499999999999999778 ) ;
#9684 = CARTESIAN_POINT ( 'NONE',  ( -13.15133943750000078, -100.9197081840000010, -8.436149941960000120 ) ) ;
#9685 = EDGE_LOOP ( 'NONE', ( #1703, #27680, #20023, #14541, #9752 ) ) ;
#9686 = CARTESIAN_POINT ( 'NONE',  ( -30.41749109087852077, -92.77481473396083800, 2.243079458206835408 ) ) ;
#9687 = VERTEX_POINT ( 'NONE', #10936 ) ;
#9688 = CARTESIAN_POINT ( 'NONE',  ( 0.09569509352523042356, -101.5829753080977582, -16.05020235182843891 ) ) ;
#9689 = CARTESIAN_POINT ( 'NONE',  ( -11.08158641716409498, -19.46474590321556875, 19.12288009785157428 ) ) ;
#9690 = CARTESIAN_POINT ( 'NONE',  ( -7.241237543289999579, -73.80576217300000508, 39.53368540329999803 ) ) ;
#9691 = CARTESIAN_POINT ( 'NONE',  ( -11.72126804459999860, -100.9137139110000021, -10.34406313869999927 ) ) ;
#9692 = CARTESIAN_POINT ( 'NONE',  ( -7.244026535083167850, -74.18384006180646395, -40.29424782656837323 ) ) ;
#9693 = AXIS2_PLACEMENT_3D ( 'NONE', #25049, #27682, #24907 ) ;
#9694 = CARTESIAN_POINT ( 'NONE',  ( 13.53498567739999991, -95.75647260690000451, -17.96385118539999937 ) ) ;
#9695 = EDGE_LOOP ( 'NONE', ( #21551, #653, #9553, #12452 ) ) ;
#9696 = CIRCLE ( 'NONE', #1339, 9.500000000000001776 ) ;
#9697 = DIRECTION ( 'NONE',  ( 0.000000000000000000, -1.000000000000000000, 0.000000000000000000 ) ) ;
#9698 = CARTESIAN_POINT ( 'NONE',  ( 8.810945591680001243, -22.49864585750000145, -19.93464393029999826 ) ) ;
#9699 = CARTESIAN_POINT ( 'NONE',  ( -1.450349733947329467, -57.47122607689037466, -23.51019145097244234 ) ) ;
#9700 = CARTESIAN_POINT ( 'NONE',  ( 20.04647669423046352, -19.46665351427041202, 9.775544613538123428 ) ) ;
#9701 = CARTESIAN_POINT ( 'NONE',  ( 15.75037718549999965, -101.2459394079999981, 2.542735002740000194 ) ) ;
#9702 = ORIENTED_EDGE ( 'NONE', *, *, #18840, .F. ) ;
#9703 = EDGE_CURVE ( 'NONE', #4968, #20017, #12562, .T. ) ;
#9704 = ORIENTED_EDGE ( 'NONE', *, *, #12711, .F. ) ;
#9705 = EDGE_CURVE ( 'NONE', #18448, #23053, #21881, .T. ) ;
#9706 = ADVANCED_FACE ( 'NONE', ( #12841 ), #5154, .T. ) ;
#9707 = CARTESIAN_POINT ( 'NONE',  ( -2.565528333990000132, -57.82174915179999886, -24.93709123049999832 ) ) ;
#9708 = CARTESIAN_POINT ( 'NONE',  ( -2.609756160320000351, -97.14975611439999170, 21.14422222710000199 ) ) ;
#9709 = CARTESIAN_POINT ( 'NONE',  ( 12.02192718879999944, -92.50000321470000131, 27.08489650960000006 ) ) ;
#9710 = ORIENTED_EDGE ( 'NONE', *, *, #9987, .T. ) ;
#9711 = VECTOR ( 'NONE', #8816, 1000.000000000000000 ) ;
#9712 = CIRCLE ( 'NONE', #18580, 7.249999999999999112 ) ;
#9713 = ORIENTED_EDGE ( 'NONE', *, *, #8007, .F. ) ;
#9714 = FACE_OUTER_BOUND ( 'NONE', #1159, .T. ) ;
#9715 = CARTESIAN_POINT ( 'NONE',  ( 9.445827302050000540, -44.46958577849999728, -23.16276489379999859 ) ) ;
#9716 = PLANE ( 'NONE',  #25104 ) ;
#9717 = ORIENTED_EDGE ( 'NONE', *, *, #27972, .T. ) ;
#9718 = CARTESIAN_POINT ( 'NONE',  ( 7.215414233289999757, -74.50000000000000000, -40.70731707320000226 ) ) ;
#9719 = LINE ( 'NONE', #3187, #6658 ) ;
#9720 = CARTESIAN_POINT ( 'NONE',  ( -14.65665268890000128, -79.65629807879999191, 36.94583904750000158 ) ) ;
#9721 = DIRECTION ( 'NONE',  ( -0.2588190451029840911, 0.000000000000000000, -0.9659258262889440783 ) ) ;
#9722 = CARTESIAN_POINT ( 'NONE',  ( -1.973996428270000214, -65.91612967349999508, -25.65258536809999868 ) ) ;
#9723 = CARTESIAN_POINT ( 'NONE',  ( -16.72250540970000188, -71.11599492770000097, 23.42677820880000183 ) ) ;
#9724 = ORIENTED_EDGE ( 'NONE', *, *, #12380, .T. ) ;
#9725 = CYLINDRICAL_SURFACE ( 'NONE', #27904, 7.250000000000004441 ) ;
#9726 = CARTESIAN_POINT ( 'NONE',  ( -15.27515611620000158, -100.9817027879999927, 2.888957402029999511 ) ) ;
#9727 = DIRECTION ( 'NONE',  ( 0.4794255386042036715, 0.000000000000000000, 0.8775825618903724257 ) ) ;
#9728 = CARTESIAN_POINT ( 'NONE',  ( -21.14045977570000190, -64.47177096180000433, 15.21445029600000076 ) ) ;
#9729 = ORIENTED_EDGE ( 'NONE', *, *, #10056, .T. ) ;
#9730 = AXIS2_PLACEMENT_3D ( 'NONE', #20304, #24831, #6771 ) ;
#9731 = CARTESIAN_POINT ( 'NONE',  ( -40.00000000000000000, -63.00000000000000000, 0.000000000000000000 ) ) ;
#9732 = CARTESIAN_POINT ( 'NONE',  ( -1.179391805059999854, -18.50000000000000000, -21.01038717779999843 ) ) ;
#9733 = CARTESIAN_POINT ( 'NONE',  ( 36.73205512257106875, -74.36687860487361945, -14.52407699815695352 ) ) ;
#9734 = ORIENTED_EDGE ( 'NONE', *, *, #6133, .F. ) ;
#9736 = EDGE_CURVE ( 'NONE', #13319, #5829, #10676, .T. ) ;
#9735 = AXIS2_PLACEMENT_3D ( 'NONE', #24541, #2560, #22363 ) ;
#9737 = AXIS2_PLACEMENT_3D ( 'NONE', #13162, #26302, #2253 ) ;
#9738 = DIRECTION ( 'NONE',  ( 0.000000000000000000, 1.000000000000000000, 0.000000000000000000 ) ) ;
#9739 = DIRECTION ( 'NONE',  ( 0.000000000000000000, -1.000000000000000000, 0.000000000000000000 ) ) ;
#9740 = CARTESIAN_POINT ( 'NONE',  ( -39.34243475499999221, -65.56519245710001087, -2.400371413390000264 ) ) ;
#9741 = DIRECTION ( 'NONE',  ( 0.000000000000000000, -1.000000000000000000, 0.000000000000000000 ) ) ;
#9742 = CARTESIAN_POINT ( 'NONE',  ( 13.91346788694689529, -99.62767017963102489, -10.34347588715546351 ) ) ;
#9743 = ORIENTED_EDGE ( 'NONE', *, *, #14240, .F. ) ;
#9744 = EDGE_CURVE ( 'NONE', #22934, #14668, #25911, .T. ) ;
#9745 = CARTESIAN_POINT ( 'NONE',  ( -11.32770615259999936, -18.50000000000000000, 18.02817438119999949 ) ) ;
#9746 = CARTESIAN_POINT ( 'NONE',  ( -11.46863496399999960, -57.40875702469999453, -22.62382260229999886 ) ) ;
#9747 = CARTESIAN_POINT ( 'NONE',  ( 37.22630421854149319, -79.99409917514977053, -13.87589282898977849 ) ) ;
#9748 = CARTESIAN_POINT ( 'NONE',  ( 24.38889592600000000, -66.59094944230000124, -8.558251894909998825 ) ) ;
#9749 = CARTESIAN_POINT ( 'NONE',  ( 8.318977493526379163, -93.18009965537066819, 27.27745815282288433 ) ) ;
#9750 = EDGE_LOOP ( 'NONE', ( #28518, #14300, #25943, #620 ) ) ;
#9751 = CARTESIAN_POINT ( 'NONE',  ( 22.78266135780000212, -94.59276583640000524, -6.873198607739999133 ) ) ;
#9752 = ORIENTED_EDGE ( 'NONE', *, *, #23047, .T. ) ;
#9753 = CYLINDRICAL_SURFACE ( 'NONE', #19561, 4.750000000000000888 ) ;
#9754 = CARTESIAN_POINT ( 'NONE',  ( -6.166870861799999659, -101.6484611580000035, 14.76436469649999950 ) ) ;
#9755 = ORIENTED_EDGE ( 'NONE', *, *, #11371, .T. ) ;
#9756 = DIRECTION ( 'NONE',  ( 0.4794255386042041156, 0.000000000000000000, 0.8775825618903722036 ) ) ;
#9757 = AXIS2_PLACEMENT_3D ( 'NONE', #21503, #1561, #5770 ) ;
#9758 = CIRCLE ( 'NONE', #17194, 20.64285714289999873 ) ;
#9759 = CARTESIAN_POINT ( 'NONE',  ( 38.71640869449999656, -73.50000064450000536, 7.135466578850000019 ) ) ;
#9760 = CARTESIAN_POINT ( 'NONE',  ( -10.52559454271665729, -19.48499002900891952, -21.09029437625177650 ) ) ;
#9761 = CARTESIAN_POINT ( 'NONE',  ( 41.00000000000000000, -80.50000000000000000, -10.20110288159999890 ) ) ;
#9762 = CARTESIAN_POINT ( 'NONE',  ( -11.85777263121401859, -63.71742432004833034, -23.51471264972168385 ) ) ;
#9763 = CARTESIAN_POINT ( 'NONE',  ( 47.01511379249026135, -79.64389730943054246, -2.310193425807324896 ) ) ;
#9764 = ORIENTED_EDGE ( 'NONE', *, *, #10665, .F. ) ;
#9765 = DIRECTION ( 'NONE',  ( 1.000000000000000000, 0.000000000000000000, 0.000000000000000000 ) ) ;
#9766 = CARTESIAN_POINT ( 'NONE',  ( 19.86697918760000192, -97.58045781670000451, 2.400950920309999681 ) ) ;
#9767 = CYLINDRICAL_SURFACE ( 'NONE', #23304, 9.500000000000001776 ) ;
#9768 = VERTEX_POINT ( 'NONE', #27155 ) ;
#9769 = EDGE_CURVE ( 'NONE', #1054, #17152, #10261, .T. ) ;
#9770 = CARTESIAN_POINT ( 'NONE',  ( 29.70835240799999966, -93.00000000000000000, 6.903897247299999762 ) ) ;
#9771 = DIRECTION ( 'NONE',  ( 1.000000000000000000, 0.000000000000000000, 0.000000000000000000 ) ) ;
#9772 = DIRECTION ( 'NONE',  ( -0.9704142011833032377, 0.000000000000000000, -0.2414462220490753985 ) ) ;
#9773 = ORIENTED_EDGE ( 'NONE', *, *, #16561, .F. ) ;
#9774 = EDGE_CURVE ( 'NONE', #12729, #8389, #359, .T. ) ;
#9775 = CARTESIAN_POINT ( 'NONE',  ( -16.70219504179999959, -100.0012196380000091, 6.767083061890000195 ) ) ;
#9776 = CARTESIAN_POINT ( 'NONE',  ( -20.32174609979999858, -45.92926717529999792, 14.70331994040000012 ) ) ;
#9777 = DIRECTION ( 'NONE',  ( 1.000000000000000000, 0.000000000000000000, 0.000000000000000000 ) ) ;
#9778 = CARTESIAN_POINT ( 'NONE',  ( 31.14753128929999804, -73.95999340959998847, -23.57268455550000041 ) ) ;
#9779 = CARTESIAN_POINT ( 'NONE',  ( 22.51510749560000235, -60.60190586809999758, -7.150863154439999647 ) ) ;
#9780 = CIRCLE ( 'NONE', #11211, 29.91857981989999971 ) ;
#9781 = CIRCLE ( 'NONE', #25149, 57.75000000000000000 ) ;
#9782 = EDGE_CURVE ( 'NONE', #11938, #6398, #28677, .T. ) ;
#9783 = CARTESIAN_POINT ( 'NONE',  ( 25.83227502339999759, -65.33654462470001079, 1.152172478150000012 ) ) ;
#9784 = B_SPLINE_CURVE_WITH_KNOTS ( 'NONE', 3,
 ( #13551, #8877, #4829, #11204 ),
 .UNSPECIFIED., .F., .F.,
 ( 4, 4 ),
 ( 0.000000000000000000, 1.000000000000000000 ),
 .UNSPECIFIED. ) ;
#9785 = LINE ( 'NONE', #27437, #27034 ) ;
#9786 = ORIENTED_EDGE ( 'NONE', *, *, #18095, .F. ) ;
#9787 = FACE_OUTER_BOUND ( 'NONE', #3590, .T. ) ;
#9788 = CARTESIAN_POINT ( 'NONE',  ( 21.54641223700000197, -36.98696877929999260, -8.488506496170000304 ) ) ;
#9789 = FACE_BOUND ( 'NONE', #9268, .T. ) ;
#9790 = ORIENTED_EDGE ( 'NONE', *, *, #28443, .F. ) ;
#9791 = LINE ( 'NONE', #6230, #12928 ) ;
#9792 = LINE ( 'NONE', #2822, #2466 ) ;
#9793 = CARTESIAN_POINT ( 'NONE',  ( 0.000000000000000000, -30.50310889129999836, 0.000000000000000000 ) ) ;
#9794 = DIRECTION ( 'NONE',  ( 1.000000000000000000, 0.000000000000000000, 0.000000000000000000 ) ) ;
#9795 = CARTESIAN_POINT ( 'NONE',  ( 9.295214654649997854, -36.51121532460000196, -22.62696043789999933 ) ) ;
#9796 = AXIS2_PLACEMENT_3D ( 'NONE', #12070, #16597, #1180 ) ;
#9797 = CARTESIAN_POINT ( 'NONE',  ( -13.83118819819999956, -92.50000000000000000, 21.42307711379999802 ) ) ;
#9798 = ORIENTED_EDGE ( 'NONE', *, *, #16973, .T. ) ;
#9799 = CARTESIAN_POINT ( 'NONE',  ( -40.20585889361907306, -74.11886065923714284, 7.247546674747338713 ) ) ;
#9800 = CARTESIAN_POINT ( 'NONE',  ( -28.43155917910000241, -92.70565333729999224, -2.447589390230000106 ) ) ;
#9801 = CARTESIAN_POINT ( 'NONE',  ( -13.31718154921655817, -19.49371677639106792, 20.06828757285913056 ) ) ;
#9802 = CARTESIAN_POINT ( 'NONE',  ( 0.000000000000000000, 4.440892098500000496E-16, 0.000000000000000000 ) ) ;
#9803 = ORIENTED_EDGE ( 'NONE', *, *, #15191, .F. ) ;
#9804 = CARTESIAN_POINT ( 'NONE',  ( 19.39131233670000043, -19.49132065570000094, -8.982198477279998983 ) ) ;
#9805 = LINE ( 'NONE', #18569, #28359 ) ;
#9806 = CARTESIAN_POINT ( 'NONE',  ( -1.560217637240000066, -26.09432050500000244, -22.44965361090000044 ) ) ;
#9807 = DIRECTION ( 'NONE',  ( 0.000000000000000000, 1.000000000000000000, 0.000000000000000000 ) ) ;
#9808 = EDGE_CURVE ( 'NONE', #8240, #16034, #20444, .T. ) ;
#9809 = ADVANCED_FACE ( 'NONE', ( #7337 ), #25618, .T. ) ;
#9810 = CARTESIAN_POINT ( 'NONE',  ( 40.70731707320000226, -84.00000000000000000, -7.215414233289999757 ) ) ;
#9811 = DIRECTION ( 'NONE',  ( 1.000000000000000000, 0.000000000000000000, 0.000000000000000000 ) ) ;
#9812 = ADVANCED_FACE ( 'NONE', ( #513 ), #20988, .F. ) ;
#9813 = CARTESIAN_POINT ( 'NONE',  ( 12.02710806035337399, -99.07183863203711383, 14.93578453548695961 ) ) ;
#9814 = CARTESIAN_POINT ( 'NONE',  ( -16.54756449519999961, -100.0429506999999916, 2.640690120740000424 ) ) ;
#9815 = ORIENTED_EDGE ( 'NONE', *, *, #6688, .F. ) ;
#9816 = CARTESIAN_POINT ( 'NONE',  ( -32.66023292530000077, -74.50000000430000568, -21.85457041679999790 ) ) ;
#9817 = LINE ( 'NONE', #25429, #12653 ) ;
#9818 = AXIS2_PLACEMENT_3D ( 'NONE', #26292, #8351, #17687 ) ;
#9819 = B_SPLINE_CURVE_WITH_KNOTS ( 'NONE', 5,
 ( #13506, #15545, #4485, #22417, #9136, #13358 ),
 .UNSPECIFIED., .F., .F.,
 ( 6, 6 ),
 ( 0.000000000000000000, 1.000000000000000000 ),
 .UNSPECIFIED. ) ;
#9820 = CIRCLE ( 'NONE', #1022, 3.000000000000002665 ) ;
#9821 = AXIS2_PLACEMENT_3D ( 'NONE', #4390, #1645, #28276 ) ;
#9822 = CARTESIAN_POINT ( 'NONE',  ( -11.71096632150000083, -94.52293512109999085, -20.87034205579999835 ) ) ;
#9823 = CARTESIAN_POINT ( 'NONE',  ( 21.05852219120000157, -34.60505771119999707, -8.113043137870000976 ) ) ;
#9824 = CARTESIAN_POINT ( 'NONE',  ( 7.230541818635105145, -73.67850591074257238, 39.46631086800589827 ) ) ;
#9825 = TOROIDAL_SURFACE ( 'NONE', #12149, 3.500000000000000000, 0.5000000000000000000 ) ;
#9826 = CARTESIAN_POINT ( 'NONE',  ( -7.322964735850000295, -98.83667233820000320, 17.15365167710000094 ) ) ;
#9827 = CARTESIAN_POINT ( 'NONE',  ( -21.52470944380124962, -93.02765837720517084, -20.24432229263281968 ) ) ;
#9828 = ADVANCED_FACE ( 'NONE', ( #218 ), #44, .T. ) ;
#9829 = LINE ( 'NONE', #2712, #16815 ) ;
#9830 = CARTESIAN_POINT ( 'NONE',  ( -5.893951993130000346E-12, -111.0000000000000000, -1.129762949859999995E-12 ) ) ;
#9831 = VERTEX_POINT ( 'NONE', #7771 ) ;
#9832 = CARTESIAN_POINT ( 'NONE',  ( -5.598527377420000839, -101.2141467319999890, 14.18131542549999935 ) ) ;
#9833 = DIRECTION ( 'NONE',  ( -1.203338504109999799E-16, -0.000000000000000000, -1.000000000000000000 ) ) ;
#9834 = EDGE_LOOP ( 'NONE', ( #6584, #25737, #19048, #15202 ) ) ;
#9835 = LINE ( 'NONE', #18743, #22944 ) ;
#9836 = CARTESIAN_POINT ( 'NONE',  ( 0.5154897680143201155, -100.1406256087915807, -17.18202921360721547 ) ) ;
#9837 = CARTESIAN_POINT ( 'NONE',  ( -7.448397597250000501, -73.97429387040000393, 38.88881331079999626 ) ) ;
#9838 = CARTESIAN_POINT ( 'NONE',  ( -12.27960098470000005, -100.1275643909999928, -11.24051300700000056 ) ) ;
#9839 = CARTESIAN_POINT ( 'NONE',  ( -14.12701123409999937, -93.90388142519999803, -21.62231189339999915 ) ) ;
#9840 = AXIS2_PLACEMENT_3D ( 'NONE', #10489, #10355, #8316 ) ;
#9841 = FACE_OUTER_BOUND ( 'NONE', #19896, .T. ) ;
#9842 = CONICAL_SURFACE ( 'NONE', #12167, 55.67692378859999280, 1.047197551199999799 ) ;
#9843 = EDGE_CURVE ( 'NONE', #5725, #23453, #14109, .T. ) ;
#9844 = AXIS2_PLACEMENT_3D ( 'NONE', #25594, #566, #16111 ) ;
#9845 = CARTESIAN_POINT ( 'NONE',  ( 11.52668943299999960, -72.21526968880000652, -27.03296487709999951 ) ) ;
#9846 = CARTESIAN_POINT ( 'NONE',  ( 23.89360401162774039, -92.87422005962199023, -18.95642123213606212 ) ) ;
#9847 = FACE_OUTER_BOUND ( 'NONE', #26862, .T. ) ;
#9848 = CARTESIAN_POINT ( 'NONE',  ( -5.679770007689999289, -80.00000000000000000, 46.75000000000000000 ) ) ;
#9849 = DIRECTION ( 'NONE',  ( 0.000000000000000000, 1.000000000000000000, 0.000000000000000000 ) ) ;
#9850 = DIRECTION ( 'NONE',  ( 0.000000000000000000, -1.000000000000000000, 0.000000000000000000 ) ) ;
#9851 = VERTEX_POINT ( 'NONE', #3262 ) ;
#9852 = CARTESIAN_POINT ( 'NONE',  ( 9.469927264672032052, -36.00000000000000000, -20.04523765350436904 ) ) ;
#9853 = ORIENTED_EDGE ( 'NONE', *, *, #11624, .F. ) ;
#9854 = AXIS2_PLACEMENT_3D ( 'NONE', #9864, #15988, #12047 ) ;
#9855 = CARTESIAN_POINT ( 'NONE',  ( -2.351527211430000097, -58.27079767440000069, -24.37373320010000199 ) ) ;
#9856 = CARTESIAN_POINT ( 'NONE',  ( -4.028625675479999835, -98.69238697990000730, 19.35340251219999885 ) ) ;
#9857 = DIRECTION ( 'NONE',  ( 0.01257738078990017563, -0.9996558222130138560, 0.02302274110720029660 ) ) ;
#9858 = ORIENTED_EDGE ( 'NONE', *, *, #1249, .T. ) ;
#9859 = ADVANCED_FACE ( 'NONE', ( #25268, #3532 ), #22938, .T. ) ;
#9860 = CYLINDRICAL_SURFACE ( 'NONE', #11143, 0.1999999999999987899 ) ;
#9861 = LINE ( 'NONE', #5063, #4703 ) ;
#9862 = CARTESIAN_POINT ( 'NONE',  ( 4.794255386040000566, -17.50000000000000000, 8.775825618900000791 ) ) ;
#9863 = VERTEX_POINT ( 'NONE', #16928 ) ;
#9864 = CARTESIAN_POINT ( 'NONE',  ( 0.000000000000000000, -2.000000000000000000, 0.000000000000000000 ) ) ;
#9865 = DIRECTION ( 'NONE',  ( -0.9890497259025925469, 0.000000000000000000, -0.1475826537639393088 ) ) ;
#9866 = CARTESIAN_POINT ( 'NONE',  ( 7.571687472095536720, -101.4628082770392297, 14.06488328537873045 ) ) ;
#9867 = FACE_OUTER_BOUND ( 'NONE', #17380, .T. ) ;
#9868 = EDGE_CURVE ( 'NONE', #22409, #5288, #11639, .T. ) ;
#9869 = CARTESIAN_POINT ( 'NONE',  ( -14.22861760630000028, -68.06112540870000771, 22.55404134810000016 ) ) ;
#9870 = ORIENTED_EDGE ( 'NONE', *, *, #4281, .F. ) ;
#9871 = CARTESIAN_POINT ( 'NONE',  ( -41.75000000000000000, -65.63577453799999262, 1.587713240270000048 ) ) ;
#9872 = CARTESIAN_POINT ( 'NONE',  ( -16.08960165530000097, -101.0043489809999926, 3.145915650070000069 ) ) ;
#9873 = CARTESIAN_POINT ( 'NONE',  ( 24.53756381369999673, -63.58862135099999335, 0.03861512792729999977 ) ) ;
#9874 = CARTESIAN_POINT ( 'NONE',  ( -6.285925807512719565, -101.5555610555536248, 14.71350185178380343 ) ) ;
#9875 = ORIENTED_EDGE ( 'NONE', *, *, #18999, .T. ) ;
#9876 = CARTESIAN_POINT ( 'NONE',  ( -18.78219790299999659, -19.46510053389999939, 11.52011550950000007 ) ) ;
#9877 = CIRCLE ( 'NONE', #26626, 7.249999999999999112 ) ;
#9878 = CARTESIAN_POINT ( 'NONE',  ( 18.88171271891879854, -18.49999999999998224, -8.341252403918135272 ) ) ;
#9879 = CARTESIAN_POINT ( 'NONE',  ( -7.919799262655152994, -100.2392017796619683, 15.16708595175554741 ) ) ;
#9880 = ORIENTED_EDGE ( 'NONE', *, *, #28165, .T. ) ;
#9881 = FACE_OUTER_BOUND ( 'NONE', #860, .T. ) ;
#9882 = CARTESIAN_POINT ( 'NONE',  ( 15.98858835731819994, -100.9570234913455664, 4.230075987765046897 ) ) ;
#9883 = CARTESIAN_POINT ( 'NONE',  ( -12.24789267329999909, -65.07443093669999712, 21.96586363990000024 ) ) ;
#9884 = ORIENTED_EDGE ( 'NONE', *, *, #22784, .F. ) ;
#9885 = B_SPLINE_SURFACE_WITH_KNOTS ( 'NONE', 5, 5, ( 
 ( #8422, #26220, #4057, #12923, #1615, #24024 ),
 ( #8156, #21840, #1893, #10731, #8571, #10879 ),
 ( #17475, #28669, #19231, #14711, #28119, #25933 ),
 ( #23743, #13821, #26808, #11475, #20381, #11018 ),
 ( #6543, #19932, #4940, #17915, #6840, #15705 ),
 ( #20092, #17617, #15406, #6992, #4359, #451 ),
 ( #16005, #9009, #24611, #22727, #6, #15856 ),
 ( #7138, #9300, #18201, #22583, #24766, #4648 ),
 ( #22435, #13374, #155, #603, #9148, #4499 ) ),
 .UNSPECIFIED., .F., .F., .F.,
 ( 6, 3, 6 ),
 ( 6, 6 ),
 ( 1.594447291550000054E-15, 2.252774941530000241, 5.576981603840000190 ),
 ( 0.000000000000000000, 1.000000000000000000 ),
 .UNSPECIFIED. ) ;
#9886 = FACE_OUTER_BOUND ( 'NONE', #14794, .T. ) ;
#9887 = CYLINDRICAL_SURFACE ( 'NONE', #5935, 0.5000000000000004441 ) ;
#9888 = ORIENTED_EDGE ( 'NONE', *, *, #2963, .F. ) ;
#9889 = CARTESIAN_POINT ( 'NONE',  ( 47.25006817639999923, -74.77883526400000846, -0.5535757861789999401 ) ) ;
#9890 = ORIENTED_EDGE ( 'NONE', *, *, #25014, .T. ) ;
#9891 = VECTOR ( 'NONE', #7727, 1000.000000000000000 ) ;
#9892 = VECTOR ( 'NONE', #25375, 1000.000000000000000 ) ;
#9893 = B_SPLINE_CURVE_WITH_KNOTS ( 'NONE', 3,
 ( #683, #27323, #7364, #8476, #8067, #17520, #17378, #26271, #6436, #17231, #17086, #10228, #1663, #14885, #21892, #8618, #3693, #14749, #19139 ),
 .UNSPECIFIED., .F., .F.,
 ( 4, 2, 2, 2, 1, 1, 1, 1, 1, 2, 2, 4 ),
 ( 0.000000000000000000, 0.2500000000000162648, 0.3750000000000244804, 0.4375000000000285882, 0.4687500000000299760, 0.4843750000000301981, 0.4921875000000297540, 0.4960937500000293654, 0.4980468750000286993, 0.4990234375000283662, 0.5000000000000279776, 1.000000000000000000 ),
 .UNSPECIFIED. ) ;
#9894 = VERTEX_POINT ( 'NONE', #9648 ) ;
#9895 = EDGE_CURVE ( 'NONE', #19383, #10333, #1225, .T. ) ;
#9896 = CIRCLE ( 'NONE', #4791, 15.19391340349999986 ) ;
#9897 = DIRECTION ( 'NONE',  ( 0.8775825618903718706, 0.000000000000000000, 0.4794255386042046152 ) ) ;
#9898 = EDGE_CURVE ( 'NONE', #27709, #19799, #14031, .T. ) ;
#9899 = B_SPLINE_CURVE_WITH_KNOTS ( 'NONE', 5,
 ( #11369, #9336, #24499, #4532, #20273, #25094 ),
 .UNSPECIFIED., .F., .F.,
 ( 6, 6 ),
 ( 0.000000000000000000, 1.000000000000000000 ),
 .UNSPECIFIED. ) ;
#9900 = CARTESIAN_POINT ( 'NONE',  ( 39.96405812750000308, -74.08838618730000292, 7.268564243930000224 ) ) ;
#9901 = CARTESIAN_POINT ( 'NONE',  ( -20.43932202180000246, -94.59276292389999696, 12.18704577789999988 ) ) ;
#9902 = CARTESIAN_POINT ( 'NONE',  ( -15.50938051129999984, -101.3150705480000084, 4.855933523060000034 ) ) ;
#9903 = EDGE_CURVE ( 'NONE', #22563, #4998, #2364, .T. ) ;
#9904 = CARTESIAN_POINT ( 'NONE',  ( 0.000000000000000000, -19.09689110869999951, 0.000000000000000000 ) ) ;
#9905 = CARTESIAN_POINT ( 'NONE',  ( 8.188637977920000921, -100.9197082849999987, 13.30686163390000054 ) ) ;
#9906 = ORIENTED_EDGE ( 'NONE', *, *, #1851, .T. ) ;
#9907 = ADVANCED_FACE ( 'NONE', ( #5297 ), #18704, .T. ) ;
#9908 = CARTESIAN_POINT ( 'NONE',  ( -32.64087606319999679, -79.95649630820000198, -22.33050332599999876 ) ) ;
#9909 = CARTESIAN_POINT ( 'NONE',  ( -41.75000000000000000, -65.00000000000000000, 2.684678751729999480 ) ) ;
#9910 = CARTESIAN_POINT ( 'NONE',  ( 0.000000000000000000, -2.000000000000000000, 0.000000000000000000 ) ) ;
#9911 = CARTESIAN_POINT ( 'NONE',  ( 23.99827830379999583, -92.84292833370000153, -18.61030780140000118 ) ) ;
#9912 = ORIENTED_EDGE ( 'NONE', *, *, #17642, .T. ) ;
#9913 = CARTESIAN_POINT ( 'NONE',  ( -0.7591504320660000804, -79.66564775870000403, 47.25050659409999554 ) ) ;
#9914 = CARTESIAN_POINT ( 'NONE',  ( 7.584268328590000330, -101.6484612600000048, 14.08825304710000026 ) ) ;
#9915 = ORIENTED_EDGE ( 'NONE', *, *, #10325, .F. ) ;
#9916 = DIRECTION ( 'NONE',  ( 0.000000000000000000, -1.000000000000000000, 0.000000000000000000 ) ) ;
#9917 = CARTESIAN_POINT ( 'NONE',  ( 0.000000000000000000, -56.78056608349999834, 0.000000000000000000 ) ) ;
#9918 = DIRECTION ( 'NONE',  ( 0.000000000000000000, -1.000000000000000000, 0.000000000000000000 ) ) ;
#9919 = CARTESIAN_POINT ( 'NONE',  ( 27.75394116159999669, -74.50000000000000000, -27.75394116159999669 ) ) ;
#9920 = CARTESIAN_POINT ( 'NONE',  ( -14.49490684773424931, -74.10099149224471660, 36.26165015395787350 ) ) ;
#9921 = AXIS2_PLACEMENT_3D ( 'NONE', #17647, #6569, #11043 ) ;
#9922 = CARTESIAN_POINT ( 'NONE',  ( -41.75000000000000000, -63.07912966450000880, 2.684678751729999480 ) ) ;
#9923 = ORIENTED_EDGE ( 'NONE', *, *, #10481, .T. ) ;
#9924 = CARTESIAN_POINT ( 'NONE',  ( 0.000000000000000000, -111.0000000000000000, 0.000000000000000000 ) ) ;
#9925 = CIRCLE ( 'NONE', #18794, 39.25000000000000000 ) ;
#9926 = CARTESIAN_POINT ( 'NONE',  ( 20.58520128069999799, -36.04995792020000067, -8.980828480690000504 ) ) ;
#9927 = DIRECTION ( 'NONE',  ( 0.9387128607161809857, 0.000000000000000000, 0.3447001089730665768 ) ) ;
#9928 = ORIENTED_EDGE ( 'NONE', *, *, #8436, .F. ) ;
#9929 = CARTESIAN_POINT ( 'NONE',  ( 27.23269985219999967, -92.50000000000000000, -12.38957130830000075 ) ) ;
#9930 = ADVANCED_FACE ( 'NONE', ( #3395 ), #8379, .F. ) ;
#9931 = CARTESIAN_POINT ( 'NONE',  ( -21.10814673583525902, -64.47177029419442817, 15.24425173043963966 ) ) ;
#9932 = CARTESIAN_POINT ( 'NONE',  ( -8.001416342079998856, -100.4792519539999915, 14.07906887139999874 ) ) ;
#9933 = CARTESIAN_POINT ( 'NONE',  ( 6.103564891039999551, -92.56168957700000988, 29.00427579219999785 ) ) ;
#9934 = FACE_OUTER_BOUND ( 'NONE', #16971, .T. ) ;
#9935 = FACE_OUTER_BOUND ( 'NONE', #1468, .T. ) ;
#9936 = EDGE_LOOP ( 'NONE', ( #7903, #19206, #14221, #14510 ) ) ;
#9937 = EDGE_CURVE ( 'NONE', #12917, #2214, #7817, .T. ) ;
#9938 = DIRECTION ( 'NONE',  ( 0.000000000000000000, 1.000000000000000000, 0.000000000000000000 ) ) ;
#9939 = CARTESIAN_POINT ( 'NONE',  ( 24.05376935019999962, -19.40595403639999716, 1.523939926209999962 ) ) ;
#9940 = CARTESIAN_POINT ( 'NONE',  ( -12.99499290521388595, -19.48483198002087491, 19.65355774919085263 ) ) ;
#9941 = CARTESIAN_POINT ( 'NONE',  ( 23.19910953469999981, -45.76350410940000302, -9.457696755039998848 ) ) ;
#9942 = ORIENTED_EDGE ( 'NONE', *, *, #16399, .T. ) ;
#9943 = CARTESIAN_POINT ( 'NONE',  ( 19.61724684530000218, -18.50000000000000000, -7.593153726179999730 ) ) ;
#9944 = CARTESIAN_POINT ( 'NONE',  ( -16.54318588419999969, -111.0000000000000000, 25.62368046950000178 ) ) ;
#9945 = CARTESIAN_POINT ( 'NONE',  ( -0.8962089411180000909, -26.09894693429999890, -22.24995341260000359 ) ) ;
#9946 = CARTESIAN_POINT ( 'NONE',  ( -17.56187199568302759, -92.66972459457754496, 24.93653312871382255 ) ) ;
#9947 = AXIS2_PLACEMENT_3D ( 'NONE', #8573, #17477, #2040 ) ;
#9948 = FACE_OUTER_BOUND ( 'NONE', #18726, .T. ) ;
#9949 = AXIS2_PLACEMENT_3D ( 'NONE', #18060, #6847, #11629 ) ;
#9950 = CARTESIAN_POINT ( 'NONE',  ( 20.06309763089999620, -36.00000000000000000, -9.476129751679998492 ) ) ;
#9951 = CARTESIAN_POINT ( 'NONE',  ( 13.86409537477300624, -98.07566823408926382, 15.06275398214450156 ) ) ;
#9952 = CARTESIAN_POINT ( 'NONE',  ( -40.50000000000000000, -65.63577453799999262, 2.309401076760000393 ) ) ;
#9953 = ORIENTED_EDGE ( 'NONE', *, *, #23090, .T. ) ;
#9954 = B_SPLINE_CURVE_WITH_KNOTS ( 'NONE', 5,
 ( #13261, #4678, #13857, #24352, #22312, #24649, #22762, #18085, #24798, #24495, #20417, #2509 ),
 .UNSPECIFIED., .F., .F.,
 ( 6, 3, 3, 6 ),
 ( 0.000000000000000000, 0.2674763062605450825, 0.5735529784659251229, 1.000000000000000000 ),
 .UNSPECIFIED. ) ;
#9955 = DIRECTION ( 'NONE',  ( 0.000000000000000000, -1.000000000000000000, 0.000000000000000000 ) ) ;
#9956 = CARTESIAN_POINT ( 'NONE',  ( -21.71458329359999695, -74.50000000000000000, -32.69645379630000548 ) ) ;
#9957 = CARTESIAN_POINT ( 'NONE',  ( -11.44873198189999819, -94.64875831279999829, -20.83031290489999776 ) ) ;
#9958 = CARTESIAN_POINT ( 'NONE',  ( 7.882323183639998732, -36.30033153219999775, -21.44286902610000212 ) ) ;
#9959 = CARTESIAN_POINT ( 'NONE',  ( 4.500000000000000000, -12.50000000000000000, 50.00000000000000000 ) ) ;
#9960 = ADVANCED_FACE ( 'NONE', ( #7905 ), #11736, .F. ) ;
#9961 = CARTESIAN_POINT ( 'NONE',  ( 23.52622212079999997, -57.40875702419999982, -9.564509902230000193 ) ) ;
#9962 = CARTESIAN_POINT ( 'NONE',  ( -13.66168260340000096, -74.00000000000000000, -27.27344781959999764 ) ) ;
#9963 = DIRECTION ( 'NONE',  ( -0.1038897333389494221, 0.000000000000000000, -0.9945888212255162841 ) ) ;
#9964 = EDGE_CURVE ( 'NONE', #3752, #5075, #19105, .T. ) ;
#9965 = DIRECTION ( 'NONE',  ( 1.000000000000000000, 0.000000000000000000, 0.000000000000000000 ) ) ;
#9966 = ORIENTED_EDGE ( 'NONE', *, *, #21108, .F. ) ;
#9967 = AXIS2_PLACEMENT_3D ( 'NONE', #18978, #3946, #21581 ) ;
#9968 = DIRECTION ( 'NONE',  ( 0.1166882174331227151, -0.3326668106479456766, -0.9357973354341229122 ) ) ;
#9969 = CARTESIAN_POINT ( 'NONE',  ( 0.000000000000000000, -111.0000000000000000, 0.000000000000000000 ) ) ;
#9970 = ORIENTED_EDGE ( 'NONE', *, *, #6313, .F. ) ;
#9971 = CARTESIAN_POINT ( 'NONE',  ( 26.38214758550000028, -68.90972672860000614, -11.00107854260000018 ) ) ;
#9972 = EDGE_CURVE ( 'NONE', #10466, #321, #16310, .T. ) ;
#9973 = CARTESIAN_POINT ( 'NONE',  ( 0.3020942853670610106, -101.4304678898396332, -16.16567993605933395 ) ) ;
#9974 = CARTESIAN_POINT ( 'NONE',  ( -7.263337524479998919, -73.89694774980000602, 39.48646518750000212 ) ) ;
#9975 = CARTESIAN_POINT ( 'NONE',  ( 13.34729337145036965, -92.71619979444699311, 27.42443759431768058 ) ) ;
#9976 = CARTESIAN_POINT ( 'NONE',  ( -13.38017493169999916, -94.34469964500000572, -21.61746068469999926 ) ) ;
#9977 =( GEOMETRIC_REPRESENTATION_CONTEXT ( 3 ) GLOBAL_UNCERTAINTY_ASSIGNED_CONTEXT ( ( #7731 ) ) GLOBAL_UNIT_ASSIGNED_CONTEXT ( ( #6474, #25872, #1974 ) ) REPRESENTATION_CONTEXT ( 'NONE', 'WORKASPACE' ) );
#9978 = CARTESIAN_POINT ( 'NONE',  ( 21.93491260069999882, -72.48668981500000541, -30.95810316469999890 ) ) ;
#9979 = CARTESIAN_POINT ( 'NONE',  ( -22.80702985319999954, -71.67701549839999586, 16.52030771659999786 ) ) ;
#9980 = CARTESIAN_POINT ( 'NONE',  ( -18.26810397560000254, -94.98812477769999418, 16.32728546869999775 ) ) ;
#9981 = CIRCLE ( 'NONE', #7217, 23.36116116979999902 ) ;
#9982 = CARTESIAN_POINT ( 'NONE',  ( -14.73065703798407711, -101.1848546039999945, 4.068069545059747050 ) ) ;
#9983 = CARTESIAN_POINT ( 'NONE',  ( 8.815774981519998832, -19.46527873000000142, -19.82451640119999681 ) ) ;
#9984 = CARTESIAN_POINT ( 'NONE',  ( -10.73867332049999845, -11.85850980319999870, -19.65700966069999822 ) ) ;
#9985 = CARTESIAN_POINT ( 'NONE',  ( -41.68173630718685274, -63.05366661935899231, 2.839229858532883455 ) ) ;
#9986 = ORIENTED_EDGE ( 'NONE', *, *, #27633, .F. ) ;
#9987 = EDGE_CURVE ( 'NONE', #12325, #11391, #6532, .T. ) ;
#9988 = AXIS2_PLACEMENT_3D ( 'NONE', #3413, #1110, #21459 ) ;
#9989 = ORIENTED_EDGE ( 'NONE', *, *, #22620, .T. ) ;
#9990 = LINE ( 'NONE', #863, #20702 ) ;
#9991 = CARTESIAN_POINT ( 'NONE',  ( -28.68689398529999934, -92.57423544259999915, 3.199804733899999754 ) ) ;
#9992 = CARTESIAN_POINT ( 'NONE',  ( 1.776356839399999804E-15, -101.6484611540000031, -1.776356839399999804E-15 ) ) ;
#9993 = EDGE_CURVE ( 'NONE', #25766, #23252, #5977, .T. ) ;
#9994 = CARTESIAN_POINT ( 'NONE',  ( -0.08129961819659545230, -95.57586223754451282, 22.58573869906598830 ) ) ;
#9995 = CARTESIAN_POINT ( 'NONE',  ( -7.135467304789999687, -73.50000064450000536, 38.71640881029999548 ) ) ;
#9996 = CARTESIAN_POINT ( 'NONE',  ( -7.315286554515622264, -74.28332971673216889, -40.00438978215803587 ) ) ;
#9997 = VERTEX_POINT ( 'NONE', #6407 ) ;
#9998 = CARTESIAN_POINT ( 'NONE',  ( 9.374849361280000792, -94.98812477599999227, -22.63660904189999812 ) ) ;
#9999 = CARTESIAN_POINT ( 'NONE',  ( 7.954809540590000339, -36.56645929769999981, -21.41760928989999968 ) ) ;
#10000 = ADVANCED_FACE ( 'NONE', ( #23763, #1637 ), #8446, .T. ) ;
#10001 = B_SPLINE_CURVE_WITH_KNOTS ( 'NONE', 3,
 ( #5659, #23448, #9742, #22881, #27394, #27547 ),
 .UNSPECIFIED., .F., .F.,
 ( 4, 2, 4 ),
 ( 0.000000000000000000, 0.5000000000000000000, 1.000000000000000000 ),
 .UNSPECIFIED. ) ;
#10002 = CARTESIAN_POINT ( 'NONE',  ( 26.21017338629999927, -93.14733690340000294, -7.956146379909999844 ) ) ;
#10003 = CARTESIAN_POINT ( 'NONE',  ( -13.80673663610000013, -68.20222181140000828, 22.71145995190000377 ) ) ;
#10004 = VERTEX_POINT ( 'NONE', #26242 ) ;
#10005 = DIRECTION ( 'NONE',  ( 1.000000000000000000, 0.000000000000000000, 0.000000000000000000 ) ) ;
#10006 = CARTESIAN_POINT ( 'NONE',  ( -15.63746481129999921, -100.7880644439999998, 2.916848959350000214 ) ) ;
#10007 = CARTESIAN_POINT ( 'NONE',  ( 23.80217619240000104, -60.55397095009999475, 0.3124424936219999949 ) ) ;
#10008 = CARTESIAN_POINT ( 'NONE',  ( -20.01779683490000039, -60.59309307459999872, 12.54531749399999896 ) ) ;
#10009 = ORIENTED_EDGE ( 'NONE', *, *, #26448, .F. ) ;
#10010 = CARTESIAN_POINT ( 'NONE',  ( 24.31832408829999892, -64.48635707210000589, -9.855635234570000236 ) ) ;
#10011 = CARTESIAN_POINT ( 'NONE',  ( 18.94592261899999741, -19.50000000000000000, -9.024080787800000891 ) ) ;
#10012 = FACE_BOUND ( 'NONE', #22202, .T. ) ;
#10013 = ORIENTED_EDGE ( 'NONE', *, *, #10404, .F. ) ;
#10014 = EDGE_CURVE ( 'NONE', #10287, #3233, #5020, .T. ) ;
#10015 = AXIS2_PLACEMENT_3D ( 'NONE', #2476, #22136, #4798 ) ;
#10016 = CARTESIAN_POINT ( 'NONE',  ( -41.75000000001212896, -65.13413837703322429, -2.717007628343222958 ) ) ;
#10017 = CARTESIAN_POINT ( 'NONE',  ( -41.82835010422233069, -65.73761215452407214, -1.198860239817544748 ) ) ;
#10018 = CARTESIAN_POINT ( 'NONE',  ( 36.62206425559999445, -80.26271606740000664, -14.12235947189999941 ) ) ;
#10019 = FACE_OUTER_BOUND ( 'NONE', #4471, .T. ) ;
#10020 = EDGE_LOOP ( 'NONE', ( #16738, #3656, #21072, #15656 ) ) ;
#10021 = ADVANCED_FACE ( 'NONE', ( #23256 ), #18260, .T. ) ;
#10022 = CARTESIAN_POINT ( 'NONE',  ( 6.748482936971252677, -100.5798851012459210, 15.42610337842955026 ) ) ;
#10023 = CARTESIAN_POINT ( 'NONE',  ( 10.00000000000000000, -19.00000000000000000, 0.000000000000000000 ) ) ;
#10024 = ORIENTED_EDGE ( 'NONE', *, *, #25799, .T. ) ;
#10025 = CARTESIAN_POINT ( 'NONE',  ( 46.37168807673121762, -73.60877760474707543, -3.458991447863533963 ) ) ;
#10026 = ORIENTED_EDGE ( 'NONE', *, *, #6811, .F. ) ;
#10027 = CARTESIAN_POINT ( 'NONE',  ( -13.26444742760000040, -34.62271398969999581, 20.17275320750000134 ) ) ;
#10028 = CARTESIAN_POINT ( 'NONE',  ( -6.285925807579999969, -101.6484611540000031, 14.71350185179999848 ) ) ;
#10029 = EDGE_LOOP ( 'NONE', ( #15675, #3901, #3803, #11032 ) ) ;
#10030 = CARTESIAN_POINT ( 'NONE',  ( -6.124560390765033446, -95.75133629536016144, -21.89659062549250734 ) ) ;
#10031 = EDGE_LOOP ( 'NONE', ( #18784, #13387, #22150, #4178, #16109, #4119, #7280 ) ) ;
#10032 = CARTESIAN_POINT ( 'NONE',  ( 38.65569830309999588, -74.00000023179998720, 7.472969336320000266 ) ) ;
#10033 = CARTESIAN_POINT ( 'NONE',  ( -12.97641886767416430, -101.6484611540000031, -9.360302276478243755 ) ) ;
#10034 = CARTESIAN_POINT ( 'NONE',  ( -11.80701538218819913, -63.17441371568864383, -23.36682876523914842 ) ) ;
#10035 = CARTESIAN_POINT ( 'NONE',  ( 46.83762086372372124, -79.80981178139894894, -3.035625116143169322 ) ) ;
#10036 = ORIENTED_EDGE ( 'NONE', *, *, #28003, .F. ) ;
#10037 = CARTESIAN_POINT ( 'NONE',  ( -32.35914374060000398, -80.34842067969999846, -22.21527698039999876 ) ) ;
#10038 = CARTESIAN_POINT ( 'NONE',  ( 16.76737182020000105, -99.57787118749999422, 4.489257787179999681 ) ) ;
#10039 = CARTESIAN_POINT ( 'NONE',  ( 16.22917866779999940, -99.91102932019998661, 4.812753184709999132 ) ) ;
#10040 = ORIENTED_EDGE ( 'NONE', *, *, #19423, .F. ) ;
#10041 = AXIS2_PLACEMENT_3D ( 'NONE', #13011, #21922, #28614 ) ;
#10042 = FACE_OUTER_BOUND ( 'NONE', #24546, .T. ) ;
#10043 = CARTESIAN_POINT ( 'NONE',  ( -12.94585355959999973, -101.6484611540000031, -9.402386697720000797 ) ) ;
#10044 = ORIENTED_EDGE ( 'NONE', *, *, #7964, .T. ) ;
#10045 = DIRECTION ( 'NONE',  ( 0.000000000000000000, -1.000000000000000000, 0.000000000000000000 ) ) ;
#10046 = DIRECTION ( 'NONE',  ( 0.4794255386042042266, 0.000000000000000000, 0.8775825618903720926 ) ) ;
#10047 = CARTESIAN_POINT ( 'NONE',  ( 23.17124894566643434, -95.36087493982624608, -1.748483809854802118 ) ) ;
#10048 = CARTESIAN_POINT ( 'NONE',  ( 30.92226875830000310, -72.24519481100000462, -21.98812938469999878 ) ) ;
#10049 = EDGE_CURVE ( 'NONE', #25778, #27814, #520, .T. ) ;
#10050 = CARTESIAN_POINT ( 'NONE',  ( -15.34661535209604644, -72.13193952715772639, 23.85822615002545888 ) ) ;
#10051 = EDGE_CURVE ( 'NONE', #4550, #14431, #4192, .T. ) ;
#10052 = B_SPLINE_CURVE_WITH_KNOTS ( 'NONE', 5,
 ( #10186, #10324, #8163, #17049, #23750, #1622 ),
 .UNSPECIFIED., .F., .F.,
 ( 6, 6 ),
 ( 0.000000000000000000, 1.000000000000000000 ),
 .UNSPECIFIED. ) ;
#10053 = B_SPLINE_SURFACE_WITH_KNOTS ( 'NONE', 5, 5, ( 
 ( #654, #9060, #11072, #26856, #15762, #2821 ),
 ( #19990, #9201, #7193, #510, #11531, #22489 ),
 ( #6897, #24668, #4701, #11386, #20288, #18114 ),
 ( #27006, #7045, #15912, #24818, #4857, #9356 ),
 ( #18257, #27153, #11681, #9506, #25114, #5144 ),
 ( #14026, #5939, #25403, #16355, #17162, #8140 ) ),
 .UNSPECIFIED., .F., .F., .F.,
 ( 6, 6 ),
 ( 6, 6 ),
 ( 2.788355763089999773, 6.107000906319999700 ),
 ( 0.000000000000000000, 0.5000000000000000000 ),
 .UNSPECIFIED. ) ;
#10054 = EDGE_CURVE ( 'NONE', #16224, #12521, #8870, .T. ) ;
#10055 = B_SPLINE_CURVE_WITH_KNOTS ( 'NONE', 5,
 ( #7425, #5378, #5651, #5232, #23016, #18641, #18922, #3335, #21245 ),
 .UNSPECIFIED., .F., .F.,
 ( 6, 3, 6 ),
 ( -1.134864905219999942, -0.9962660581400000215, 0.000000000000000000 ),
 .UNSPECIFIED. ) ;
#10056 = EDGE_CURVE ( 'NONE', #25273, #6167, #18237, .T. ) ;
#10057 = ORIENTED_EDGE ( 'NONE', *, *, #13066, .T. ) ;
#10058 = CARTESIAN_POINT ( 'NONE',  ( 8.883150714079999233, -37.96517267130000306, -22.08524768410000050 ) ) ;
#10059 = CARTESIAN_POINT ( 'NONE',  ( 20.01429411540000203, -35.44265700830000299, -8.963580768409999067 ) ) ;
#10060 = CARTESIAN_POINT ( 'NONE',  ( 21.16092811309999888, -36.40219747150000273, -8.702541777570001358 ) ) ;
#10061 = PLANE ( 'NONE',  #18636 ) ;
#10062 = ORIENTED_EDGE ( 'NONE', *, *, #17974, .T. ) ;
#10063 = CARTESIAN_POINT ( 'NONE',  ( -12.92849772029999933, -101.3256027080000052, -9.267492799690000282 ) ) ;
#10064 = CARTESIAN_POINT ( 'NONE',  ( 23.92053897610000135, -91.50000000000000000, -18.92241567810000191 ) ) ;
#10065 = CARTESIAN_POINT ( 'NONE',  ( -1.869204707399999776, -93.63284696360000225, 25.01358039600000183 ) ) ;
#10066 = DIRECTION ( 'NONE',  ( 0.000000000000000000, -1.000000000000000000, 0.000000000000000000 ) ) ;
#10067 = CARTESIAN_POINT ( 'NONE',  ( 7.243954325790000759, -101.1848542809999856, 13.45609835219999972 ) ) ;
#10068 = ORIENTED_EDGE ( 'NONE', *, *, #17432, .T. ) ;
#10069 = CARTESIAN_POINT ( 'NONE',  ( 0.000000000000000000, -83.75000000000000000, 0.000000000000000000 ) ) ;
#10070 = LINE ( 'NONE', #12533, #15361 ) ;
#10071 = CARTESIAN_POINT ( 'NONE',  ( -10.20110288159999890, -84.00000000000000000, -41.00000000000000000 ) ) ;
#10072 = ORIENTED_EDGE ( 'NONE', *, *, #4415, .T. ) ;
#10073 = DIRECTION ( 'NONE',  ( 0.000000000000000000, 1.000000000000000000, 0.000000000000000000 ) ) ;
#10074 = B_SPLINE_CURVE_WITH_KNOTS ( 'NONE', 5,
 ( #10011, #7722, #27805, #16877, #9878, #7847 ),
 .UNSPECIFIED., .F., .F.,
 ( 6, 6 ),
 ( 0.000000000000000000, 1.000000000000000000 ),
 .UNSPECIFIED. ) ;
#10075 = CARTESIAN_POINT ( 'NONE',  ( -14.51516215540000054, -74.22762369209999633, 36.44028598479999914 ) ) ;
#10076 = CARTESIAN_POINT ( 'NONE',  ( -14.94461375770000089, -74.50000000000000000, 45.97940633559999668 ) ) ;
#10077 = CARTESIAN_POINT ( 'NONE',  ( -16.86265888959999870, -74.50000000000000000, 45.21850545039999503 ) ) ;
#10078 = B_SPLINE_CURVE_WITH_KNOTS ( 'NONE', 5,
 ( #23156, #600, #27385, #20379, #3068, #9876 ),
 .UNSPECIFIED., .F., .F.,
 ( 6, 6 ),
 ( 0.000000000000000000, 46.92787229080000344 ),
 .UNSPECIFIED. ) ;
#10079 = DIRECTION ( 'NONE',  ( 0.000000000000000000, -1.000000000000000000, 0.000000000000000000 ) ) ;
#10080 = CARTESIAN_POINT ( 'NONE',  ( -0.1776101844839999833, -101.4254868729999970, -15.96796905659999766 ) ) ;
#10081 = CARTESIAN_POINT ( 'NONE',  ( 12.72804228091459144, -98.68740076101950365, 15.00358873733218168 ) ) ;
#10082 = CARTESIAN_POINT ( 'NONE',  ( -10.97670906379999956, -34.61119146809999592, -21.88132632449999804 ) ) ;
#10083 = VERTEX_POINT ( 'NONE', #16025 ) ;
#10084 = EDGE_CURVE ( 'NONE', #19884, #13409, #27277, .T. ) ;
#10085 = CARTESIAN_POINT ( 'NONE',  ( 6.638238976540000280, -100.0496341300000154, 15.55554575080000035 ) ) ;
#10086 = CARTESIAN_POINT ( 'NONE',  ( 13.56781805022574439, -96.36359511437918002, -17.24825640581852326 ) ) ;
#10087 = CARTESIAN_POINT ( 'NONE',  ( 7.642202223189999977, -101.1334489860000048, 13.31223315789999972 ) ) ;
#10088 = EDGE_CURVE ( 'NONE', #6300, #2641, #24099, .T. ) ;
#10089 = CARTESIAN_POINT ( 'NONE',  ( 10.00000000000000000, -42.50000000000000000, -2.449212707639999657E-15 ) ) ;
#10090 = CARTESIAN_POINT ( 'NONE',  ( 8.408940298639999256, -35.33620340770000468, -20.95510887249999854 ) ) ;
#10091 = CARTESIAN_POINT ( 'NONE',  ( 7.221517031000784570, -73.63371395842501954, 39.35783505868155174 ) ) ;
#10092 = CARTESIAN_POINT ( 'NONE',  ( 25.91186513281249404, -93.33134965530122429, -7.488690889712852794 ) ) ;
#10093 = DIRECTION ( 'NONE',  ( 0.000000000000000000, -1.000000000000000000, 0.000000000000000000 ) ) ;
#10094 = CIRCLE ( 'NONE', #7344, 23.79684788999999867 ) ;
#10095 = ORIENTED_EDGE ( 'NONE', *, *, #4173, .F. ) ;
#10096 = CARTESIAN_POINT ( 'NONE',  ( 10.33698150750000089, -74.00000000000000000, -28.69894320070000049 ) ) ;
#10097 = CYLINDRICAL_SURFACE ( 'NONE', #23673, 11.00000000000000000 ) ;
#10098 = ORIENTED_EDGE ( 'NONE', *, *, #8897, .T. ) ;
#10099 = CIRCLE ( 'NONE', #20828, 9.499999999999998224 ) ;
#10100 = CARTESIAN_POINT ( 'NONE',  ( 0.000000000000000000, -2.000000000000000000, 0.000000000000000000 ) ) ;
#10101 = VERTEX_POINT ( 'NONE', #22007 ) ;
#10102 = DIRECTION ( 'NONE',  ( 1.000000000000000000, 0.000000000000000000, 0.000000000000000000 ) ) ;
#10103 = FACE_OUTER_BOUND ( 'NONE', #21192, .T. ) ;
#10104 = CARTESIAN_POINT ( 'NONE',  ( 10.50000000000000000, -89.50000000000000000, 0.000000000000000000 ) ) ;
#10105 = CARTESIAN_POINT ( 'NONE',  ( 26.50110885399999816, -74.25067683309998756, -29.00949035939999732 ) ) ;
#10106 = DIRECTION ( 'NONE',  ( 0.000000000000000000, -1.000000000000000000, 0.000000000000000000 ) ) ;
#10107 = B_SPLINE_SURFACE_WITH_KNOTS ( 'NONE', 5, 5, ( 
 ( #27661, #22698, #9421, #16566, #18328, #16123, #13947, #16850, #12732 ),
 ( #25743, #15061, #16702, #14923, #3453, #1419, #12320, #14784, #23685 ),
 ( #28196, #23970, #1560, #12180, #10403, #8229, #1153, #17125, #4985 ),
 ( #4147, #18404, #7040, #20436, #22083, #10964, #1835, #28755, #28481 ),
 ( #18108, #22630, #6333, #24113, #1982, #10825, #8653, #6483, #10058 ),
 ( #7487, #14583, #7899, #3524, #9638, #27593, #21027, #5426, #10193 ) ),
 .UNSPECIFIED., .F., .F., .F.,
 ( 6, 6 ),
 ( 6, 3, 6 ),
 ( 0.000000000000000000, 2.709627183969999908 ),
 ( 0.000000000000000000, 1.000000000000000000, 2.000000000000000000 ),
 .UNSPECIFIED. ) ;
#10109 = EDGE_CURVE ( 'NONE', #767, #17600, #20499, .T. ) ;
#10108 = CARTESIAN_POINT ( 'NONE',  ( 11.77817022719999862, -101.0685849509999912, -10.96540529560000010 ) ) ;
#10110 = DIRECTION ( 'NONE',  ( 0.9919319056295825554, 0.000000000000000000, 0.1267718209779474525 ) ) ;
#10111 = CARTESIAN_POINT ( 'NONE',  ( -2.565530488236128726, -57.41946962537819843, -24.92670969134982073 ) ) ;
#10112 = CARTESIAN_POINT ( 'NONE',  ( -41.48056608648862920, -63.07120704560056623, 2.875531170741493447 ) ) ;
#10113 = ORIENTED_EDGE ( 'NONE', *, *, #18813, .F. ) ;
#10114 = EDGE_CURVE ( 'NONE', #4043, #9863, #24698, .T. ) ;
#10115 = DIRECTION ( 'NONE',  ( 0.000000000000000000, -1.000000000000000000, 0.000000000000000000 ) ) ;
#10116 = VECTOR ( 'NONE', #11793, 1000.000000000000114 ) ;
#10117 = CIRCLE ( 'NONE', #18965, 18.14285714289999873 ) ;
#10118 = ORIENTED_EDGE ( 'NONE', *, *, #16884, .T. ) ;
#10119 = CARTESIAN_POINT ( 'NONE',  ( -33.25000000000000000, -69.00000000000000000, 2.267215112510000273E-15 ) ) ;
#10120 = EDGE_CURVE ( 'NONE', #26131, #519, #4665, .T. ) ;
#10121 = DIRECTION ( 'NONE',  ( 0.4794255386042036715, 0.000000000000000000, 0.8775825618903724257 ) ) ;
#10122 = AXIS2_PLACEMENT_3D ( 'NONE', #8125, #3482, #23164 ) ;
#10123 = CARTESIAN_POINT ( 'NONE',  ( -29.43810879609999986, -92.99999932709999939, 4.713437748839999664 ) ) ;
#10124 = CARTESIAN_POINT ( 'NONE',  ( 9.108768439514689064, -94.52419745025660802, -22.22443064656424383 ) ) ;
#10125 = EDGE_LOOP ( 'NONE', ( #22521, #13197 ) ) ;
#10126 = DIRECTION ( 'NONE',  ( 0.000000000000000000, -1.000000000000000000, 0.000000000000000000 ) ) ;
#10127 = ORIENTED_EDGE ( 'NONE', *, *, #9166, .F. ) ;
#10128 = CARTESIAN_POINT ( 'NONE',  ( -40.00000000000000000, -65.84529946160000691, 0.000000000000000000 ) ) ;
#10129 = CARTESIAN_POINT ( 'NONE',  ( 9.079731074819999748, -35.79879667440000190, -19.54912311329999852 ) ) ;
#10130 = CIRCLE ( 'NONE', #9693, 23.79684788999999867 ) ;
#10131 = CARTESIAN_POINT ( 'NONE',  ( -14.93121042630000161, -79.81259640750000983, 36.29905572410000048 ) ) ;
#10132 = CARTESIAN_POINT ( 'NONE',  ( -41.75000000000000000, -65.56519245710001087, 1.769653913539999790 ) ) ;
#10133 = CIRCLE ( 'NONE', #13882, 0.3500000000000003664 ) ;
#10134 = CARTESIAN_POINT ( 'NONE',  ( -22.19162232541316726, -74.22311029766915169, -32.68008730919952853 ) ) ;
#10135 = ORIENTED_EDGE ( 'NONE', *, *, #27228, .T. ) ;
#10136 = CARTESIAN_POINT ( 'NONE',  ( -15.12545007849999834, -101.1042191290000005, 4.523950879969999228 ) ) ;
#10137 = CARTESIAN_POINT ( 'NONE',  ( -15.12490670039999863, -101.0835132970000103, 3.210671277119999889 ) ) ;
#10138 = CARTESIAN_POINT ( 'NONE',  ( -32.38119801256480201, -74.06990842591031310, -22.11895758288902769 ) ) ;
#10139 = CARTESIAN_POINT ( 'NONE',  ( -21.43329106970000453, -64.24504445130001784, 15.59675033660000132 ) ) ;
#10140 = ORIENTED_EDGE ( 'NONE', *, *, #25606, .T. ) ;
#10141 = CARTESIAN_POINT ( 'NONE',  ( -40.00000000000000000, -79.00000000000000000, 0.000000000000000000 ) ) ;
#10142 = CARTESIAN_POINT ( 'NONE',  ( -2.433604254030000025, -18.85965710059999978, -22.72529456070000009 ) ) ;
#10143 = CARTESIAN_POINT ( 'NONE',  ( -7.367195939092531454, -101.3586211803017960, 14.45516488556769907 ) ) ;
#10144 = VERTEX_POINT ( 'NONE', #4821 ) ;
#10145 = EDGE_CURVE ( 'NONE', #6448, #7597, #13247, .T. ) ;
#10146 = EDGE_CURVE ( 'NONE', #21742, #10192, #27938, .T. ) ;
#10147 = LINE ( 'NONE', #27544, #26544 ) ;
#10148 = CARTESIAN_POINT ( 'NONE',  ( -41.91080735079999897, -65.74290444429999525, -1.043878813350000101 ) ) ;
#10149 = CARTESIAN_POINT ( 'NONE',  ( 36.70830968599999977, -79.18133521899999039, -14.75000000000000000 ) ) ;
#10150 = EDGE_LOOP ( 'NONE', ( #1130, #15266, #17117 ) ) ;
#10151 = EDGE_CURVE ( 'NONE', #14119, #3822, #28397, .T. ) ;
#10152 = AXIS2_PLACEMENT_3D ( 'NONE', #17292, #26032, #19465 ) ;
#10153 = AXIS2_PLACEMENT_3D ( 'NONE', #25340, #25037, #2753 ) ;
#10154 = CARTESIAN_POINT ( 'NONE',  ( 6.682768326704020545, -100.8061861241085353, 15.25838507520291287 ) ) ;
#10155 = CARTESIAN_POINT ( 'NONE',  ( -1.962472190547156492, -80.20444909203943951, 46.98144082036905900 ) ) ;
#10156 = ORIENTED_EDGE ( 'NONE', *, *, #6786, .T. ) ;
#10157 = CARTESIAN_POINT ( 'NONE',  ( 46.35917536702522312, -73.60349922462170014, -3.481876491973060705 ) ) ;
#10158 = EDGE_LOOP ( 'NONE', ( #11623, #13094, #17011, #5035, #1607 ) ) ;
#10159 = CARTESIAN_POINT ( 'NONE',  ( 23.14416696800000040, -57.40875702389999446, 10.37855829579999778 ) ) ;
#10160 = CARTESIAN_POINT ( 'NONE',  ( -6.003869784890000005, -101.1848541609999899, 14.05329173640000029 ) ) ;
#10161 = ORIENTED_EDGE ( 'NONE', *, *, #3341, .T. ) ;
#10162 = CARTESIAN_POINT ( 'NONE',  ( 13.69115815750000031, -100.1275643909999928, -9.470476298019999462 ) ) ;
#10163 = CARTESIAN_POINT ( 'NONE',  ( 22.97877291159999658, -37.99999999279999230, -9.393614097370001303 ) ) ;
#10164 = ADVANCED_FACE ( 'NONE', ( #19946 ), #14081, .T. ) ;
#10165 = AXIS2_PLACEMENT_3D ( 'NONE', #8404, #17025, #11832 ) ;
#10166 = CARTESIAN_POINT ( 'NONE',  ( 40.32207487400000190, -74.31847293620000983, 7.253641904880000268 ) ) ;
#10167 = CARTESIAN_POINT ( 'NONE',  ( 8.748807886850000770, -36.72219091139999847, -21.64960688639999731 ) ) ;
#10168 = CARTESIAN_POINT ( 'NONE',  ( 19.36781163719999910, -19.46510053389999939, 10.50580276810000058 ) ) ;
#10169 = CARTESIAN_POINT ( 'NONE',  ( 9.719900652158303345, -61.18767182266058313, -23.95297974322888024 ) ) ;
#10170 = VERTEX_POINT ( 'NONE', #20554 ) ;
#10171 = VECTOR ( 'NONE', #6723, 1000.000000000000114 ) ;
#10172 = AXIS2_PLACEMENT_3D ( 'NONE', #26983, #2507, #11210 ) ;
#10173 = DIRECTION ( 'NONE',  ( 1.000000000000000000, 0.000000000000000000, 0.000000000000000000 ) ) ;
#10174 = CARTESIAN_POINT ( 'NONE',  ( 11.67094368468833387, -93.01584921746606938, -23.70866539702249653 ) ) ;
#10175 = CARTESIAN_POINT ( 'NONE',  ( 24.17687301000000133, -92.98481302140000082, -11.27069079640000027 ) ) ;
#10176 = CARTESIAN_POINT ( 'NONE',  ( -2.566493094860000213, -53.78538132969999452, -24.83346198079999922 ) ) ;
#10177 = CIRCLE ( 'NONE', #20916, 0.4999999999999982236 ) ;
#10178 = CARTESIAN_POINT ( 'NONE',  ( 29.73294340391298007, -92.80442066025455006, 6.797243626917193637 ) ) ;
#10179 = DIRECTION ( 'NONE',  ( 0.4794255386042036715, 0.000000000000000000, 0.8775825618903724257 ) ) ;
#10180 = ORIENTED_EDGE ( 'NONE', *, *, #7540, .T. ) ;
#10181 = CARTESIAN_POINT ( 'NONE',  ( 9.718892398710000435, -91.50000000000000000, 28.91008700340000104 ) ) ;
#10182 = CARTESIAN_POINT ( 'NONE',  ( 25.02601311510000315, -11.00000000000000000, 45.80980973070000317 ) ) ;
#10183 = DIRECTION ( 'NONE',  ( 1.000000000000000000, 0.000000000000000000, 0.000000000000000000 ) ) ;
#10184 = B_SPLINE_CURVE_WITH_KNOTS ( 'NONE', 3,
 ( #5265, #1327, #20861, #920, #5120, #3367, #2945, #10169, #27271, #7308, #22907, #21001 ),
 .UNSPECIFIED., .F., .F.,
 ( 4, 2, 2, 2, 2, 4 ),
 ( 0.000000000000000000, 0.2500000000000004996, 0.3750000000000007772, 0.4375000000000008882, 0.5000000000000009992, 1.000000000000000000 ),
 .UNSPECIFIED. ) ;
#10185 = CARTESIAN_POINT ( 'NONE',  ( 31.74621573099999949, -73.74045749030000252, -21.89553964419999943 ) ) ;
#10186 = CARTESIAN_POINT ( 'NONE',  ( 20.30102379280000235, -72.00000000000000000, -30.97095677779999789 ) ) ;
#10187 = B_SPLINE_CURVE_WITH_KNOTS ( 'NONE', 3,
 ( #17708, #20026, #26594, #94, #17852, #26750, #4589, #13464, #11269, #249, #17995, #6930, #15793, #18876, #11715, #3424, #12289, #20777, #21062, #18440, #25144, #14623, #7671, #23243, #9824, #21198, #10091, #7368, #5741, #16670, #11866, #25434, #1121 ),
 .UNSPECIFIED., .F., .F.,
 ( 4, 2, 2, 1, 1, 1, 2, 2, 2, 1, 1, 1, 2, 2, 2, 1, 1, 1, 2, 2, 4 ),
 ( 0.000000000000000000, 0.1250000000005699607, 0.1875000000008528733, 0.2187500000009991175, 0.2343750000010775270, 0.2421875000011083912, 0.2460937500011094736, 0.2500000000011105561, 0.3750000000008985035, 0.4375000000007871481, 0.4687500000007259193, 0.4843750000006953327, 0.4921875000006845635, 0.5000000000006737944, 0.6250000000004710676, 0.6875000000003697043, 0.7187500000003232969, 0.7343750000002956524, 0.7421875000002818856, 0.7500000000002680078, 1.000000000000000000 ),
 .UNSPECIFIED. ) ;
#10188 =( LENGTH_UNIT ( ) NAMED_UNIT ( * ) SI_UNIT ( .MILLI., .METRE. ) );
#10189 = DIRECTION ( 'NONE',  ( 0.000000000000000000, -1.000000000000000000, 0.000000000000000000 ) ) ;
#10190 = CIRCLE ( 'NONE', #19979, 18.64285714289999873 ) ;
#10191 = AXIS2_PLACEMENT_3D ( 'NONE', #6320, #22066, #19857 ) ;
#10192 = VERTEX_POINT ( 'NONE', #13842 ) ;
#10193 = CARTESIAN_POINT ( 'NONE',  ( 8.677144177649999790, -37.95796631159999635, -21.92880660069999976 ) ) ;
#10194 = CARTESIAN_POINT ( 'NONE',  ( 21.23424077079999961, -35.30313508829999591, -7.936588796080000563 ) ) ;
#10195 = CARTESIAN_POINT ( 'NONE',  ( 21.41729796960000343, -36.56372031789999966, -7.953963089449999302 ) ) ;
#10196 = CARTESIAN_POINT ( 'NONE',  ( -21.60034894820000062, -79.50000026560000776, -32.77174736439999947 ) ) ;
#10197 = EDGE_LOOP ( 'NONE', ( #4455, #14921, #14855, #19599 ) ) ;
#10198 = CARTESIAN_POINT ( 'NONE',  ( -12.86092766119999986, -101.0535396030000044, -8.816187549039998572 ) ) ;
#10199 = ADVANCED_FACE ( 'NONE', ( #3220 ), #9753, .T. ) ;
#10200 = CARTESIAN_POINT ( 'NONE',  ( -17.06630915629999734, -92.84728946610000833, -23.47642349310000043 ) ) ;
#10201 = CARTESIAN_POINT ( 'NONE',  ( -1.229525073969999882, -101.0685839089999831, -16.04536366179999973 ) ) ;
#10202 = CARTESIAN_POINT ( 'NONE',  ( -4.794255386040000566, -107.5000000000000000, -8.775825618900000791 ) ) ;
#10203 = DIRECTION ( 'NONE',  ( 0.8091158474751271035, 0.000000000000000000, 0.5876491686070922649 ) ) ;
#10204 = CARTESIAN_POINT ( 'NONE',  ( 7.569553306790000491, -101.4254870009999934, 14.06091893229999990 ) ) ;
#10205 = VERTEX_POINT ( 'NONE', #7299 ) ;
#10206 = ADVANCED_FACE ( 'NONE', ( #12224 ), #18660, .F. ) ;
#10207 = CARTESIAN_POINT ( 'NONE',  ( 12.39757656149999931, -101.6484611540000031, -10.11435096289999969 ) ) ;
#10208 = CARTESIAN_POINT ( 'NONE',  ( -25.63355024200000187, -93.05538537040000335, -6.006632896850000236 ) ) ;
#10209 = CARTESIAN_POINT ( 'NONE',  ( 11.86656066179999947, -101.3150700380000018, -11.10431109579999820 ) ) ;
#10210 = ORIENTED_EDGE ( 'NONE', *, *, #27116, .T. ) ;
#10211 = CARTESIAN_POINT ( 'NONE',  ( -13.82310862920000005, -74.00000000000000000, 36.20061004769999613 ) ) ;
#10212 = ADVANCED_FACE ( 'NONE', ( #9468 ), #24774, .F. ) ;
#10213 = DIRECTION ( 'NONE',  ( 0.5000000000001884048, 0.000000000000000000, -0.8660254037843300168 ) ) ;
#10214 = CARTESIAN_POINT ( 'NONE',  ( -14.65665286289999969, -74.50000000000000000, 36.94583910070000599 ) ) ;
#10215 = CARTESIAN_POINT ( 'NONE',  ( -17.58183917889999748, -94.05395947819999947, 17.08481454950000256 ) ) ;
#10216 = DIRECTION ( 'NONE',  ( 0.000000000000000000, 1.000000000000000000, 0.000000000000000000 ) ) ;
#10217 = VERTEX_POINT ( 'NONE', #28519 ) ;
#10218 = ADVANCED_FACE ( 'NONE', ( #8001 ), #27109, .T. ) ;
#10219 = VECTOR ( 'NONE', #12990, 1000.000000000000000 ) ;
#10220 = DIRECTION ( 'NONE',  ( -1.000000000000000000, 0.000000000000000000, -7.486357007659997978E-17 ) ) ;
#10221 = CARTESIAN_POINT ( 'NONE',  ( -0.03691758196609999654, -101.3138676899999950, -15.91402604900000028 ) ) ;
#10222 = CARTESIAN_POINT ( 'NONE',  ( 9.613588401009998563, -61.68639133699999633, -23.70244304940000291 ) ) ;
#10223 = CARTESIAN_POINT ( 'NONE',  ( 15.64667777420000050, -100.8816835080000089, 2.154424203329999621 ) ) ;
#10224 = CARTESIAN_POINT ( 'NONE',  ( 22.56940943720000092, -57.43018231299999599, 10.15711860900000119 ) ) ;
#10225 = DIRECTION ( 'NONE',  ( -1.000000000000000000, 0.000000000000000000, 0.000000000000000000 ) ) ;
#10226 = ORIENTED_EDGE ( 'NONE', *, *, #7346, .T. ) ;
#10227 = CARTESIAN_POINT ( 'NONE',  ( 6.678590877449999574, -99.74726900420000675, 15.80215313019999890 ) ) ;
#10228 = CARTESIAN_POINT ( 'NONE',  ( -15.63967876733211249, -92.57787461316036115, -24.03209257557816514 ) ) ;
#10229 = CARTESIAN_POINT ( 'NONE',  ( -11.67413748739999946, -94.95684267580000437, -21.41802841999999885 ) ) ;
#10230 = DIRECTION ( 'NONE',  ( 0.000000000000000000, -1.000000000000000000, 0.000000000000000000 ) ) ;
#10231 = CARTESIAN_POINT ( 'NONE',  ( 5.011613449249795238, -92.66777315147957950, -30.08544135070622616 ) ) ;
#10232 = CARTESIAN_POINT ( 'NONE',  ( -7.302336599650000259, -98.93445099689999722, 17.20095762220000069 ) ) ;
#10233 = AXIS2_PLACEMENT_3D ( 'NONE', #13153, #10945, #17107 ) ;
#10234 = CARTESIAN_POINT ( 'NONE',  ( -28.07036528529999941, -39.50000000000000000, -51.38245899869999533 ) ) ;
#10235 = CARTESIAN_POINT ( 'NONE',  ( 9.011184001060000170, -94.54647010780000471, -23.25409275959999889 ) ) ;
#10236 = VECTOR ( 'NONE', #26727, 1000.000000000000000 ) ;
#10237 = CARTESIAN_POINT ( 'NONE',  ( 21.05852160050000066, -34.60505674910000096, -8.113043604739999637 ) ) ;
#10238 = ORIENTED_EDGE ( 'NONE', *, *, #19214, .T. ) ;
#10239 = LINE ( 'NONE', #24083, #2686 ) ;
#10240 = CARTESIAN_POINT ( 'NONE',  ( -5.854053644989999583, -101.0685849509999912, 14.98984533339999992 ) ) ;
#10241 = EDGE_LOOP ( 'NONE', ( #14140, #15157, #25095, #9167 ) ) ;
#10242 = ADVANCED_FACE ( 'NONE', ( #24296 ), #19912, .F. ) ;
#10243 = CARTESIAN_POINT ( 'NONE',  ( 7.215414233289999757, -74.50000000000000000, -40.70731707320000226 ) ) ;
#10244 = EDGE_CURVE ( 'NONE', #24813, #4093, #25868, .T. ) ;
#10245 = CARTESIAN_POINT ( 'NONE',  ( 0.5204107913287318032, -100.1517898586199493, -17.17286546631214961 ) ) ;
#10246 = CARTESIAN_POINT ( 'NONE',  ( 6.072376808220000477, -100.9137139110000021, 14.40534646189999890 ) ) ;
#10247 = CARTESIAN_POINT ( 'NONE',  ( -13.09441083470000144, -92.84549618469999643, -23.96915825600000005 ) ) ;
#10248 = DIRECTION ( 'NONE',  ( 1.000000000000000000, 0.000000000000000000, 0.000000000000000000 ) ) ;
#10249 = ADVANCED_FACE ( 'NONE', ( #20362 ), #13508, .T. ) ;
#10250 = CARTESIAN_POINT ( 'NONE',  ( 26.48637309549999941, -74.30622060240000337, -29.02318743760000075 ) ) ;
#10251 = ADVANCED_FACE ( 'NONE', ( #18181 ), #27669, .T. ) ;
#10252 = CARTESIAN_POINT ( 'NONE',  ( -26.77683864449999973, -26.59999999999999787, -49.01467436490000296 ) ) ;
#10253 = DIRECTION ( 'NONE',  ( 0.000000000000000000, -1.000000000000000000, 0.000000000000000000 ) ) ;
#10254 = FACE_OUTER_BOUND ( 'NONE', #20944, .T. ) ;
#10255 = CARTESIAN_POINT ( 'NONE',  ( 24.33664649176833095, -93.98969193921543308, -9.464842905525378214 ) ) ;
#10256 = AXIS2_PLACEMENT_3D ( 'NONE', #18011, #26909, #6950 ) ;
#10257 = VERTEX_POINT ( 'NONE', #24890 ) ;
#10258 = AXIS2_PLACEMENT_3D ( 'NONE', #26369, #17628, #21999 ) ;
#10259 = CARTESIAN_POINT ( 'NONE',  ( -41.14961768690000099, -65.31510159580000163, 2.684458023169999930 ) ) ;
#10260 = CIRCLE ( 'NONE', #4704, 34.89999999999999858 ) ;
#10261 = B_SPLINE_CURVE_WITH_KNOTS ( 'NONE', 3,
 ( #20596, #17821, #11389, #4705, #18116, #2232 ),
 .UNSPECIFIED., .F., .F.,
 ( 4, 2, 4 ),
 ( 0.000000000000000000, 0.5000000000000002220, 1.000000000000000000 ),
 .UNSPECIFIED. ) ;
#10262 = EDGE_LOOP ( 'NONE', ( #11078, #11466, #12908, #2782 ) ) ;
#10263 = CARTESIAN_POINT ( 'NONE',  ( -0.9108550417630000284, -62.96338283689998860, -24.26276433549999823 ) ) ;
#10264 = CARTESIAN_POINT ( 'NONE',  ( -29.66597372489999884, -92.76843000840000286, 6.359924916739999823 ) ) ;
#10265 = CARTESIAN_POINT ( 'NONE',  ( 20.95510892579999762, -35.33620225780000368, -8.408939989400000314 ) ) ;
#10266 = ORIENTED_EDGE ( 'NONE', *, *, #2149, .F. ) ;
#10267 = CARTESIAN_POINT ( 'NONE',  ( 21.43354447929999651, -35.82074273779999629, -7.316573576590000627 ) ) ;
#10268 = ORIENTED_EDGE ( 'NONE', *, *, #4741, .F. ) ;
#10269 = AXIS2_PLACEMENT_3D ( 'NONE', #11990, #16946, #7783 ) ;
#10270 = CARTESIAN_POINT ( 'NONE',  ( 7.635730262653531497, -37.29149436589506195, -21.50724729230068988 ) ) ;
#10271 = CIRCLE ( 'NONE', #6574, 2.500000000000000444 ) ;
#10272 = ORIENTED_EDGE ( 'NONE', *, *, #18902, .F. ) ;
#10273 = EDGE_CURVE ( 'NONE', #28503, #22334, #6074, .T. ) ;
#10274 = AXIS2_PLACEMENT_3D ( 'NONE', #11347, #13091, #22288 ) ;
#10275 = CARTESIAN_POINT ( 'NONE',  ( -14.66608889819999995, -79.71516998469999749, 36.47374630150000030 ) ) ;
#10276 = CARTESIAN_POINT ( 'NONE',  ( 10.20110288159999890, -84.00000000000000000, 41.00000000000000000 ) ) ;
#10277 = EDGE_CURVE ( 'NONE', #14992, #14960, #9861, .T. ) ;
#10278 = FACE_OUTER_BOUND ( 'NONE', #26904, .T. ) ;
#10279 = CARTESIAN_POINT ( 'NONE',  ( -15.48764535020000110, -101.3256027289999963, 3.628077442809999997 ) ) ;
#10280 = CARTESIAN_POINT ( 'NONE',  ( -32.82503636037260719, -74.41293640438078683, -22.22642620204530672 ) ) ;
#10281 = CARTESIAN_POINT ( 'NONE',  ( -17.59440688584024315, -95.56535007417228655, 14.09092167176237531 ) ) ;
#10282 = VERTEX_POINT ( 'NONE', #9427 ) ;
#10283 = CARTESIAN_POINT ( 'NONE',  ( -47.25000000000000000, -69.50000000000000000, 3.352534721190000231E-15 ) ) ;
#10284 = CARTESIAN_POINT ( 'NONE',  ( -12.36549121539999874, -100.9678331089999972, -10.43708019790000030 ) ) ;
#10285 = CARTESIAN_POINT ( 'NONE',  ( -2.591557398349999985, -19.17414499179999865, -23.45736093650000242 ) ) ;
#10286 = CARTESIAN_POINT ( 'NONE',  ( -7.787505644985010633, -100.7538407668029379, 14.77225502553302583 ) ) ;
#10287 = VERTEX_POINT ( 'NONE', #25187 ) ;
#10288 = CARTESIAN_POINT ( 'NONE',  ( -4.500000000000000000, -15.00000000000000000, 31.00000000000000000 ) ) ;
#10289 = CARTESIAN_POINT ( 'NONE',  ( -31.99425276130000384, -74.00000000020000357, -21.99785695679999975 ) ) ;
#10290 = CARTESIAN_POINT ( 'NONE',  ( 7.196178079599999222, -73.81415926540000783, 38.70548889989999708 ) ) ;
#10291 = ORIENTED_EDGE ( 'NONE', *, *, #25646, .T. ) ;
#10292 = TOROIDAL_SURFACE ( 'NONE', #25237, 5.500000000000000000, 0.5000000000000000000 ) ;
#10293 = AXIS2_PLACEMENT_3D ( 'NONE', #24325, #2044, #26964 ) ;
#10294 = CARTESIAN_POINT ( 'NONE',  ( 40.00000000000000000, -73.50000000000000000, 2.065014825799999939E-15 ) ) ;
#10295 = CARTESIAN_POINT ( 'NONE',  ( -2.570879204283450736, -80.36838817132422719, 46.77903939411709189 ) ) ;
#10296 = VERTEX_POINT ( 'NONE', #20512 ) ;
#10297 = CARTESIAN_POINT ( 'NONE',  ( 27.18988201479999844, -23.90155444570000043, 49.77074518290000071 ) ) ;
#10298 = VERTEX_POINT ( 'NONE', #582 ) ;
#10299 = CARTESIAN_POINT ( 'NONE',  ( 27.11204721459999689, -92.54030572580001035, 9.444959058340000269 ) ) ;
#10300 = CARTESIAN_POINT ( 'NONE',  ( -38.48683073767716678, -63.06504043304416030, 2.884616214735281847 ) ) ;
#10301 = CARTESIAN_POINT ( 'NONE',  ( -7.260205543919999727, -73.74944613220000633, -39.69269201139999836 ) ) ;
#10302 = ORIENTED_EDGE ( 'NONE', *, *, #26155, .T. ) ;
#10303 = CARTESIAN_POINT ( 'NONE',  ( -3.219077971254640236, -97.43430234703029669, -20.31490937506839600 ) ) ;
#10304 = DIRECTION ( 'NONE',  ( 0.000000000000000000, -1.000000000000000000, 0.000000000000000000 ) ) ;
#10305 = EDGE_CURVE ( 'NONE', #10296, #23041, #3183, .T. ) ;
#10306 = CARTESIAN_POINT ( 'NONE',  ( -42.84278392979705785, -63.17171877515596634, 0.3794438750353775203 ) ) ;
#10307 = CARTESIAN_POINT ( 'NONE',  ( 7.629218925470000023, -101.5342894280000081, 14.06592359269999903 ) ) ;
#10308 = AXIS2_PLACEMENT_3D ( 'NONE', #26891, #2708, #7222 ) ;
#10309 = DIRECTION ( 'NONE',  ( 0.000000000000000000, 1.000000000000000000, 0.000000000000000000 ) ) ;
#10310 = ORIENTED_EDGE ( 'NONE', *, *, #5965, .F. ) ;
#10311 = CARTESIAN_POINT ( 'NONE',  ( -15.04902548439999954, -98.73889367950000917, -10.99609012540000030 ) ) ;
#10312 = CARTESIAN_POINT ( 'NONE',  ( 19.97576656849999921, -35.50000000000000000, -19.97576656849999921 ) ) ;
#10313 = CARTESIAN_POINT ( 'NONE',  ( -20.52074439609999956, -93.75380055729999640, 14.17856059480000042 ) ) ;
#10314 = CARTESIAN_POINT ( 'NONE',  ( 24.04401824170000168, -94.24983875559999547, -8.202559790829997866 ) ) ;
#10315 = CARTESIAN_POINT ( 'NONE',  ( -0.5367793161509999411, -55.05574748869999979, -23.27036471170000098 ) ) ;
#10316 = CARTESIAN_POINT ( 'NONE',  ( 26.60903970598167589, -30.20000000000000284, 48.70752046822583736 ) ) ;
#10317 = DIRECTION ( 'NONE',  ( 0.000000000000000000, 1.000000000000000000, 0.000000000000000000 ) ) ;
#10318 = ORIENTED_EDGE ( 'NONE', *, *, #2888, .F. ) ;
#10319 = DIRECTION ( 'NONE',  ( 1.000000000000000000, 0.000000000000000000, 1.278217298088173493E-15 ) ) ;
#10320 = CARTESIAN_POINT ( 'NONE',  ( -18.51518804340000202, -19.44981017040000282, 13.21263506969999924 ) ) ;
#10321 = DIRECTION ( 'NONE',  ( 0.4794255386042041156, 0.000000000000000000, 0.8775825618903719816 ) ) ;
#10322 = CARTESIAN_POINT ( 'NONE',  ( 8.125022609680000230, -36.17810633829999745, -21.26282345639999605 ) ) ;
#10323 = APPLICATION_CONTEXT ( 'automotive_design' ) ;
#10324 = CARTESIAN_POINT ( 'NONE',  ( 22.05228288849999885, -72.00360875399999827, -30.91980140109999553 ) ) ;
#10325 = EDGE_CURVE ( 'NONE', #16095, #14660, #24841, .T. ) ;
#10326 = AXIS2_PLACEMENT_3D ( 'NONE', #13086, #9741, #7284 ) ;
#10327 = CIRCLE ( 'NONE', #21109, 4.750000000000000888 ) ;
#10328 = ORIENTED_EDGE ( 'NONE', *, *, #3414, .T. ) ;
#10329 = CARTESIAN_POINT ( 'NONE',  ( 21.45633488809999889, -36.07487150869999937, -7.289748192099999358 ) ) ;
#10330 = ORIENTED_EDGE ( 'NONE', *, *, #8956, .T. ) ;
#10331 = CARTESIAN_POINT ( 'NONE',  ( 21.29631346280000059, -36.39568407349999291, -8.188957909990000061 ) ) ;
#10332 = CARTESIAN_POINT ( 'NONE',  ( -9.708956880459998828, -80.00000000000000000, 43.08928339610000791 ) ) ;
#10333 = VERTEX_POINT ( 'NONE', #7120 ) ;
#10334 = CARTESIAN_POINT ( 'NONE',  ( 9.279094190520000396, -98.48918237500001283, 16.48187022329999962 ) ) ;
#10335 = EDGE_CURVE ( 'NONE', #22088, #21458, #2605, .T. ) ;
#10336 = B_SPLINE_SURFACE_WITH_KNOTS ( 'NONE', 5, 5, ( 
 ( #25241, #12367, #23596, #3640, #10038, #18678 ),
 ( #12501, #21413, #27418, #7471, #23055, #3099 ),
 ( #924, #25653, #5683, #11952, #9766, #16480 ),
 ( #25382, #3237, #12094, #22368, #685, #27036 ),
 ( #7079, #22811, #18137, #22662, #7366, #9387 ),
 ( #18438, #9535, #11713, #24987, #386, #2854 ) ),
 .UNSPECIFIED., .F., .F., .F.,
 ( 6, 6 ),
 ( 6, 6 ),
 ( 15.82767921900000019, 30.79602961229999991 ),
 ( 0.000000000000000000, 0.5000000000000000000 ),
 .UNSPECIFIED. ) ;
#10337 = CARTESIAN_POINT ( 'NONE',  ( -14.13789956389999958, -93.18831369829999289, -23.64158520889999693 ) ) ;
#10338 = DIRECTION ( 'NONE',  ( 0.000000000000000000, -1.000000000000000000, 0.000000000000000000 ) ) ;
#10339 = ORIENTED_EDGE ( 'NONE', *, *, #9401, .T. ) ;
#10340 = CARTESIAN_POINT ( 'NONE',  ( 1.810422456229999977, -92.75885938639999040, 27.42763845990000249 ) ) ;
#10341 = AXIS2_PLACEMENT_3D ( 'NONE', #21847, #11182, #4505 ) ;
#10342 = CARTESIAN_POINT ( 'NONE',  ( 9.099149309629998683, -57.44066854489999940, -22.71963733680000175 ) ) ;
#10343 = CYLINDRICAL_SURFACE ( 'NONE', #28324, 57.74999999999999289 ) ;
#10344 = ORIENTED_EDGE ( 'NONE', *, *, #7719, .F. ) ;
#10345 = CYLINDRICAL_SURFACE ( 'NONE', #16734, 7.250000000000004441 ) ;
#10346 = CARTESIAN_POINT ( 'NONE',  ( -27.14282719570000069, -92.75885938639999040, -4.338192340750000042 ) ) ;
#10347 = CARTESIAN_POINT ( 'NONE',  ( -13.00193227667292639, -19.48498969582177409, 19.66058068040372575 ) ) ;
#10348 = CARTESIAN_POINT ( 'NONE',  ( 39.29494613547247894, -73.61009970497249810, 7.215638845165015525 ) ) ;
#10349 = ORIENTED_EDGE ( 'NONE', *, *, #22654, .T. ) ;
#10350 = CARTESIAN_POINT ( 'NONE',  ( 20.19515389160000396, -19.16582656490000147, -8.522375633559999386 ) ) ;
#10351 = CIRCLE ( 'NONE', #3844, 55.67692378859999991 ) ;
#10352 = AXIS2_PLACEMENT_3D ( 'NONE', #16790, #10066, #10203 ) ;
#10353 = CARTESIAN_POINT ( 'NONE',  ( -14.12253468279999957, -74.03309514170000227, 36.41043208560000011 ) ) ;
#10354 = DIRECTION ( 'NONE',  ( 0.9295286103719527793, 0.000000000000000000, 0.3687499999999814260 ) ) ;
#10355 = DIRECTION ( 'NONE',  ( 0.000000000000000000, 1.000000000000000000, 0.000000000000000000 ) ) ;
#10356 = ORIENTED_EDGE ( 'NONE', *, *, #10273, .T. ) ;
#10357 = CARTESIAN_POINT ( 'NONE',  ( 40.00000000000000000, -73.50000000000000000, 2.065014825799999939E-15 ) ) ;
#10358 = CARTESIAN_POINT ( 'NONE',  ( -0.1689899845689999958, -101.2530993010000060, -15.19297360289999865 ) ) ;
#10359 = CARTESIAN_POINT ( 'NONE',  ( 8.286111488879999598, -65.02206714839999790, -23.78780924429999999 ) ) ;
#10360 = CARTESIAN_POINT ( 'NONE',  ( 7.370697001239634005, -73.94611239985914608, -38.67409491847346459 ) ) ;
#10361 = CARTESIAN_POINT ( 'NONE',  ( 7.670973119660000172, -34.59820496239999699, -21.21808926809999818 ) ) ;
#10362 = CARTESIAN_POINT ( 'NONE',  ( 5.326862811529999898E-15, -77.00000000000000000, -47.25000000000000000 ) ) ;
#10363 = ORIENTED_EDGE ( 'NONE', *, *, #4446, .F. ) ;
#10364 = EDGE_CURVE ( 'NONE', #10257, #2641, #3051, .T. ) ;
#10365 = CARTESIAN_POINT ( 'NONE',  ( 6.266701257130000258, -100.8685038539999965, 14.42968300090000078 ) ) ;
#10366 = CARTESIAN_POINT ( 'NONE',  ( 15.37132493649999887, -101.0678230150000019, 3.755183840060000389 ) ) ;
#10367 = AXIS2_PLACEMENT_3D ( 'NONE', #10662, #11252, #17833 ) ;
#10368 = CARTESIAN_POINT ( 'NONE',  ( -40.46255798985529140, -65.65254685978855775, -2.287783922119399183 ) ) ;
#10369 = CARTESIAN_POINT ( 'NONE',  ( 25.02601311510000315, -6.000000000000000000, 45.80980973070000317 ) ) ;
#10370 = EDGE_CURVE ( 'NONE', #54, #16026, #11903, .T. ) ;
#10371 = CARTESIAN_POINT ( 'NONE',  ( 25.33393120808624843, -93.66270333200125719, -5.817803472910904716 ) ) ;
#10372 = ORIENTED_EDGE ( 'NONE', *, *, #6852, .F. ) ;
#10373 = TOROIDAL_SURFACE ( 'NONE', #8989, 21.14285714289999873, 0.5000000000000000000 ) ;
#10374 = CARTESIAN_POINT ( 'NONE',  ( 3.220763788040000186, -92.54807930229999613, -28.60785095109999787 ) ) ;
#10375 = CARTESIAN_POINT ( 'NONE',  ( -7.135467526410000261, -73.50000000000000000, -38.71641004229999794 ) ) ;
#10376 = CARTESIAN_POINT ( 'NONE',  ( -3.215510237749999778, -94.59276292389999696, 23.57860181210000405 ) ) ;
#10377 = ORIENTED_EDGE ( 'NONE', *, *, #11307, .F. ) ;
#10378 = CARTESIAN_POINT ( 'NONE',  ( 0.000000000000000000, -21.50000000000000000, 0.000000000000000000 ) ) ;
#10379 = CARTESIAN_POINT ( 'NONE',  ( 19.97576656849999921, -55.50000000000000000, -19.97576656849999921 ) ) ;
#10380 = ORIENTED_EDGE ( 'NONE', *, *, #20788, .F. ) ;
#10381 = ORIENTED_EDGE ( 'NONE', *, *, #27519, .F. ) ;
#10382 = CARTESIAN_POINT ( 'NONE',  ( 11.74592569580000045, -14.00000000000000000, 21.50077276629999901 ) ) ;
#10383 = TOROIDAL_SURFACE ( 'NONE', #21138, 18.14285714289999873, 0.5000000000000000000 ) ;
#10384 = DIRECTION ( 'NONE',  ( 1.000000000000000000, 0.000000000000000000, 0.000000000000000000 ) ) ;
#10385 = CIRCLE ( 'NONE', #26677, 2.000000000000000888 ) ;
#10386 = CARTESIAN_POINT ( 'NONE',  ( 13.22388793010019548, -92.80442066019948300, 27.48416330172907607 ) ) ;
#10387 = DIRECTION ( 'NONE',  ( 0.000000000000000000, 1.000000000000000000, 0.000000000000000000 ) ) ;
#10388 = FACE_OUTER_BOUND ( 'NONE', #17932, .T. ) ;
#10389 = CARTESIAN_POINT ( 'NONE',  ( -23.11870653469999937, -72.31449597569999810, 16.58129546599999671 ) ) ;
#10390 = DIRECTION ( 'NONE',  ( 0.000000000000000000, 1.000000000000000000, 0.000000000000000000 ) ) ;
#10391 = CARTESIAN_POINT ( 'NONE',  ( -12.03627366839999802, -92.50000000000000000, 28.02459841239999960 ) ) ;
#10392 = AXIS2_PLACEMENT_3D ( 'NONE', #20496, #17878, #2734 ) ;
#10393 = CARTESIAN_POINT ( 'NONE',  ( 6.929578963970000061, -35.67530021650000549, -21.51138254459999999 ) ) ;
#10394 = FACE_OUTER_BOUND ( 'NONE', #9530, .T. ) ;
#10395 = ORIENTED_EDGE ( 'NONE', *, *, #15649, .T. ) ;
#10396 = ORIENTED_EDGE ( 'NONE', *, *, #6006, .T. ) ;
#10397 = CARTESIAN_POINT ( 'NONE',  ( 22.60430443959999991, -36.06167118559999807, -10.71318590909999990 ) ) ;
#10398 = ADVANCED_FACE ( 'NONE', ( #16427 ), #13832, .F. ) ;
#10399 = EDGE_CURVE ( 'NONE', #212, #23252, #2851, .T. ) ;
#10400 = CIRCLE ( 'NONE', #16948, 0.5000000000000013323 ) ;
#10401 = CARTESIAN_POINT ( 'NONE',  ( -0.5436438173659999817, -58.35721741809999941, -23.39762436370000032 ) ) ;
#10402 = CIRCLE ( 'NONE', #26729, 0.5000000000000004441 ) ;
#10403 = CARTESIAN_POINT ( 'NONE',  ( 9.691266666139998875, -36.53611442790000297, -22.20987735279999953 ) ) ;
#10404 = EDGE_CURVE ( 'NONE', #12727, #27727, #8398, .T. ) ;
#10405 = CARTESIAN_POINT ( 'NONE',  ( -29.37337778839999913, -92.51542729400000553, 6.408755614549999535 ) ) ;
#10406 = CARTESIAN_POINT ( 'NONE',  ( 8.920183199378271865, -94.54719627018464223, -22.12534656354277374 ) ) ;
#10407 = EDGE_CURVE ( 'NONE', #7623, #13967, #507, .T. ) ;
#10408 = ORIENTED_EDGE ( 'NONE', *, *, #3378, .F. ) ;
#10409 = CARTESIAN_POINT ( 'NONE',  ( 21.30237673919999608, -35.02344231349999859, -7.506539989010000191 ) ) ;
#10410 = DIRECTION ( 'NONE',  ( 0.000000000000000000, 1.000000000000000000, 0.000000000000000000 ) ) ;
#10411 = ORIENTED_EDGE ( 'NONE', *, *, #2988, .F. ) ;
#10412 = AXIS2_PLACEMENT_3D ( 'NONE', #678, #2999, #23098 ) ;
#10413 = DIRECTION ( 'NONE',  ( 0.2730005759809499555, 0.000000000000000000, -0.9620138697098237213 ) ) ;
#10414 = CARTESIAN_POINT ( 'NONE',  ( -22.13750278361801449, -74.09775395658994057, -32.45700471235915785 ) ) ;
#10415 = CARTESIAN_POINT ( 'NONE',  ( 21.77543175429999778, -18.50000000000000000, 8.809926792680000673 ) ) ;
#10416 = CARTESIAN_POINT ( 'NONE',  ( -32.50515439522262540, -74.11794838461926815, -22.14922053471763164 ) ) ;
#10417 = CARTESIAN_POINT ( 'NONE',  ( -20.33633474980000244, -58.84825201809999839, 14.70359657240000040 ) ) ;
#10418 = ORIENTED_EDGE ( 'NONE', *, *, #20815, .T. ) ;
#10419 = CIRCLE ( 'NONE', #20207, 8.099999999999999645 ) ;
#10420 = CARTESIAN_POINT ( 'NONE',  ( 23.54313657600000198, -94.98812477599999227, -6.784142512209999865 ) ) ;
#10421 = CARTESIAN_POINT ( 'NONE',  ( -11.97505089750000096, -101.1848541609999899, -9.495040346209998816 ) ) ;
#10422 = CARTESIAN_POINT ( 'NONE',  ( -0.5856137342820000313, -19.46510053389999939, -22.02591827759999887 ) ) ;
#10423 = CARTESIAN_POINT ( 'NONE',  ( -7.693802629154737005, -100.9364580240060292, 14.65842723137789960 ) ) ;
#10424 = ORIENTED_EDGE ( 'NONE', *, *, #15323, .T. ) ;
#10425 = CARTESIAN_POINT ( 'NONE',  ( 10.08508256729999886, -64.24504434620000382, -24.78974309399999854 ) ) ;
#10426 = DIRECTION ( 'NONE',  ( 1.000000000000000000, 0.000000000000000000, 0.000000000000000000 ) ) ;
#10427 = VERTEX_POINT ( 'NONE', #17269 ) ;
#10428 = ADVANCED_FACE ( 'NONE', ( #6631 ), #3327, .F. ) ;
#10429 = AXIS2_PLACEMENT_3D ( 'NONE', #505, #13874, #5140 ) ;
#10430 = LINE ( 'NONE', #14816, #27821 ) ;
#10431 = EDGE_CURVE ( 'NONE', #15079, #7826, #19607, .T. ) ;
#10432 = ORIENTED_EDGE ( 'NONE', *, *, #12108, .F. ) ;
#10433 = CARTESIAN_POINT ( 'NONE',  ( -12.79457676069784178, -70.02558174159734961, -24.23940011715129472 ) ) ;
#10434 = FACE_OUTER_BOUND ( 'NONE', #13555, .T. ) ;
#10435 = ORIENTED_EDGE ( 'NONE', *, *, #1951, .F. ) ;
#10436 = VECTOR ( 'NONE', #674, 1000.000000000000000 ) ;
#10437 = CARTESIAN_POINT ( 'NONE',  ( 29.52540672639999997, -93.00000902169999506, 7.168157281560000982 ) ) ;
#10438 = CARTESIAN_POINT ( 'NONE',  ( 15.50925563669999896, -100.9197081840000010, 1.894558565230000102 ) ) ;
#10439 = CARTESIAN_POINT ( 'NONE',  ( -7.283536107469999799, -74.14144860030000928, -39.92836808239999868 ) ) ;
#10440 = ORIENTED_EDGE ( 'NONE', *, *, #24381, .F. ) ;
#10441 = FACE_OUTER_BOUND ( 'NONE', #11443, .T. ) ;
#10442 = CARTESIAN_POINT ( 'NONE',  ( 19.53732555980000285, -35.60472305269999538, -8.991793591719998702 ) ) ;
#10443 = DIRECTION ( 'NONE',  ( 1.000000000000000000, 0.000000000000000000, 0.000000000000000000 ) ) ;
#10444 = CARTESIAN_POINT ( 'NONE',  ( 4.314829847440000421, -16.50000000000000000, 7.898243057010000179 ) ) ;
#10445 = ORIENTED_EDGE ( 'NONE', *, *, #20364, .F. ) ;
#10446 = CARTESIAN_POINT ( 'NONE',  ( -22.24124375720000302, -94.63960162979999780, -8.291374127620001033 ) ) ;
#10447 = CARTESIAN_POINT ( 'NONE',  ( 11.97048044210000128, -101.2358105800000061, -9.395351924210000760 ) ) ;
#10448 = CARTESIAN_POINT ( 'NONE',  ( -19.74785546080000032, -92.58502690130001156, 20.72667931229999994 ) ) ;
#10449 = CARTESIAN_POINT ( 'NONE',  ( 24.43035140000000283, -92.76004107139999633, -17.00416254499999980 ) ) ;
#10450 = ORIENTED_EDGE ( 'NONE', *, *, #3412, .F. ) ;
#10451 = CIRCLE ( 'NONE', #27730, 4.750000000000000000 ) ;
#10452 = CARTESIAN_POINT ( 'NONE',  ( 10.66842981584318295, -72.57936627267046958, -26.81288472990357263 ) ) ;
#10453 = FACE_BOUND ( 'NONE', #11195, .T. ) ;
#10454 = VERTEX_POINT ( 'NONE', #384 ) ;
#10455 = CARTESIAN_POINT ( 'NONE',  ( 21.83355004490000084, -37.95349900880000149, -8.543356255189999970 ) ) ;
#10456 = DIRECTION ( 'NONE',  ( 0.000000000000000000, 1.000000000000000000, 0.000000000000000000 ) ) ;
#10457 = CARTESIAN_POINT ( 'NONE',  ( 20.53702927206556339, -97.42330310008513550, 1.367348661909628227 ) ) ;
#10458 = CARTESIAN_POINT ( 'NONE',  ( 19.97576656849999921, -38.00000000000000000, -19.97576656849999921 ) ) ;
#10459 = CARTESIAN_POINT ( 'NONE',  ( -14.42431928191101953, -74.07810314560701670, 36.25543878699895828 ) ) ;
#10460 = DIRECTION ( 'NONE',  ( 0.000000000000000000, -1.000000000000000000, 0.000000000000000000 ) ) ;
#10461 = ADVANCED_FACE ( 'NONE', ( #20626 ), #22684, .T. ) ;
#10462 = EDGE_CURVE ( 'NONE', #9315, #11556, #12985, .T. ) ;
#10463 = ORIENTED_EDGE ( 'NONE', *, *, #13273, .T. ) ;
#10464 = PLANE ( 'NONE',  #22885 ) ;
#10465 = CARTESIAN_POINT ( 'NONE',  ( -40.27753662873140428, -74.17170883818889138, -7.244686332484143065 ) ) ;
#10466 = VERTEX_POINT ( 'NONE', #21610 ) ;
#10467 = B_SPLINE_CURVE_WITH_KNOTS ( 'NONE', 3,
 ( #23316, #7303, #25079, #20715 ),
 .UNSPECIFIED., .F., .F.,
 ( 4, 4 ),
 ( 0.000000000000000000, 1.000000000000000000 ),
 .UNSPECIFIED. ) ;
#10468 = CARTESIAN_POINT ( 'NONE',  ( 19.54920062769999944, -35.79804965070000122, -9.079275989799999280 ) ) ;
#10469 = CARTESIAN_POINT ( 'NONE',  ( -8.467380000549999508, -74.00000000000000000, 37.95957158089999695 ) ) ;
#10470 = ORIENTED_EDGE ( 'NONE', *, *, #23651, .F. ) ;
#10471 = FACE_OUTER_BOUND ( 'NONE', #21119, .T. ) ;
#10472 = DIRECTION ( 'NONE',  ( -0.8775825618903722036, 0.000000000000000000, 0.4794255386042041156 ) ) ;
#10473 = CARTESIAN_POINT ( 'NONE',  ( -14.09262705500000123, -92.79515029379999191, -23.78749435689999814 ) ) ;
#10474 = VERTEX_POINT ( 'NONE', #28296 ) ;
#10475 = CARTESIAN_POINT ( 'NONE',  ( -1.604075271319999940, -100.9197075889999979, -15.54198525189999813 ) ) ;
#10476 = DIRECTION ( 'NONE',  ( 0.000000000000000000, -1.000000000000000000, 0.000000000000000000 ) ) ;
#10477 = VECTOR ( 'NONE', #14014, 1000.000000000000000 ) ;
#10478 = DIRECTION ( 'NONE',  ( 0.000000000000000000, 1.000000000000000000, 0.000000000000000000 ) ) ;
#10479 = VERTEX_POINT ( 'NONE', #16051 ) ;
#10480 = CARTESIAN_POINT ( 'NONE',  ( 13.29192986090826878, -100.9364580246202081, -9.868570734956325197 ) ) ;
#10481 = EDGE_CURVE ( 'NONE', #20846, #27931, #5173, .T. ) ;
#10482 = CARTESIAN_POINT ( 'NONE',  ( 25.14017297600000234, -49.80573906499999737, 1.377424475129999992 ) ) ;
#10483 = CARTESIAN_POINT ( 'NONE',  ( 23.93286062550000182, -64.98911155900000836, 10.71582475930000022 ) ) ;
#10484 = DIRECTION ( 'NONE',  ( -0.8775825618903722036, 0.000000000000000000, 0.4794255386042041156 ) ) ;
#10485 = ORIENTED_EDGE ( 'NONE', *, *, #12273, .T. ) ;
#10486 = DIRECTION ( 'NONE',  ( 1.000000000000000000, 0.000000000000000000, 0.000000000000000000 ) ) ;
#10487 = CARTESIAN_POINT ( 'NONE',  ( -14.20005211740000028, -74.02367878169998505, 36.23549608150000267 ) ) ;
#10488 = CARTESIAN_POINT ( 'NONE',  ( -17.83719336599999750, -93.71758747490000019, 18.24690405790000014 ) ) ;
#10489 = CARTESIAN_POINT ( 'NONE',  ( 0.3059185938709999553, -93.00000000000000000, 14.72672055670000013 ) ) ;
#10490 = ORIENTED_EDGE ( 'NONE', *, *, #962, .F. ) ;
#10491 = CARTESIAN_POINT ( 'NONE',  ( -0.8996493333321277097, -74.26935822088371708, 47.19463505169927231 ) ) ;
#10492 = CARTESIAN_POINT ( 'NONE',  ( -0.1779554536940000098, -101.5369810359999860, -15.99901033990000165 ) ) ;
#10493 = CARTESIAN_POINT ( 'NONE',  ( 27.23269985219999967, -92.50000000000000000, -12.38957130830000075 ) ) ;
#10494 = CARTESIAN_POINT ( 'NONE',  ( -13.18221367349999973, -68.65989719860000662, -23.31533323539999714 ) ) ;
#10495 = CARTESIAN_POINT ( 'NONE',  ( 20.84247163680000270, -57.47571004099999925, 10.69856784059999910 ) ) ;
#10496 = DIRECTION ( 'NONE',  ( -0.3687499999999814260, 0.000000000000000000, 0.9295286103719527793 ) ) ;
#10497 = ORIENTED_EDGE ( 'NONE', *, *, #19239, .F. ) ;
#10498 = ADVANCED_FACE ( 'NONE', ( #24812, #8899 ), #7038, .T. ) ;
#10499 = ADVANCED_FACE ( 'NONE', ( #9194 ), #4213, .F. ) ;
#10500 = CARTESIAN_POINT ( 'NONE',  ( 6.523512041040000042, -100.2511768809999921, 15.35682148189999907 ) ) ;
#10501 = CARTESIAN_POINT ( 'NONE',  ( 15.01705834989999921, -101.1411470200000053, 3.365801592560000000 ) ) ;
#10502 = CARTESIAN_POINT ( 'NONE',  ( -32.70900267797851058, -74.50000000069999828, -21.69554430468080142 ) ) ;
#10503 = CYLINDRICAL_SURFACE ( 'NONE', #12204, 3.749999999999996447 ) ;
#10504 = FACE_OUTER_BOUND ( 'NONE', #7458, .T. ) ;
#10505 = VERTEX_POINT ( 'NONE', #20431 ) ;
#10506 = CARTESIAN_POINT ( 'NONE',  ( 8.149626591600000580, -93.87552273900000444, -23.44626940270000048 ) ) ;
#10507 = DIRECTION ( 'NONE',  ( 1.000000000000000000, 0.000000000000000000, 0.000000000000000000 ) ) ;
#10508 = LINE ( 'NONE', #1952, #1879 ) ;
#10509 = CARTESIAN_POINT ( 'NONE',  ( 6.019093083229999586, -92.50000000000000000, 29.30685818879999971 ) ) ;
#10510 = ORIENTED_EDGE ( 'NONE', *, *, #2045, .F. ) ;
#10511 = CARTESIAN_POINT ( 'NONE',  ( -11.90026993885546602, -42.27314267039926676, -19.48333362464491003 ) ) ;
#10512 = CARTESIAN_POINT ( 'NONE',  ( -12.49059627124878347, -101.1742791177312597, -10.57827074192917571 ) ) ;
#10513 = VERTEX_POINT ( 'NONE', #6595 ) ;
#10514 = EDGE_LOOP ( 'NONE', ( #26525, #5552, #28646, #17454 ) ) ;
#10515 = CARTESIAN_POINT ( 'NONE',  ( -1.381305061119999955, -100.8816835080000089, -15.73378738089999729 ) ) ;
#10516 = ADVANCED_FACE ( 'NONE', ( #15455 ), #208, .T. ) ;
#10517 = FACE_OUTER_BOUND ( 'NONE', #26931, .T. ) ;
#10518 = DIRECTION ( 'NONE',  ( 0.4794255386042038936, 0.000000000000000000, 0.8775825618903723147 ) ) ;
#10519 = CARTESIAN_POINT ( 'NONE',  ( -13.32816333360000094, -111.0000000000000000, -11.12411022969999941 ) ) ;
#10520 = EDGE_CURVE ( 'NONE', #12535, #15620, #9785, .T. ) ;
#10521 = CARTESIAN_POINT ( 'NONE',  ( 16.09608533816492226, -94.75169073774321760, 17.24760066427640837 ) ) ;
#10522 = CARTESIAN_POINT ( 'NONE',  ( -22.53552307149999834, -71.00576155849999793, 16.55302470919999536 ) ) ;
#10523 = CARTESIAN_POINT ( 'NONE',  ( 0.000000000000000000, -82.25000000000000000, 0.000000000000000000 ) ) ;
#10524 = CARTESIAN_POINT ( 'NONE',  ( -12.53135398279999890, -65.65894985500000303, -22.11805201909999852 ) ) ;
#10525 = CARTESIAN_POINT ( 'NONE',  ( 24.24250217843501076, -94.10917102468839346, -9.048685009091679277 ) ) ;
#10526 = CARTESIAN_POINT ( 'NONE',  ( -39.12241743810000116, -66.42264973080000345, 0.4794255386039999456 ) ) ;
#10527 = ORIENTED_EDGE ( 'NONE', *, *, #25638, .F. ) ;
#10528 = CARTESIAN_POINT ( 'NONE',  ( 7.685455694319999864, -18.85523520590000146, -20.50116753240000023 ) ) ;
#10529 = VERTEX_POINT ( 'NONE', #16497 ) ;
#10530 = CARTESIAN_POINT ( 'NONE',  ( 22.30282385709999815, -36.18404282190000743, -10.32053919999999891 ) ) ;
#10531 = CARTESIAN_POINT ( 'NONE',  ( 7.356933064080000584, -36.56811125840000187, -21.47791245320000186 ) ) ;
#10532 = CARTESIAN_POINT ( 'NONE',  ( -28.98397190429999881, -92.96321827540000982, 3.119460853480000129 ) ) ;
#10533 = CARTESIAN_POINT ( 'NONE',  ( -41.74999999999475619, -63.24690319806150285, -1.908633995617260437 ) ) ;
#10534 = CARTESIAN_POINT ( 'NONE',  ( -38.25000000000000000, -65.00000000000000000, 1.587713240270000048 ) ) ;
#10535 = CARTESIAN_POINT ( 'NONE',  ( 15.58177396959999861, -100.4808658609999981, 4.510597657439999963 ) ) ;
#10536 = ORIENTED_EDGE ( 'NONE', *, *, #22819, .F. ) ;
#10537 = FACE_OUTER_BOUND ( 'NONE', #2008, .T. ) ;
#10538 = AXIS2_PLACEMENT_3D ( 'NONE', #21157, #25807, #8286 ) ;
#10539 = VERTEX_POINT ( 'NONE', #9922 ) ;
#10540 = CARTESIAN_POINT ( 'NONE',  ( -37.25000000000000000, -65.00000000000000000, -1.587713240270000048 ) ) ;
#10541 = EDGE_CURVE ( 'NONE', #28301, #15673, #13037, .T. ) ;
#10542 = CARTESIAN_POINT ( 'NONE',  ( -18.04504154990000231, -18.50000000000000000, 14.32575856849999951 ) ) ;
#10543 = EDGE_CURVE ( 'NONE', #10981, #5413, #27958, .T. ) ;
#10544 = MECHANICAL_DESIGN_GEOMETRIC_PRESENTATION_REPRESENTATION (  '', ( #8689 ), #4536 ) ;
#10545 = CARTESIAN_POINT ( 'NONE',  ( 11.70455088819999823, -93.00000000000000000, 8.942783294160001617 ) ) ;
#10546 = DIRECTION ( 'NONE',  ( 0.000000000000000000, 1.000000000000000000, 0.000000000000000000 ) ) ;
#10547 = CARTESIAN_POINT ( 'NONE',  ( -19.95528134719999969, -57.47855581339999986, 12.14623028109999936 ) ) ;
#10548 = ORIENTED_EDGE ( 'NONE', *, *, #4331, .T. ) ;
#10549 = FACE_OUTER_BOUND ( 'NONE', #17666, .T. ) ;
#10550 = CARTESIAN_POINT ( 'NONE',  ( -12.07947227870000084, -101.0956037589999994, -9.784155217600000398 ) ) ;
#10551 = EDGE_CURVE ( 'NONE', #21931, #25380, #11235, .T. ) ;
#10552 = LINE ( 'NONE', #12753, #8550 ) ;
#10553 = FACE_OUTER_BOUND ( 'NONE', #20731, .T. ) ;
#10554 = EDGE_LOOP ( 'NONE', ( #4156, #7455, #6279, #21040 ) ) ;
#10555 = EDGE_CURVE ( 'NONE', #19768, #27517, #9820, .T. ) ;
#10556 = CARTESIAN_POINT ( 'NONE',  ( -10.89815191770000169, -18.50000000000000000, -17.99090140869999743 ) ) ;
#10557 = AXIS2_PLACEMENT_3D ( 'NONE', #24508, #6886, #15751 ) ;
#10558 = CARTESIAN_POINT ( 'NONE',  ( -32.60214282289999943, -74.28456446479999897, -21.99410253310000130 ) ) ;
#10559 = CARTESIAN_POINT ( 'NONE',  ( 36.66437779740000025, -79.55211029950000068, -14.61455063210000205 ) ) ;
#10560 = EDGE_LOOP ( 'NONE', ( #3679, #19871, #10687, #12831 ) ) ;
#10561 = B_SPLINE_SURFACE_WITH_KNOTS ( 'NONE', 5, 5, ( 
 ( #21600, #10492, #10080, #8060, #3682, #8467, #27875, #14613, #10358 ),
 ( #23643, #26113, #21318, #1787, #19273, #15013, #23515, #19545, #18996 ),
 ( #1374, #7922, #16806, #10221, #25841, #5863, #12545, #21460, #14877 ),
 ( #17078, #28159, #8192, #25972, #3824, #19407, #22476, #24360, #8745 ),
 ( #26546, #15152, #12971, #20129, #11060, #4688, #24502, #15449, #24656 ),
 ( #20277, #2367, #26399, #19975, #15603, #24216, #6286, #8611, #4250 ),
 ( #8893, #26698, #6429, #13122, #10921, #28705, #17662, #6587, #4539 ),
 ( #11374, #19687, #21884, #15746, #15292, #48, #11223, #19828, #198 ),
 ( #24062, #1935, #2518, #4401, #13268, #344, #22177, #17369, #6739 ),
 ( #17807, #22034, #2217, #13417, #22319, #17513, #26265, #9048, #17952 ),
 ( #26846, #4101, #10775, #6880, #13567, #28577, #2082, #7320, #16489 ),
 ( #23066, #18244, #2959, #7480, #16047, #26993, #494, #24949, #642 ) ),
 .UNSPECIFIED., .F., .F., .F.,
 ( 6, 3, 3, 6 ),
 ( 6, 3, 6 ),
 ( 3.852920539459999905, 4.834764074400000666, 6.134713715030000181, 8.383984506220000910 ),
 ( 0.000000000000000000, 0.2500000000000000000, 0.5000000000000000000 ),
 .UNSPECIFIED. ) ;
#10562 = CARTESIAN_POINT ( 'NONE',  ( -1.776356839399999804E-15, -79.50000000000000000, 47.25000000000000000 ) ) ;
#10563 = ORIENTED_EDGE ( 'NONE', *, *, #15947, .T. ) ;
#10564 = VECTOR ( 'NONE', #3870, 1000.000000000000000 ) ;
#10565 = CARTESIAN_POINT ( 'NONE',  ( -12.04650752959999949, -69.29982884310000202, -25.46956806489999892 ) ) ;
#10566 = CARTESIAN_POINT ( 'NONE',  ( -19.49896612583845013, -96.70003212931756309, 8.002497787980619393 ) ) ;
#10567 = CIRCLE ( 'NONE', #14349, 7.249999999999999112 ) ;
#10568 = ORIENTED_EDGE ( 'NONE', *, *, #4169, .F. ) ;
#10569 = CARTESIAN_POINT ( 'NONE',  ( 20.49657866069999912, -57.47855601730000075, 11.20866246219999951 ) ) ;
#10570 = DIRECTION ( 'NONE',  ( 0.000000000000000000, -1.000000000000000000, 0.000000000000000000 ) ) ;
#10571 = ORIENTED_EDGE ( 'NONE', *, *, #3212, .F. ) ;
#10572 = CARTESIAN_POINT ( 'NONE',  ( -3.225656763162762175, -97.43022994611277454, -20.31916069606105069 ) ) ;
#10573 = CARTESIAN_POINT ( 'NONE',  ( 22.83075791639760510, -36.54217832149996781, -9.915197167589349547 ) ) ;
#10574 = CARTESIAN_POINT ( 'NONE',  ( 22.13892079547798630, -37.96769806959605376, -8.928661031997458863 ) ) ;
#10575 = FACE_OUTER_BOUND ( 'NONE', #16119, .T. ) ;
#10576 = DIRECTION ( 'NONE',  ( 0.000000000000000000, 1.000000000000000000, 0.000000000000000000 ) ) ;
#10577 = EDGE_LOOP ( 'NONE', ( #6661, #22850, #10161, #18708, #1887, #25631, #12356 ) ) ;
#10578 = ADVANCED_FACE ( 'NONE', ( #25256 ), #10692, .T. ) ;
#10579 = CARTESIAN_POINT ( 'NONE',  ( -18.72456657609999908, -96.53848370309999893, -10.28520937999999951 ) ) ;
#10580 = CARTESIAN_POINT ( 'NONE',  ( 12.97255956529999921, -101.0405520670000072, -9.781797840599999461 ) ) ;
#10581 = DIRECTION ( 'NONE',  ( -0.8391385125251890065, -0.000000000000000000, -0.5439177849611219751 ) ) ;
#10582 = ORIENTED_EDGE ( 'NONE', *, *, #17193, .T. ) ;
#10583 = CARTESIAN_POINT ( 'NONE',  ( 10.26571866753450735, -72.70657137122177005, -26.82921983142418654 ) ) ;
#10584 = CARTESIAN_POINT ( 'NONE',  ( -12.09704001540000107, -74.00000000000000000, 47.10905722069999513 ) ) ;
#10585 = VERTEX_POINT ( 'NONE', #17191 ) ;
#10586 = EDGE_CURVE ( 'NONE', #23988, #25155, #15866, .T. ) ;
#10587 = AXIS2_PLACEMENT_3D ( 'NONE', #11332, #26357, #26650 ) ;
#10588 = DIRECTION ( 'NONE',  ( 0.4794255386042036715, 0.000000000000000000, 0.8775825618903722036 ) ) ;
#10589 = AXIS2_PLACEMENT_3D ( 'NONE', #18707, #16935, #23217 ) ;
#10590 = CARTESIAN_POINT ( 'NONE',  ( 8.600016245220459155, -57.45905972565284259, -22.33353789330169903 ) ) ;
#10591 = CARTESIAN_POINT ( 'NONE',  ( 2.798556025240000070E-15, -74.00000000000000000, 3.175502518160000051E-15 ) ) ;
#10592 = DIRECTION ( 'NONE',  ( 0.000000000000000000, 1.000000000000000000, 0.000000000000000000 ) ) ;
#10593 = CARTESIAN_POINT ( 'NONE',  ( 0.03892854975575889276, -92.83160374581088092, -30.49997535110724911 ) ) ;
#10594 = UNCERTAINTY_MEASURE_WITH_UNIT (LENGTH_MEASURE( 1.000000000000000082E-05 ), #1392, 'distance_accuracy_value', 'NONE');
#10595 = FACE_OUTER_BOUND ( 'NONE', #19711, .T. ) ;
#10596 = VERTEX_POINT ( 'NONE', #12795 ) ;
#10597 = CARTESIAN_POINT ( 'NONE',  ( -39.75929607736751592, -73.82871504812071350, -7.246063797182709543 ) ) ;
#10599 = ORIENTED_EDGE ( 'NONE', *, *, #11834, .T. ) ;
#10598 = AXIS2_PLACEMENT_3D ( 'NONE', #7653, #14332, #20612 ) ;
#10600 = CARTESIAN_POINT ( 'NONE',  ( 21.59259415360000034, -37.41349446709999427, -8.074292674670001446 ) ) ;
#10601 = CARTESIAN_POINT ( 'NONE',  ( 7.215414233289999757, -74.50000000000000000, 40.70731707320000226 ) ) ;
#10602 = ORIENTED_EDGE ( 'NONE', *, *, #17001, .T. ) ;
#10603 = CARTESIAN_POINT ( 'NONE',  ( -12.76745321220000129, -101.1364147039999892, -8.514038431850000421 ) ) ;
#10604 = CIRCLE ( 'NONE', #18105, 0.5000000000000027756 ) ;
#10605 = CIRCLE ( 'NONE', #14387, 1.000000000000000444 ) ;
#10606 = CARTESIAN_POINT ( 'NONE',  ( -40.70731707320000226, -82.25000000000000000, 7.215414233289999757 ) ) ;
#10607 = LINE ( 'NONE', #1767, #21051 ) ;
#10608 = ORIENTED_EDGE ( 'NONE', *, *, #6241, .F. ) ;
#10609 = CIRCLE ( 'NONE', #4601, 30.50000000000000000 ) ;
#10610 = CARTESIAN_POINT ( 'NONE',  ( 0.000000000000000000, -2.000000000000000000, 0.000000000000000000 ) ) ;
#10611 = DIRECTION ( 'NONE',  ( 0.4794255386042038936, 0.000000000000000000, 0.8775825618903723147 ) ) ;
#10612 = EDGE_CURVE ( 'NONE', #24581, #14960, #22861, .T. ) ;
#10613 = DIRECTION ( 'NONE',  ( 0.000000000000000000, 0.000000000000000000, 1.000000000000000000 ) ) ;
#10614 = CARTESIAN_POINT ( 'NONE',  ( -29.70568929799252800, -92.71346081467955003, 6.915347693732913470 ) ) ;
#10615 = ORIENTED_EDGE ( 'NONE', *, *, #5734, .T. ) ;
#10616 = EDGE_CURVE ( 'NONE', #11515, #27229, #21898, .T. ) ;
#10617 = CARTESIAN_POINT ( 'NONE',  ( 12.73554887757679310, -101.5026031440401368, -9.870240380742313135 ) ) ;
#10618 = CARTESIAN_POINT ( 'NONE',  ( 24.58067739159999832, -26.99662418180000145, 1.425465004250000112 ) ) ;
#10619 = CARTESIAN_POINT ( 'NONE',  ( 23.63993607689999976, -65.72572872239999242, 10.85718295470000072 ) ) ;
#10620 = CARTESIAN_POINT ( 'NONE',  ( -15.84587239670000258, -101.4177331369999990, 3.264600553649999792 ) ) ;
#10621 = ORIENTED_EDGE ( 'NONE', *, *, #21014, .F. ) ;
#10622 = CARTESIAN_POINT ( 'NONE',  ( 0.000000000000000000, -26.59999999999999787, 0.000000000000000000 ) ) ;
#10623 = ADVANCED_FACE ( 'NONE', ( #10595 ), #19513, .F. ) ;
#10624 = DIRECTION ( 'NONE',  ( 1.000000000000000000, 0.000000000000000000, 0.000000000000000000 ) ) ;
#10625 = DIRECTION ( 'NONE',  ( 1.000000000000000000, 0.000000000000000000, 0.000000000000000000 ) ) ;
#10626 = CARTESIAN_POINT ( 'NONE',  ( -20.57915330399717746, -93.03394437611173373, 17.00111121841682760 ) ) ;
#10627 = ORIENTED_EDGE ( 'NONE', *, *, #22492, .T. ) ;
#10628 = EDGE_CURVE ( 'NONE', #21742, #2030, #25636, .T. ) ;
#10629 = CARTESIAN_POINT ( 'NONE',  ( 28.73411594649999756, -72.18745077389999665, 2.870220308499999984 ) ) ;
#10630 = VECTOR ( 'NONE', #15894, 1000.000000000000000 ) ;
#10631 = DIRECTION ( 'NONE',  ( 0.4794255386042000078, 0.000000000000000000, 0.8775825618903743131 ) ) ;
#10632 = CARTESIAN_POINT ( 'NONE',  ( 8.575410935299998982, -64.96415972239999803, -23.78692408539999903 ) ) ;
#10633 = CARTESIAN_POINT ( 'NONE',  ( -12.07243755420000042, -67.46050599719998786, -24.77969519869999715 ) ) ;
#10634 = CARTESIAN_POINT ( 'NONE',  ( -16.78865735879999832, -72.00000000000000000, 25.46808810279999946 ) ) ;
#10635 = DIRECTION ( 'NONE',  ( 1.000000000000000000, 0.000000000000000000, 0.000000000000000000 ) ) ;
#10636 = EDGE_LOOP ( 'NONE', ( #28464, #26396, #18355, #19045 ) ) ;
#10637 = CIRCLE ( 'NONE', #26976, 0.5000000000000027756 ) ;
#10638 = CIRCLE ( 'NONE', #25107, 60.85000000000000142 ) ;
#10639 = CARTESIAN_POINT ( 'NONE',  ( 6.737873477499999986, -100.1459902240000019, 15.55874246810000017 ) ) ;
#10640 = CARTESIAN_POINT ( 'NONE',  ( 15.75714761940000308, -101.3090757639999993, 4.024255779760000706 ) ) ;
#10641 = ORIENTED_EDGE ( 'NONE', *, *, #129, .T. ) ;
#10642 = CARTESIAN_POINT ( 'NONE',  ( -40.36777568491834245, -65.68647126653578994, -2.245284808034711421 ) ) ;
#10643 = CARTESIAN_POINT ( 'NONE',  ( 23.36120711399192018, -60.32159801849539349, 10.48029063133665950 ) ) ;
#10644 = CARTESIAN_POINT ( 'NONE',  ( 0.000000000000000000, -94.59276292389999696, 0.000000000000000000 ) ) ;
#10645 = ORIENTED_EDGE ( 'NONE', *, *, #1571, .T. ) ;
#10646 = CARTESIAN_POINT ( 'NONE',  ( 1.957052877659999801, -92.91851489729999969, -29.74816621520000126 ) ) ;
#10647 = CARTESIAN_POINT ( 'NONE',  ( 7.102042752109999135, -101.6484611540000031, 14.33739825589999839 ) ) ;
#10648 = CARTESIAN_POINT ( 'NONE',  ( -6.752147290549999958, -101.1180794200000008, 13.97358175370000133 ) ) ;
#10649 = ORIENTED_EDGE ( 'NONE', *, *, #27516, .T. ) ;
#10650 = FACE_OUTER_BOUND ( 'NONE', #23455, .T. ) ;
#10651 = CARTESIAN_POINT ( 'NONE',  ( -12.48059356133589226, -101.2111896144776324, -10.54544150875332065 ) ) ;
#10652 = VERTEX_POINT ( 'NONE', #22287 ) ;
#10653 = CARTESIAN_POINT ( 'NONE',  ( 8.586027522829999370, -36.03056633890000171, -20.93209955569999892 ) ) ;
#10654 = CARTESIAN_POINT ( 'NONE',  ( -41.75000000000000000, -65.14977478849999670, 2.684678751729999480 ) ) ;
#10655 = ORIENTED_EDGE ( 'NONE', *, *, #8241, .F. ) ;
#10656 = AXIS2_PLACEMENT_3D ( 'NONE', #25373, #14142, #14421 ) ;
#10657 = AXIS2_PLACEMENT_3D ( 'NONE', #12400, #23225, #27744 ) ;
#10658 = EDGE_CURVE ( 'NONE', #24310, #4593, #25515, .T. ) ;
#10659 = CARTESIAN_POINT ( 'NONE',  ( -29.21843812340000213, -92.50000000000000000, 6.434616699369999360 ) ) ;
#10660 = CARTESIAN_POINT ( 'NONE',  ( 22.05393571419999788, -18.50000000000000000, 1.471539986210000039 ) ) ;
#10661 = CYLINDRICAL_SURFACE ( 'NONE', #10233, 34.89999999999999858 ) ;
#10662 = CARTESIAN_POINT ( 'NONE',  ( -40.00000000000000000, -84.50000000000000000, -1.998401444329999950E-16 ) ) ;
#10663 = CARTESIAN_POINT ( 'NONE',  ( 0.000000000000000000, -23.30310889129999907, 0.000000000000000000 ) ) ;
#10664 = EDGE_LOOP ( 'NONE', ( #1976, #9880, #26690, #764 ) ) ;
#10665 = EDGE_CURVE ( 'NONE', #3189, #8384, #23306, .T. ) ;
#10666 = CARTESIAN_POINT ( 'NONE',  ( 37.60355029590000697, -74.50000000000000000, 9.356041104380000917 ) ) ;
#10667 = CARTESIAN_POINT ( 'NONE',  ( 9.444187806723459033, -35.99901531098080909, -19.97576011151723563 ) ) ;
#10668 = CARTESIAN_POINT ( 'NONE',  ( 13.75075768692672540, -100.1517898586340038, -10.30023294644368903 ) ) ;
#10669 = CARTESIAN_POINT ( 'NONE',  ( -18.48779199151693220, -19.46686856770285345, 12.50825135346812012 ) ) ;
#10670 = CARTESIAN_POINT ( 'NONE',  ( 7.253824032229999830, -36.56890884879999959, -21.48302425329999821 ) ) ;
#10671 = CARTESIAN_POINT ( 'NONE',  ( 8.125631349740000786, -93.00000000000000000, 24.17072847820000092 ) ) ;
#10672 = ORIENTED_EDGE ( 'NONE', *, *, #22372, .F. ) ;
#10673 = CARTESIAN_POINT ( 'NONE',  ( 36.40080305970000296, -74.58594344089999595, -14.77956079149999979 ) ) ;
#10674 = CARTESIAN_POINT ( 'NONE',  ( 22.20987792570000252, -36.53611441549999483, -9.691267042979999857 ) ) ;
#10675 = AXIS2_PLACEMENT_3D ( 'NONE', #7728, #25359, #11931 ) ;
#10676 = CIRCLE ( 'NONE', #1432, 6.000000000000000000 ) ;
#10677 = EDGE_CURVE ( 'NONE', #2951, #19383, #10890, .T. ) ;
#10678 = CARTESIAN_POINT ( 'NONE',  ( -1.453418026390000062, -61.82150526550000080, -24.08281248540000163 ) ) ;
#10679 = DIRECTION ( 'NONE',  ( 1.000000000000000000, 0.000000000000000000, 0.000000000000000000 ) ) ;
#10680 = CARTESIAN_POINT ( 'NONE',  ( -19.95527576509999790, -57.47855601730000075, 12.14622657969999864 ) ) ;
#10681 = CARTESIAN_POINT ( 'NONE',  ( 0.000000000000000000, -107.5000000000000000, 0.000000000000000000 ) ) ;
#10682 = ORIENTED_EDGE ( 'NONE', *, *, #243, .T. ) ;
#10683 = CARTESIAN_POINT ( 'NONE',  ( -19.95527577780000072, -57.47855601759999900, 12.14622656770000120 ) ) ;
#10684 = CARTESIAN_POINT ( 'NONE',  ( 7.252014196660000245, -74.29300278830000082, -40.34091732179999923 ) ) ;
#10685 = ORIENTED_EDGE ( 'NONE', *, *, #27258, .T. ) ;
#10686 = FACE_OUTER_BOUND ( 'NONE', #5080, .T. ) ;
#10687 = ORIENTED_EDGE ( 'NONE', *, *, #18763, .F. ) ;
#10688 = EDGE_CURVE ( 'NONE', #16942, #19419, #19587, .T. ) ;
#10689 = CARTESIAN_POINT ( 'NONE',  ( 21.83467201959999926, -39.32886505740000160, 9.827746952760001875 ) ) ;
#10690 = AXIS2_PLACEMENT_3D ( 'NONE', #5551, #14565, #21006 ) ;
#10691 = CARTESIAN_POINT ( 'NONE',  ( -22.13657418456727299, -74.09627300783152748, -32.45321636354270822 ) ) ;
#10692 = TOROIDAL_SURFACE ( 'NONE', #26099, 6.750000000000000000, 0.5000000000000000000 ) ;
#10693 = CIRCLE ( 'NONE', #28398, 1.999999999999998890 ) ;
#10694 = FACE_OUTER_BOUND ( 'NONE', #16638, .T. ) ;
#10695 = CARTESIAN_POINT ( 'NONE',  ( -32.23078363019764225, -74.03198227414637245, -22.08206013869884643 ) ) ;
#10696 = CARTESIAN_POINT ( 'NONE',  ( -29.86363316589999783, -93.00000000000000000, 0.3450520983969999622 ) ) ;
#10697 = EDGE_LOOP ( 'NONE', ( #4393, #9160, #26295, #20519 ) ) ;
#10698 = CARTESIAN_POINT ( 'NONE',  ( -31.00000000000000000, -15.00000000000000000, 4.500000000000000000 ) ) ;
#10699 = CARTESIAN_POINT ( 'NONE',  ( -22.65530694619999963, -72.00000000000000000, 18.22957389299999775 ) ) ;
#10700 = CARTESIAN_POINT ( 'NONE',  ( -7.834619151519719438, -100.6338045035611515, 14.85527437501940362 ) ) ;
#10701 = ORIENTED_EDGE ( 'NONE', *, *, #28663, .T. ) ;
#10702 = CARTESIAN_POINT ( 'NONE',  ( -1.283023294879999998, -101.3150694429999987, -16.20107482390000087 ) ) ;
#10703 = CARTESIAN_POINT ( 'NONE',  ( 6.114061450890000415, -111.0000000000000000, -13.40104985119999981 ) ) ;
#10704 = ORIENTED_EDGE ( 'NONE', *, *, #18873, .F. ) ;
#10705 = ADVANCED_FACE ( 'NONE', ( #9886 ), #12144, .F. ) ;
#10706 = CARTESIAN_POINT ( 'NONE',  ( 19.99313163150000250, -36.00000036840000206, -9.451827061030000365 ) ) ;
#10707 = AXIS2_PLACEMENT_3D ( 'NONE', #4871, #13752, #527 ) ;
#10708 = CARTESIAN_POINT ( 'NONE',  ( 12.02508340220000171, -92.51167569919999778, 27.24521537120000048 ) ) ;
#10709 = AXIS2_PLACEMENT_3D ( 'NONE', #25905, #21816, #23717 ) ;
#10710 = ORIENTED_EDGE ( 'NONE', *, *, #12761, .T. ) ;
#10711 = CIRCLE ( 'NONE', #10274, 3.749999999999996447 ) ;
#10712 = CARTESIAN_POINT ( 'NONE',  ( -19.86057790159999925, -54.24814459719999604, 12.08483967110000101 ) ) ;
#10713 = CARTESIAN_POINT ( 'NONE',  ( -16.34073580590758112, -93.59825774987527325, -21.52464356387743294 ) ) ;
#10714 = ORIENTED_EDGE ( 'NONE', *, *, #23998, .T. ) ;
#10715 = CARTESIAN_POINT ( 'NONE',  ( 23.09098980150000102, -54.98594849529999351, 10.35171084059999913 ) ) ;
#10716 = CARTESIAN_POINT ( 'NONE',  ( 45.89652018349999452, -73.81415926540000783, -4.323400012419999605 ) ) ;
#10717 = EDGE_CURVE ( 'NONE', #3822, #25360, #25160, .T. ) ;
#10718 = ORIENTED_EDGE ( 'NONE', *, *, #19062, .T. ) ;
#10719 = DIRECTION ( 'NONE',  ( -6.123031769109999188E-17, 0.000000000000000000, 1.000000000000000000 ) ) ;
#10720 = CARTESIAN_POINT ( 'NONE',  ( -40.00000000000000000, -94.00000000000000000, 0.000000000000000000 ) ) ;
#10721 = CARTESIAN_POINT ( 'NONE',  ( 9.807088892109998568, -36.00000000000000000, -20.27618918270000137 ) ) ;
#10722 = CARTESIAN_POINT ( 'NONE',  ( -16.46937899769999802, -93.21603264569999681, -21.54563518039999792 ) ) ;
#10723 = CARTESIAN_POINT ( 'NONE',  ( -17.05574026919999753, -93.34713166629998682, 21.78488634390000200 ) ) ;
#10724 = ORIENTED_EDGE ( 'NONE', *, *, #8030, .F. ) ;
#10725 = DIRECTION ( 'NONE',  ( -0.8775825618903722036, 0.000000000000000000, 0.4794255386042041156 ) ) ;
#10726 = CARTESIAN_POINT ( 'NONE',  ( 13.23566414709999961, -100.6809449770000100, -9.745096673970000012 ) ) ;
#10727 = DIRECTION ( 'NONE',  ( 0.000000000000000000, 1.000000000000000000, 0.000000000000000000 ) ) ;
#10728 = CARTESIAN_POINT ( 'NONE',  ( -1.990166961069999907, -53.82492386869999734, -23.72420749220000147 ) ) ;
#10729 = AXIS2_PLACEMENT_3D ( 'NONE', #22173, #27281, #15895 ) ;
#10730 = CARTESIAN_POINT ( 'NONE',  ( 30.00028607799999847, -92.50000000000000000, 5.498439345520000465 ) ) ;
#10731 = CARTESIAN_POINT ( 'NONE',  ( -19.41166767530000214, -18.86932112550000085, 14.42276170449999917 ) ) ;
#10732 = EDGE_LOOP ( 'NONE', ( #6970, #28346, #21430, #1075 ) ) ;
#10733 = CIRCLE ( 'NONE', #27074, 15.19391340349999986 ) ;
#10734 = SHAPE_REPRESENTATION ( 'Water Pump Main Cast Housing', ( #26433 ), #911 ) ;
#10735 = CARTESIAN_POINT ( 'NONE',  ( -4.500000000000000000, -12.50000000000000000, -50.00000000000000000 ) ) ;
#10736 = CARTESIAN_POINT ( 'NONE',  ( -42.25000000000000000, -63.30468293320000583, 0.7216878364880000563 ) ) ;
#10737 = CARTESIAN_POINT ( 'NONE',  ( 4.420730772149999765, -92.67327634539999792, -27.51018170170000232 ) ) ;
#10738 = CARTESIAN_POINT ( 'NONE',  ( 18.58445413780000166, -18.50000000000000000, 9.853938316409998066 ) ) ;
#10739 = CARTESIAN_POINT ( 'NONE',  ( -38.55000000000000426, -65.14977478849999670, 2.857883832489999776 ) ) ;
#10740 = B_SPLINE_SURFACE_WITH_KNOTS ( 'NONE', 5, 5, ( 
 ( #3191, #27673, #13293, #24087, #23952, #16718 ),
 ( #15319, #14523, #23426, #28310, #28600, #12997 ),
 ( #10002, #22197, #12846, #18915, #3465, #22059 ),
 ( #27795, #1811, #24239, #1959, #17249, #12331 ),
 ( #26570, #21239, #19572, #28458, #17394, #26426 ),
 ( #8769, #26288, #21760, #6312, #3987, #8495 ) ),
 .UNSPECIFIED., .F., .F., .F.,
 ( 6, 6 ),
 ( 6, 6 ),
 ( 7.179431123200000542, 23.44689954300000068 ),
 ( 0.000000000000000000, 0.5000000000000000000 ),
 .UNSPECIFIED. ) ;
#10741 = CARTESIAN_POINT ( 'NONE',  ( 0.000000000000000000, -2.000000000000000000, 0.000000000000000000 ) ) ;
#10742 = PRODUCT_DEFINITION ( 'UNKNOWN', '', #3653, #3619 ) ;
#10743 = CARTESIAN_POINT ( 'NONE',  ( -11.85289073049999864, -94.98812769020000246, -21.44326021599999876 ) ) ;
#10744 = ADVANCED_FACE ( 'NONE', ( #21534 ), #2383, .F. ) ;
#10745 = ORIENTED_EDGE ( 'NONE', *, *, #6844, .F. ) ;
#10746 = AXIS2_PLACEMENT_3D ( 'NONE', #1570, #10413, #16997 ) ;
#10747 = CARTESIAN_POINT ( 'NONE',  ( 19.60969031579999822, -98.43722211769998864, -0.3265172099129999839 ) ) ;
#10748 = ORIENTED_EDGE ( 'NONE', *, *, #1884, .T. ) ;
#10749 = CARTESIAN_POINT ( 'NONE',  ( 19.86198292329999759, -35.82855941500000085, -9.092038893569998947 ) ) ;
#10750 = CYLINDRICAL_SURFACE ( 'NONE', #4174, 3.000000000000001332 ) ;
#10751 = ADVANCED_FACE ( 'NONE', ( #19624 ), #7857, .T. ) ;
#10752 = ORIENTED_EDGE ( 'NONE', *, *, #91, .F. ) ;
#10753 = CIRCLE ( 'NONE', #12182, 3.000000000000002665 ) ;
#10754 = CARTESIAN_POINT ( 'NONE',  ( 16.54056940490000116, -94.89196973119999257, 16.94454239999999956 ) ) ;
#10755 = EDGE_CURVE ( 'NONE', #23918, #25360, #6815, .T. ) ;
#10756 = FACE_OUTER_BOUND ( 'NONE', #8742, .T. ) ;
#10757 = DIRECTION ( 'NONE',  ( 1.000000000000000000, 0.000000000000000000, 0.000000000000000000 ) ) ;
#10758 = CARTESIAN_POINT ( 'NONE',  ( 7.286238495500000134, -101.2500498790000023, 13.33737010350000141 ) ) ;
#10759 = CARTESIAN_POINT ( 'NONE',  ( -30.39212651620044170, -92.86276748823678417, 2.566209473271955144 ) ) ;
#10760 = CARTESIAN_POINT ( 'NONE',  ( 9.238026508649999968, -49.06719615769999621, -22.71123055929999879 ) ) ;
#10761 = CARTESIAN_POINT ( 'NONE',  ( 0.000000000000000000, -2.000000000000000000, 0.000000000000000000 ) ) ;
#10762 = DIRECTION ( 'NONE',  ( 0.4509255599460827435, -0.3396444637780623443, 0.8254137008871517134 ) ) ;
#10763 = ORIENTED_EDGE ( 'NONE', *, *, #20681, .F. ) ;
#10764 = CARTESIAN_POINT ( 'NONE',  ( 13.42574138988457655, -100.7538407676048848, -9.930469818722173159 ) ) ;
#10765 = DIRECTION ( 'NONE',  ( -0.9704142011833030157, 0.000000000000000000, 0.2414462220490760924 ) ) ;
#10766 = CARTESIAN_POINT ( 'NONE',  ( 25.86461527650000036, -68.93885193590000426, 10.86608366989999830 ) ) ;
#10767 = CARTESIAN_POINT ( 'NONE',  ( 8.831073959190000267, -94.59276583650000703, -22.09757114230000141 ) ) ;
#10768 = EDGE_LOOP ( 'NONE', ( #15539, #1014, #23530, #4913, #16866, #7576, #24130 ) ) ;
#10769 = FACE_OUTER_BOUND ( 'NONE', #7128, .T. ) ;
#10770 = CARTESIAN_POINT ( 'NONE',  ( -15.25386055589999934, -92.94769410010000854, 25.12374163710000019 ) ) ;
#10771 = CARTESIAN_POINT ( 'NONE',  ( -20.34767246214833847, -92.64526570559976903, 19.18952924589508413 ) ) ;
#10772 = VERTEX_POINT ( 'NONE', #9126 ) ;
#10773 = DIRECTION ( 'NONE',  ( 1.000000000000000000, 0.000000000000000000, -1.203338504109999799E-16 ) ) ;
#10774 = AXIS2_PLACEMENT_3D ( 'NONE', #15805, #16397, #5187 ) ;
#10775 = CARTESIAN_POINT ( 'NONE',  ( 0.5694848120150000081, -99.99711545080000974, -17.16320790510000194 ) ) ;
#10776 = CARTESIAN_POINT ( 'NONE',  ( 25.67840951673019134, -74.29132473649202950, -29.62461545363389703 ) ) ;
#10777 = CARTESIAN_POINT ( 'NONE',  ( 15.03693308380000104, -101.1848541609999899, 2.726188632040000392 ) ) ;
#10778 = CARTESIAN_POINT ( 'NONE',  ( 22.28403574200000037, -58.27079767440000069, 10.15038429719999868 ) ) ;
#10779 = CARTESIAN_POINT ( 'NONE',  ( -11.21295062929999986, -49.81670839429999376, -22.19244673080000041 ) ) ;
#10780 = AXIS2_PLACEMENT_3D ( 'NONE', #5327, #23106, #3146 ) ;
#10781 = VERTEX_POINT ( 'NONE', #13651 ) ;
#10782 = PLANE ( 'NONE',  #15702 ) ;
#10783 = CARTESIAN_POINT ( 'NONE',  ( 15.12841431370000045, -101.0956037589999994, 3.574132650939999767 ) ) ;
#10784 = CARTESIAN_POINT ( 'NONE',  ( -5.902985309178900408, -97.42330309878559547, 19.71785937141702405 ) ) ;
#10785 = EDGE_CURVE ( 'NONE', #11872, #24375, #7957, .T. ) ;
#10786 = ORIENTED_EDGE ( 'NONE', *, *, #10551, .F. ) ;
#10787 = CARTESIAN_POINT ( 'NONE',  ( -16.44063509269999912, -92.87228942340000515, 21.55809250360000107 ) ) ;
#10788 = CARTESIAN_POINT ( 'NONE',  ( 4.811931075225057697, -92.71525149899693474, -30.11819794593843724 ) ) ;
#10789 = CARTESIAN_POINT ( 'NONE',  ( -4.472380792810000116, -95.66919271819999437, 22.06157936329999814 ) ) ;
#10790 = ORIENTED_EDGE ( 'NONE', *, *, #14200, .F. ) ;
#10791 = CARTESIAN_POINT ( 'NONE',  ( 4.725730692399999988, -92.90721294759998727, -27.95382239220000287 ) ) ;
#10792 = EDGE_CURVE ( 'NONE', #23252, #10529, #63, .T. ) ;
#10793 = CARTESIAN_POINT ( 'NONE',  ( 20.59195074500000189, -22.47117435080000192, -8.142470642490000188 ) ) ;
#10794 = CARTESIAN_POINT ( 'NONE',  ( -15.42268960139999834, -101.1889999979999999, 4.259183661159999801 ) ) ;
#10795 = PLANE ( 'NONE',  #15401 ) ;
#10796 = ORIENTED_EDGE ( 'NONE', *, *, #14963, .T. ) ;
#10797 = AXIS2_PLACEMENT_3D ( 'NONE', #19152, #12010, #8078 ) ;
#10798 = CARTESIAN_POINT ( 'NONE',  ( 32.25000000000000000, -73.50000000000000000, 1.484822157706350179E-15 ) ) ;
#10799 = AXIS2_PLACEMENT_3D ( 'NONE', #17604, #24596, #20222 ) ;
#10800 = CARTESIAN_POINT ( 'NONE',  ( -13.10181604453989124, -100.1517898586368460, -11.11398002738276070 ) ) ;
#10801 = ORIENTED_EDGE ( 'NONE', *, *, #129, .F. ) ;
#10802 = DIRECTION ( 'NONE',  ( 0.000000000000000000, -1.000000000000000000, 0.000000000000000000 ) ) ;
#10803 = CIRCLE ( 'NONE', #27144, 18.64285714289999873 ) ;
#10804 = DIRECTION ( 'NONE',  ( -0.7414446217286150276, 0.000000000000000000, -0.6710140631236509723 ) ) ;
#10805 = EDGE_LOOP ( 'NONE', ( #22674, #27558, #11818, #11495 ) ) ;
#10806 = CARTESIAN_POINT ( 'NONE',  ( 9.753760903854669095, -93.20709273739691980, -25.68565009221217466 ) ) ;
#10807 = CARTESIAN_POINT ( 'NONE',  ( -37.75000000000000000, -63.30468293320000583, 0.7216878364859999895 ) ) ;
#10808 = CARTESIAN_POINT ( 'NONE',  ( -12.27251325432490781, -19.47282290365338397, 19.18777339616194055 ) ) ;
#10809 = CARTESIAN_POINT ( 'NONE',  ( -19.89498170407338407, -92.54383083955177369, -23.11796002674290307 ) ) ;
#10810 = VERTEX_POINT ( 'NONE', #28511 ) ;
#10811 = CARTESIAN_POINT ( 'NONE',  ( -15.13778281370000123, -101.1716780380000102, 4.291020750220000401 ) ) ;
#10812 = CARTESIAN_POINT ( 'NONE',  ( -13.84192735959999965, -18.50000000000000000, 18.94933192010000056 ) ) ;
#10813 = CARTESIAN_POINT ( 'NONE',  ( 19.69582338720000081, -18.50000000000000000, -7.383548592259999488 ) ) ;
#10814 = CARTESIAN_POINT ( 'NONE',  ( -36.71401968334630794, -65.10234783420575866, -0.07523755576584739702 ) ) ;
#10815 = AXIS2_PLACEMENT_3D ( 'NONE', #11555, #20464, #11859 ) ;
#10816 = CARTESIAN_POINT ( 'NONE',  ( 13.74822071429026771, -100.1585711159249570, -10.29449286259888297 ) ) ;
#10817 = LINE ( 'NONE', #24535, #20356 ) ;
#10818 = CARTESIAN_POINT ( 'NONE',  ( 24.52093283500401455, -93.74885976995108194, -10.40268822211655397 ) ) ;
#10819 = CARTESIAN_POINT ( 'NONE',  ( 18.98656275410000305, -20.74345739960000401, -9.020322599649999162 ) ) ;
#10820 = VERTEX_POINT ( 'NONE', #2014 ) ;
#10821 = CARTESIAN_POINT ( 'NONE',  ( -13.18688177930000016, -93.32822605769999313, -23.58441486170000090 ) ) ;
#10822 = EDGE_CURVE ( 'NONE', #17492, #13409, #24230, .T. ) ;
#10823 = ORIENTED_EDGE ( 'NONE', *, *, #13548, .T. ) ;
#10824 = CARTESIAN_POINT ( 'NONE',  ( -2.646733530900000186, -62.35648592489999942, -25.81438035669999564 ) ) ;
#10825 = CARTESIAN_POINT ( 'NONE',  ( 9.022692971490000602, -37.05206027789999723, -21.94388125080000052 ) ) ;
#10826 = CARTESIAN_POINT ( 'NONE',  ( -24.06374496360000137, -94.22763312380000400, -3.197736329870000116 ) ) ;
#10827 = CARTESIAN_POINT ( 'NONE',  ( -19.72357768420000212, -55.05548131559999803, 12.36420953449999871 ) ) ;
#10828 = CARTESIAN_POINT ( 'NONE',  ( 0.000000000000000000, -101.1889999979999999, 0.000000000000000000 ) ) ;
#10829 = ORIENTED_EDGE ( 'NONE', *, *, #2197, .T. ) ;
#10830 = AXIS2_PLACEMENT_3D ( 'NONE', #1779, #16291, #14399 ) ;
#10831 = CARTESIAN_POINT ( 'NONE',  ( 21.39448334389999928, -35.36119160450000010, -7.275524378479999221 ) ) ;
#10832 = CARTESIAN_POINT ( 'NONE',  ( 7.367357169079999935, -74.05258142279998879, -39.49501612619999946 ) ) ;
#10833 = VERTEX_POINT ( 'NONE', #13205 ) ;
#10834 = DIRECTION ( 'NONE',  ( 0.000000000000000000, 1.000000000000000000, 0.000000000000000000 ) ) ;
#10835 = CYLINDRICAL_SURFACE ( 'NONE', #18835, 0.1999999999999987899 ) ;
#10836 = B_SPLINE_CURVE_WITH_KNOTS ( 'NONE', 5,
 ( #24229, #19839, #11387, #28720, #8759, #7046 ),
 .UNSPECIFIED., .F., .F.,
 ( 6, 6 ),
 ( 0.000000000000000000, 1.000000000000000000 ),
 .UNSPECIFIED. ) ;
#10837 = CARTESIAN_POINT ( 'NONE',  ( -10.09856422800000075, -18.50000000000000000, -18.66762288940000403 ) ) ;
#10838 = VECTOR ( 'NONE', #4347, 1000.000000000000000 ) ;
#10839 = CARTESIAN_POINT ( 'NONE',  ( 0.000000000000000000, -19.40000000000000213, 0.000000000000000000 ) ) ;
#10840 = CARTESIAN_POINT ( 'NONE',  ( 26.69293917519999937, -29.89689110870000022, 48.86109741659999628 ) ) ;
#10841 = CARTESIAN_POINT ( 'NONE',  ( -17.60247688846170888, -95.05882272216540230, 15.10979806272066917 ) ) ;
#10842 = EDGE_CURVE ( 'NONE', #2729, #14760, #10992, .T. ) ;
#10843 = ORIENTED_EDGE ( 'NONE', *, *, #9448, .T. ) ;
#10844 = DIRECTION ( 'NONE',  ( 1.000000000000000000, 0.000000000000000000, 0.000000000000000000 ) ) ;
#10845 = CARTESIAN_POINT ( 'NONE',  ( -12.44240347620000087, -101.3878691800000098, -10.22198205940000015 ) ) ;
#10846 = CARTESIAN_POINT ( 'NONE',  ( 22.85380330025371265, -61.78215645786973909, -7.276638066883097444 ) ) ;
#10847 = ORIENTED_EDGE ( 'NONE', *, *, #21067, .T. ) ;
#10848 = CIRCLE ( 'NONE', #2525, 0.5000000000000004441 ) ;
#10849 = CARTESIAN_POINT ( 'NONE',  ( 8.472395020760000506, -37.95144078679999922, -21.79230213740000011 ) ) ;
#10850 = CARTESIAN_POINT ( 'NONE',  ( 36.75955791450000021, -80.34763096870000254, -13.75991944210000106 ) ) ;
#10851 = EDGE_LOOP ( 'NONE', ( #28444, #21277, #612, #17736 ) ) ;
#10852 = EDGE_CURVE ( 'NONE', #16224, #22982, #17726, .T. ) ;
#10853 = EDGE_CURVE ( 'NONE', #28363, #22254, #720, .T. ) ;
#10854 = CARTESIAN_POINT ( 'NONE',  ( 25.26718046270000073, -72.00000000000000000, 6.129403842640000377 ) ) ;
#10855 = CARTESIAN_POINT ( 'NONE',  ( -22.71848792900000191, -80.00000000000000000, -32.61798286559999838 ) ) ;
#10856 = CARTESIAN_POINT ( 'NONE',  ( -0.5421338679160000451, -57.91805294160000273, -23.37022173519999768 ) ) ;
#10857 = ORIENTED_EDGE ( 'NONE', *, *, #28166, .T. ) ;
#10858 = CARTESIAN_POINT ( 'NONE',  ( -19.88469613148559390, -96.02299627876102761, 9.294782919059894510 ) ) ;
#10859 = ORIENTED_EDGE ( 'NONE', *, *, #4859, .T. ) ;
#10860 = CARTESIAN_POINT ( 'NONE',  ( 22.06554121350000131, -93.81709728810000115, 13.31880052350000021 ) ) ;
#10861 = CARTESIAN_POINT ( 'NONE',  ( 0.000000000000000000, -19.46510050329999686, 0.000000000000000000 ) ) ;
#10862 = ORIENTED_EDGE ( 'NONE', *, *, #7322, .T. ) ;
#10863 = CARTESIAN_POINT ( 'NONE',  ( -41.76016118384315945, -65.69391135771232371, 1.423064894540761349 ) ) ;
#10864 = CARTESIAN_POINT ( 'NONE',  ( -22.62871153299999705, -80.00000000000000000, -32.48908674569999988 ) ) ;
#10865 = TOROIDAL_SURFACE ( 'NONE', #3042, 5.500000000000000000, 0.5000000000000000000 ) ;
#10866 = PLANE ( 'NONE',  #13428 ) ;
#10867 = CARTESIAN_POINT ( 'NONE',  ( 12.44788637039999912, -101.5369810359999860, -10.05268415809999993 ) ) ;
#10868 = CARTESIAN_POINT ( 'NONE',  ( -20.30146180590000071, -92.55031878709998239, -20.19289408079999859 ) ) ;
#10869 = CARTESIAN_POINT ( 'NONE',  ( 6.114061450880000415, -93.00000000000000000, -13.40104985119999981 ) ) ;
#10870 = ORIENTED_EDGE ( 'NONE', *, *, #2988, .T. ) ;
#10871 = DIRECTION ( 'NONE',  ( 1.000000000000000000, 0.000000000000000000, 0.000000000000000000 ) ) ;
#10872 = CARTESIAN_POINT ( 'NONE',  ( 12.57051157029999899, -101.4908759489999994, -9.948597786639998830 ) ) ;
#10873 = FACE_BOUND ( 'NONE', #23002, .T. ) ;
#10874 = EDGE_CURVE ( 'NONE', #15494, #13209, #11185, .T. ) ;
#10875 = CARTESIAN_POINT ( 'NONE',  ( -0.5413028955969999556, -57.47855601730000075, -23.35488904190000170 ) ) ;
#10876 = CARTESIAN_POINT ( 'NONE',  ( -11.78548194719999920, -15.31994771319999948, -21.57317999869999881 ) ) ;
#10877 = AXIS2_PLACEMENT_3D ( 'NONE', #19865, #4435, #11261 ) ;
#10878 = CARTESIAN_POINT ( 'NONE',  ( 10.38182607682433378, -72.67376041724993740, -26.81396579421036463 ) ) ;
#10879 = CARTESIAN_POINT ( 'NONE',  ( -19.47508940490000029, -19.49504784870000051, 14.31286723660000071 ) ) ;
#10880 = ORIENTED_EDGE ( 'NONE', *, *, #28443, .T. ) ;
#10881 = CARTESIAN_POINT ( 'NONE',  ( -38.25000000000463984, -63.24690319806150285, 1.908633995616615397 ) ) ;
#10882 = AXIS2_PLACEMENT_3D ( 'NONE', #131, #13496, #24880 ) ;
#10883 = PLANE ( 'NONE',  #25946 ) ;
#10884 = CARTESIAN_POINT ( 'NONE',  ( 26.77683864449999973, -30.20000000000000284, 49.01467436490000296 ) ) ;
#10885 = CARTESIAN_POINT ( 'NONE',  ( -38.25000000000000000, -65.56519245710001087, 1.769653913539999790 ) ) ;
#10886 = CARTESIAN_POINT ( 'NONE',  ( -0.1318277626668340474, -92.71346081467603994, -30.49971527465584842 ) ) ;
#10887 = FACE_OUTER_BOUND ( 'NONE', #17402, .T. ) ;
#10888 = AXIS2_PLACEMENT_3D ( 'NONE', #15290, #2216, #4249 ) ;
#10889 = B_SPLINE_CURVE_WITH_KNOTS ( 'NONE', 3,
 ( #1079, #3246, #18245, #25522, #27286, #5558 ),
 .UNSPECIFIED., .F., .F.,
 ( 4, 2, 4 ),
 ( 0.000000000000000000, 0.5000000000000000000, 1.000000000000000000 ),
 .UNSPECIFIED. ) ;
#10890 = LINE ( 'NONE', #22148, #20518 ) ;
#10891 = CARTESIAN_POINT ( 'NONE',  ( -11.38188502134437385, -94.78087563376180924, -20.62155828120727108 ) ) ;
#10892 = EDGE_LOOP ( 'NONE', ( #262, #5160, #9798, #24558, #4223 ) ) ;
#10893 = B_SPLINE_CURVE_WITH_KNOTS ( 'NONE', 5,
 ( #19376, #24323, #4063, #10322, #28124, #17481, #17048, #22714, #27232 ),
 .UNSPECIFIED., .F., .F.,
 ( 6, 3, 6 ),
 ( 0.000000000000000000, 0.5000000000000000000, 1.000000000000000000 ),
 .UNSPECIFIED. ) ;
#10894 = CARTESIAN_POINT ( 'NONE',  ( 19.67779709110000042, -98.51736893609999868, -0.3242707669709999907 ) ) ;
#10895 = ORIENTED_EDGE ( 'NONE', *, *, #25330, .F. ) ;
#10896 = CARTESIAN_POINT ( 'NONE',  ( -11.62935565859999798, -49.87337825049999651, 20.03543646159999980 ) ) ;
#10897 = CARTESIAN_POINT ( 'NONE',  ( 7.383549334360000493, -18.50000000000000000, -19.69582310909999734 ) ) ;
#10898 = VERTEX_POINT ( 'NONE', #3045 ) ;
#10899 = CARTESIAN_POINT ( 'NONE',  ( -25.77179612209999959, -37.57799544290000426, -47.17495636800000369 ) ) ;
#10900 = CARTESIAN_POINT ( 'NONE',  ( -3.240188565246664432, -67.45413847081940162, -27.37092558598135028 ) ) ;
#10901 = AXIS2_PLACEMENT_3D ( 'NONE', #13352, #19769, #26631 ) ;
#10902 = CARTESIAN_POINT ( 'NONE',  ( -4.523871465800000990, -98.54854614750000508, -18.92597532359999946 ) ) ;
#10903 = CARTESIAN_POINT ( 'NONE',  ( 9.332951828819998852, -36.18018306619999436, -21.06416784469999826 ) ) ;
#10904 = CARTESIAN_POINT ( 'NONE',  ( -20.19758353400000317, -95.55441921500001001, 10.16704513559999867 ) ) ;
#10905 = CARTESIAN_POINT ( 'NONE',  ( -29.54921749321805180, -92.53260370677851654, 7.556178546955753639 ) ) ;
#10906 = CARTESIAN_POINT ( 'NONE',  ( 6.880103916109999496, -101.6484611540000031, 13.88935456040000105 ) ) ;
#10907 = ORIENTED_EDGE ( 'NONE', *, *, #7254, .F. ) ;
#10908 = SHAPE_REPRESENTATION ( 'Coolant Impeller Vanes', ( #26433 ), #17143 ) ;
#10909 = DIRECTION ( 'NONE',  ( 0.000000000000000000, 1.000000000000000000, 0.000000000000000000 ) ) ;
#10910 = CARTESIAN_POINT ( 'NONE',  ( 23.35417710990000373, -57.47855602609999437, -0.5711871778539999722 ) ) ;
#10911 = DIRECTION ( 'NONE',  ( 1.000000000000000000, 0.000000000000000000, 0.000000000000000000 ) ) ;
#10912 = CARTESIAN_POINT ( 'NONE',  ( 39.30828467216858968, -73.61493928630405037, 7.216929735073121854 ) ) ;
#10913 = ORIENTED_EDGE ( 'NONE', *, *, #24174, .T. ) ;
#10914 = B_SPLINE_CURVE_WITH_KNOTS ( 'NONE', 3,
 ( #10196, #14454, #7768, #5840, #21435, #25401 ),
 .UNSPECIFIED., .F., .F.,
 ( 4, 2, 4 ),
 ( 0.000000000000000000, 0.5000000000000000000, 1.000000000000000000 ),
 .UNSPECIFIED. ) ;
#10915 = CARTESIAN_POINT ( 'NONE',  ( -38.70548889989999708, -73.81415926540000783, 7.196178079599999222 ) ) ;
#10916 = CARTESIAN_POINT ( 'NONE',  ( -13.45765177410000035, -92.63554508160000012, 27.09946297289999961 ) ) ;
#10917 = DIRECTION ( 'NONE',  ( 1.000000000000000000, 0.000000000000000000, 0.000000000000000000 ) ) ;
#10918 = ORIENTED_EDGE ( 'NONE', *, *, #18879, .T. ) ;
#10919 = ADVANCED_FACE ( 'NONE', ( #11896 ), #10107, .F. ) ;
#10920 = CARTESIAN_POINT ( 'NONE',  ( 28.19138828400000207, -71.67693266270001118, 1.948646730969999963 ) ) ;
#10921 = CARTESIAN_POINT ( 'NONE',  ( 0.5104505476449999746, -100.8455998110000138, -16.03521346039999784 ) ) ;
#10922 = CARTESIAN_POINT ( 'NONE',  ( 22.44846404289852515, -74.05540946579084505, -31.87117065944173433 ) ) ;
#10923 = CARTESIAN_POINT ( 'NONE',  ( 15.65153732499999961, -101.3256027139999986, 2.837616081620000230 ) ) ;
#10924 = EDGE_CURVE ( 'NONE', #5668, #10427, #1086, .T. ) ;
#10925 = CARTESIAN_POINT ( 'NONE',  ( -10.92535406200000025, -42.25468912499999874, -20.74622789749999896 ) ) ;
#10926 = ORIENTED_EDGE ( 'NONE', *, *, #6640, .T. ) ;
#10927 = EDGE_CURVE ( 'NONE', #2868, #14159, #14709, .T. ) ;
#10928 = CARTESIAN_POINT ( 'NONE',  ( 22.16163108380142432, -57.47158985094319661, -7.992697376200416315 ) ) ;
#10929 = CARTESIAN_POINT ( 'NONE',  ( 12.39757656149999931, -101.1889999979999999, -10.11435096289999969 ) ) ;
#10930 = ORIENTED_EDGE ( 'NONE', *, *, #13277, .T. ) ;
#10931 = CARTESIAN_POINT ( 'NONE',  ( -17.00181101289999930, -93.27295844349998788, 19.70561590980000233 ) ) ;
#10932 = CARTESIAN_POINT ( 'NONE',  ( -42.56117883860000006, -65.49083508809999898, 0.5420286502529999551 ) ) ;
#10933 = CARTESIAN_POINT ( 'NONE',  ( 7.435983481019023955, -74.13941005068963364, 39.48497135292184623 ) ) ;
#10934 = AXIS2_PLACEMENT_3D ( 'NONE', #26879, #8784, #8933 ) ;
#10935 = CARTESIAN_POINT ( 'NONE',  ( 26.66586667100000341, -92.50000467790000869, 13.56662017419999877 ) ) ;
#10936 = CARTESIAN_POINT ( 'NONE',  ( 36.25000000000000000, -69.00000000000000000, 2.314797894279999601E-15 ) ) ;
#10937 = CARTESIAN_POINT ( 'NONE',  ( -42.25000000000000000, -65.63577453799999262, -0.7216878364880000563 ) ) ;
#10938 = CARTESIAN_POINT ( 'NONE',  ( 27.04769748009325880, -72.23842146203566017, -11.44023399195399371 ) ) ;
#10939 = DIRECTION ( 'NONE',  ( 1.000000000000000000, 0.000000000000000000, 0.000000000000000000 ) ) ;
#10940 = EDGE_LOOP ( 'NONE', ( #8339, #13940 ) ) ;
#10941 = DIRECTION ( 'NONE',  ( -0.000000000000000000, 1.000000000000000000, 0.000000000000000000 ) ) ;
#10942 = FACE_OUTER_BOUND ( 'NONE', #12870, .T. ) ;
#10943 = CARTESIAN_POINT ( 'NONE',  ( 8.825526648140000319, -98.73826279789999205, 16.36868468389999620 ) ) ;
#10944 = CARTESIAN_POINT ( 'NONE',  ( 23.15198552840000090, -19.16887642500000055, 1.371920395479999888 ) ) ;
#10945 = DIRECTION ( 'NONE',  ( 0.000000000000000000, 1.000000000000000000, 0.000000000000000000 ) ) ;
#10946 = CARTESIAN_POINT ( 'NONE',  ( -20.82481777699772607, -92.81370807121814437, -22.28401471726260041 ) ) ;
#10947 = CARTESIAN_POINT ( 'NONE',  ( -15.12459707010000010, -101.1499364180000100, 4.397920892620000188 ) ) ;
#10948 = CARTESIAN_POINT ( 'NONE',  ( 28.44483739272424216, -70.46285482980914594, 2.597167156265934640 ) ) ;
#10949 = CARTESIAN_POINT ( 'NONE',  ( -7.630334818519999729, -100.8023006570000035, 13.80849637110000039 ) ) ;
#10950 = EDGE_CURVE ( 'NONE', #5438, #1018, #13055, .T. ) ;
#10951 = CARTESIAN_POINT ( 'NONE',  ( 6.931585813929999951, -44.93330283539999925, -21.84994998139999822 ) ) ;
#10952 = DIRECTION ( 'NONE',  ( 0.000000000000000000, 1.000000000000000000, 0.000000000000000000 ) ) ;
#10953 = CARTESIAN_POINT ( 'NONE',  ( -12.73274366210000075, -67.57003242140000054, -23.00245288660000043 ) ) ;
#10954 = CARTESIAN_POINT ( 'NONE',  ( -38.25718401418472325, -65.12549727759254381, -2.739325690388396239 ) ) ;
#10955 = CARTESIAN_POINT ( 'NONE',  ( 24.75663061290020650, -93.31462968082412601, -12.91046299435144817 ) ) ;
#10956 = CARTESIAN_POINT ( 'NONE',  ( -10.27945668490000131, -18.50000000000000000, 18.70272521329999904 ) ) ;
#10957 = ORIENTED_EDGE ( 'NONE', *, *, #15825, .F. ) ;
#10958 = EDGE_CURVE ( 'NONE', #17392, #15244, #12659, .T. ) ;
#10959 = CARTESIAN_POINT ( 'NONE',  ( 8.857880004760000148, -18.86754460619999918, -19.35192615410000272 ) ) ;
#10960 = CARTESIAN_POINT ( 'NONE',  ( 22.49242817279999684, -37.98196143189999674, -9.212282262639998720 ) ) ;
#10961 = EDGE_LOOP ( 'NONE', ( #8758, #18202, #12679, #338 ) ) ;
#10962 = CARTESIAN_POINT ( 'NONE',  ( -12.71547034009999955, -65.00127802399998700, 21.72228991030000245 ) ) ;
#10963 = LINE ( 'NONE', #19873, #14071 ) ;
#10964 = CARTESIAN_POINT ( 'NONE',  ( 9.219197186969998015, -37.05706108660000098, -22.15413563950000153 ) ) ;
#10965 = CARTESIAN_POINT ( 'NONE',  ( -26.67277937040000069, -92.98481302140000082, -0.3354105345299999708 ) ) ;
#10966 = CARTESIAN_POINT ( 'NONE',  ( -19.63524818169999975, -57.47122622290000749, 13.01113544189999871 ) ) ;
#10967 = CARTESIAN_POINT ( 'NONE',  ( -20.19582590579999959, -52.57401960350014036, 14.62459034920000001 ) ) ;
#10968 = ORIENTED_EDGE ( 'NONE', *, *, #6337, .F. ) ;
#10969 = FILL_AREA_STYLE ('',( #260 ) ) ;
#10970 = CYLINDRICAL_SURFACE ( 'NONE', #8026, 0.1999999999999997891 ) ;
#10971 = EDGE_LOOP ( 'NONE', ( #23666, #17065, #21811, #1921 ) ) ;
#10972 = CYLINDRICAL_SURFACE ( 'NONE', #6614, 0.9999999999999988898 ) ;
#10973 = EDGE_LOOP ( 'NONE', ( #26541, #27363, #13744, #16126 ) ) ;
#10974 = CARTESIAN_POINT ( 'NONE',  ( -9.927741060089999792, -18.50000000000000000, -22.19465444469999937 ) ) ;
#10975 = CARTESIAN_POINT ( 'NONE',  ( -41.75000000000000000, -64.11445222650000630, -2.684678751739999925 ) ) ;
#10976 = ADVANCED_FACE ( 'NONE', ( #6260 ), #10464, .T. ) ;
#10977 = CARTESIAN_POINT ( 'NONE',  ( 20.49657866619999780, -57.47855601759999900, 11.20866246179999948 ) ) ;
#10978 = CARTESIAN_POINT ( 'NONE',  ( 8.782859991099998709, -69.73939502419999314, -25.82418225190000172 ) ) ;
#10979 = CARTESIAN_POINT ( 'NONE',  ( -14.79537251110000007, -100.9197086940000077, 5.022279785309999411 ) ) ;
#10980 = B_SPLINE_SURFACE_WITH_KNOTS ( 'NONE', 5, 5, ( 
 ( #5853, #21179, #16515, #21450, #18854, #18985 ),
 ( #25690, #14599, #23503, #1361, #8049, #16940 ),
 ( #22024, #19678, #1927, #1646, #24351, #12959 ),
 ( #10766, #11051, #6578, #21588, #28423, #6129 ),
 ( #3953, #15002, #15143, #28277, #15283, #23916 ),
 ( #24051, #12816, #15439, #26390, #17359, #21726 ),
 ( #1776, #19966, #10619, #4091, #19535, #8456 ),
 ( #28567, #10483, #19395, #12677, #26254, #17211 ),
 ( #4241, #26103, #6277, #21873, #8602, #17505 ) ),
 .UNSPECIFIED., .F., .F., .F.,
 ( 6, 3, 6 ),
 ( 6, 6 ),
 ( 41.71218049779999859, 49.83411874859999813, 53.81665561530000019 ),
 ( 0.000000000000000000, 2.000000000000000000 ),
 .UNSPECIFIED. ) ;
#10981 = VERTEX_POINT ( 'NONE', #14987 ) ;
#10982 = CARTESIAN_POINT ( 'NONE',  ( -15.40337430839999833, -101.5317003319999998, 4.643717924509999762 ) ) ;
#10983 = CARTESIAN_POINT ( 'NONE',  ( 26.79207366509999844, -72.75494331939999881, -10.16049586859999998 ) ) ;
#10984 = CARTESIAN_POINT ( 'NONE',  ( 8.185346967789998374, -101.3150701389999995, 14.03998109830000018 ) ) ;
#10985 = CARTESIAN_POINT ( 'NONE',  ( 9.385332722619999402, -98.68450614990000247, 16.47661810339999988 ) ) ;
#10986 = ORIENTED_EDGE ( 'NONE', *, *, #27899, .T. ) ;
#10987 = EDGE_CURVE ( 'NONE', #2039, #103, #28258, .T. ) ;
#10988 = CARTESIAN_POINT ( 'NONE',  ( -0.7724858235186301547, -101.6484611540000031, -15.98142581210590762 ) ) ;
#10989 = CARTESIAN_POINT ( 'NONE',  ( -13.09441083470000144, -92.84549618469999643, -23.96915825600000005 ) ) ;
#10990 = EDGE_LOOP ( 'NONE', ( #18172, #13350, #3566, #9966 ) ) ;
#10991 = DIRECTION ( 'NONE',  ( 0.000000000000000000, 1.000000000000000000, 0.000000000000000000 ) ) ;
#10992 = LINE ( 'NONE', #16267, #23331 ) ;
#10993 = CARTESIAN_POINT ( 'NONE',  ( -5.884306709680000580, -101.1461869959999973, 15.04985507670000011 ) ) ;
#10994 = CARTESIAN_POINT ( 'NONE',  ( -22.62871152338947311, -80.00000000056968474, -32.48908675062602924 ) ) ;
#10995 = ORIENTED_EDGE ( 'NONE', *, *, #17035, .T. ) ;
#10996 = B_SPLINE_CURVE_WITH_KNOTS ( 'NONE', 3,
 ( #18308, #16102, #24717, #11730, #13777, #20644 ),
 .UNSPECIFIED., .F., .F.,
 ( 4, 2, 4 ),
 ( 0.000000000000000000, 0.5000000000000000000, 1.000000000000000000 ),
 .UNSPECIFIED. ) ;
#10997 = CYLINDRICAL_SURFACE ( 'NONE', #5802, 3.000000000000001332 ) ;
#10998 = ORIENTED_EDGE ( 'NONE', *, *, #938, .F. ) ;
#10999 = CARTESIAN_POINT ( 'NONE',  ( 21.07836655800000258, -93.85715932649999615, 13.25903705600000038 ) ) ;
#11000 = CARTESIAN_POINT ( 'NONE',  ( 46.22668039279999874, -73.89966597549998539, -4.016967337520000569 ) ) ;
#11001 = ORIENTED_EDGE ( 'NONE', *, *, #25951, .T. ) ;
#11002 = CARTESIAN_POINT ( 'NONE',  ( -41.78603200349471791, -65.71742637283956867, 1.321057898033102029 ) ) ;
#11003 = CARTESIAN_POINT ( 'NONE',  ( -22.29269500190000386, -94.98812477769999418, -8.065858985560000249 ) ) ;
#11004 = AXIS2_PLACEMENT_3D ( 'NONE', #28041, #3706, #12568 ) ;
#11005 = CARTESIAN_POINT ( 'NONE',  ( 12.29187919760000014, -101.1617736559999940, -9.834676144290000366 ) ) ;
#11006 = DIRECTION ( 'NONE',  ( 0.000000000000000000, -1.000000000000000000, 0.000000000000000000 ) ) ;
#11007 = CARTESIAN_POINT ( 'NONE',  ( 0.000000000000000000, -90.50000000000000000, 0.000000000000000000 ) ) ;
#11008 = ORIENTED_EDGE ( 'NONE', *, *, #23610, .F. ) ;
#11009 = ADVANCED_FACE ( 'NONE', ( #12939 ), #9842, .T. ) ;
#11010 = CARTESIAN_POINT ( 'NONE',  ( -1.449832362199999780, -100.8733988930000010, -15.65780151839999945 ) ) ;
#11011 = EDGE_CURVE ( 'NONE', #10810, #17507, #19141, .T. ) ;
#11012 = DIRECTION ( 'NONE',  ( 0.3687499999999813705, 0.000000000000000000, -0.9295286103719528903 ) ) ;
#11013 = CARTESIAN_POINT ( 'NONE',  ( 0.000000000000000000, -2.000000000000000000, 0.000000000000000000 ) ) ;
#11014 = CARTESIAN_POINT ( 'NONE',  ( -2.489779910060000212, -56.21886023140000077, -24.59145677380000095 ) ) ;
#11015 = DIRECTION ( 'NONE',  ( 1.000000000000000000, 0.000000000000000000, 0.000000000000000000 ) ) ;
#11016 = EDGE_CURVE ( 'NONE', #17262, #10454, #16920, .T. ) ;
#11017 = DIRECTION ( 'NONE',  ( 0.000000000000000000, 1.000000000000000000, 0.000000000000000000 ) ) ;
#11018 = CARTESIAN_POINT ( 'NONE',  ( -19.02205191440000220, -19.48534420260000033, 13.96959728589999905 ) ) ;
#11019 = VERTEX_POINT ( 'NONE', #24927 ) ;
#11020 = CARTESIAN_POINT ( 'NONE',  ( -15.95377854864229050, -18.50000000000000000, 21.99697738415282799 ) ) ;
#11021 = CARTESIAN_POINT ( 'NONE',  ( -7.105427357599999217E-15, -101.6484611540000031, -1.598721155459999804E-14 ) ) ;
#11022 = DIRECTION ( 'NONE',  ( -0.5715342875219319163, 0.000000000000000000, -0.8205781852979018298 ) ) ;
#11023 = FACE_OUTER_BOUND ( 'NONE', #6068, .T. ) ;
#11024 = CARTESIAN_POINT ( 'NONE',  ( 0.1200718050890000055, -91.50000000000000000, -30.49976365090000030 ) ) ;
#11025 = AXIS2_PLACEMENT_3D ( 'NONE', #617, #16161, #5101 ) ;
#11026 = APPLICATION_PROTOCOL_DEFINITION ( 'draft international standard', 'automotive_design', 1998, #8834 ) ;
#11027 = CARTESIAN_POINT ( 'NONE',  ( 0.000000000000000000, -29.89689110870000022, 0.000000000000000000 ) ) ;
#11028 = CARTESIAN_POINT ( 'NONE',  ( -11.64049356306891347, -94.65527814842015175, -20.66310145454055558 ) ) ;
#11029 = VERTEX_POINT ( 'NONE', #22291 ) ;
#11030 = EDGE_CURVE ( 'NONE', #23088, #17197, #15887, .T. ) ;
#11031 = CARTESIAN_POINT ( 'NONE',  ( 22.04471494010000043, -95.70830610080000156, -4.438274023730000017 ) ) ;
#11032 = ORIENTED_EDGE ( 'NONE', *, *, #14361, .F. ) ;
#11033 = AXIS2_PLACEMENT_3D ( 'NONE', #21992, #17622, #2041 ) ;
#11034 = DIRECTION ( 'NONE',  ( 0.000000000000000000, -1.000000000000000000, 0.000000000000000000 ) ) ;
#11035 = DIRECTION ( 'NONE',  ( 0.4794255386042040601, 0.000000000000000000, 0.8775825618903720926 ) ) ;
#11036 = ORIENTED_EDGE ( 'NONE', *, *, #24810, .T. ) ;
#11037 = DIRECTION ( 'NONE',  ( 0.000000000000000000, -1.000000000000000000, 0.000000000000000000 ) ) ;
#11038 = CARTESIAN_POINT ( 'NONE',  ( -41.75000000000000000, -63.00000000000000000, 1.587713240270000048 ) ) ;
#11039 = B_SPLINE_SURFACE_WITH_KNOTS ( 'NONE', 5, 5, ( 
 ( #9657, #14190, #6908, #24682, #16514, #25689 ),
 ( #16649, #28147, #9800, #25543, #23086, #20897 ),
 ( #5581, #14466, #17068, #10346, #7776, #19259 ),
 ( #25830, #5852, #25962, #3672, #10208, #19122 ),
 ( #23359, #1232, #5986, #25411, #23220, #7912 ),
 ( #12269, #23633, #18853, #21449, #16797, #14734 ) ),
 .UNSPECIFIED., .F., .F., .F.,
 ( 6, 6 ),
 ( 6, 6 ),
 ( 7.179431122970000523, 23.44689954309999891 ),
 ( 0.000000000000000000, 0.5000000000000000000 ),
 .UNSPECIFIED. ) ;
#11040 = ORIENTED_EDGE ( 'NONE', *, *, #565, .T. ) ;
#11041 = CARTESIAN_POINT ( 'NONE',  ( -11.23277242420000022, -95.05245081340000013, -21.31917440760000204 ) ) ;
#11042 = CARTESIAN_POINT ( 'NONE',  ( 1.342713516450000144, -94.57749834670001121, 24.16140173950000047 ) ) ;
#11043 = DIRECTION ( 'NONE',  ( 1.000000000000000000, 0.000000000000000000, 0.000000000000000000 ) ) ;
#11044 = CARTESIAN_POINT ( 'NONE',  ( -29.45136854416018224, -92.49999999999997158, 7.930057420454290629 ) ) ;
#11045 = CARTESIAN_POINT ( 'NONE',  ( 22.17953377930000158, -65.07443093669999712, 11.85657293289999892 ) ) ;
#11046 = VERTEX_POINT ( 'NONE', #26821 ) ;
#11047 = CIRCLE ( 'NONE', #28750, 18.14285714289999873 ) ;
#11048 = CARTESIAN_POINT ( 'NONE',  ( 6.717799458580000049, -84.50000000000000000, 40.65853658540000026 ) ) ;
#11049 = EDGE_CURVE ( 'NONE', #7605, #9894, #18213, .T. ) ;
#11050 = CARTESIAN_POINT ( 'NONE',  ( 24.20832872070000263, -49.83808240369999254, 1.215820334740000064 ) ) ;
#11051 = CARTESIAN_POINT ( 'NONE',  ( 25.49852039510000168, -69.13896873969999035, 10.91553851559999977 ) ) ;
#11052 = CARTESIAN_POINT ( 'NONE',  ( -13.27471559884043728, -92.83865970264245959, 27.45964197909431093 ) ) ;
#11053 = ORIENTED_EDGE ( 'NONE', *, *, #5975, .T. ) ;
#11054 = CARTESIAN_POINT ( 'NONE',  ( -12.84659744679999882, -72.82938648530000592, -25.64625568420000334 ) ) ;
#11055 = CARTESIAN_POINT ( 'NONE',  ( -13.54698799950000065, -92.84291960289999679, 27.17977165490000147 ) ) ;
#11056 = CARTESIAN_POINT ( 'NONE',  ( -14.34373124439999891, -102.5000000000000000, -26.25602392650000283 ) ) ;
#11057 = VERTEX_POINT ( 'NONE', #15575 ) ;
#11058 = CARTESIAN_POINT ( 'NONE',  ( 11.70455088819999823, -92.50000000000000000, 8.942783294160001617 ) ) ;
#11059 = AXIS2_PLACEMENT_3D ( 'NONE', #8710, #6396, #11345 ) ;
#11060 = CARTESIAN_POINT ( 'NONE',  ( 0.2405919600229999844, -101.0678230150000019, -15.82154074309999991 ) ) ;
#11061 = DIRECTION ( 'NONE',  ( 1.291895883199999965E-15, -0.000000000000000000, 1.000000000000000000 ) ) ;
#11062 = CARTESIAN_POINT ( 'NONE',  ( 15.17121247040000043, -101.1411470150000014, 2.586268237070000087 ) ) ;
#11063 = CARTESIAN_POINT ( 'NONE',  ( -11.67870342830000041, -57.47571039179999985, -20.30949892389999789 ) ) ;
#11064 = CARTESIAN_POINT ( 'NONE',  ( 22.26662627820000040, -57.47855601759999900, -7.066909182079999852 ) ) ;
#11065 = CIRCLE ( 'NONE', #11558, 25.14975229270000057 ) ;
#11066 = EDGE_LOOP ( 'NONE', ( #12483, #3043, #23489, #7004 ) ) ;
#11067 = CARTESIAN_POINT ( 'NONE',  ( 28.34932843007601377, -92.75430643202088277, 11.25025375756242951 ) ) ;
#11068 = CARTESIAN_POINT ( 'NONE',  ( -43.16155280139999917, -65.17124718639999514, 0.1954025812279999996 ) ) ;
#11069 = CIRCLE ( 'NONE', #11578, 7.249999999999999112 ) ;
#11070 = CARTESIAN_POINT ( 'NONE',  ( -2.903043064769999848, -94.98812477769999418, 23.52859639729999941 ) ) ;
#11071 = ORIENTED_EDGE ( 'NONE', *, *, #21964, .F. ) ;
#11072 = CARTESIAN_POINT ( 'NONE',  ( 7.196178079599999222, -73.81415926540000783, 38.70548889989999708 ) ) ;
#11073 = CARTESIAN_POINT ( 'NONE',  ( 20.51117185680000077, -93.49005502510000554, 16.28046590780000002 ) ) ;
#11074 = ADVANCED_FACE ( 'NONE', ( #24478 ), #24627, .F. ) ;
#11075 = CARTESIAN_POINT ( 'NONE',  ( -10.20110288159999890, -80.00000000000000000, 41.00000000000000000 ) ) ;
#11076 = CARTESIAN_POINT ( 'NONE',  ( 22.29295329801293235, -19.46656432701744777, 0.4976463741603174284 ) ) ;
#11077 = CARTESIAN_POINT ( 'NONE',  ( -6.842500939620000722, -101.1402801299999936, 13.72981480590000025 ) ) ;
#11078 = ORIENTED_EDGE ( 'NONE', *, *, #22231, .T. ) ;
#11079 = CARTESIAN_POINT ( 'NONE',  ( 0.000000000000000000, -84.00000000000000000, 0.000000000000000000 ) ) ;
#11080 = CARTESIAN_POINT ( 'NONE',  ( -12.88540406179054187, -100.4166221067027323, -11.03975155362831551 ) ) ;
#11081 = ORIENTED_EDGE ( 'NONE', *, *, #26858, .F. ) ;
#11082 = CARTESIAN_POINT ( 'NONE',  ( 9.203357703080000007, -35.92863931600000171, -19.97610107710000094 ) ) ;
#11083 = EDGE_CURVE ( 'NONE', #16955, #19768, #18702, .T. ) ;
#11084 = CARTESIAN_POINT ( 'NONE',  ( 21.43169449828233653, -35.31509369946678589, -7.132046020603563186 ) ) ;
#11085 = CARTESIAN_POINT ( 'NONE',  ( -6.665307709260000379, -93.00000000000000000, -13.13558364449999871 ) ) ;
#11086 = CARTESIAN_POINT ( 'NONE',  ( -12.16664950528991440, -19.47159289567763096, 19.15110637680422201 ) ) ;
#11087 = CARTESIAN_POINT ( 'NONE',  ( -7.593123957489999576, -94.98812477769999418, -22.45811603920000010 ) ) ;
#11088 = VECTOR ( 'NONE', #22354, 1000.000000000000000 ) ;
#11089 = CARTESIAN_POINT ( 'NONE',  ( 14.03681164164373563, -92.52048598158043546, 27.07800181827376207 ) ) ;
#11090 = VERTEX_POINT ( 'NONE', #2642 ) ;
#11091 = CARTESIAN_POINT ( 'NONE',  ( -14.76791303109999909, -100.9938288390000025, 4.803350814669999913 ) ) ;
#11092 = CARTESIAN_POINT ( 'NONE',  ( -14.40572000550000098, -18.50000000000000000, 20.06574520719999910 ) ) ;
#11093 = CARTESIAN_POINT ( 'NONE',  ( 16.28649422715901451, -94.66088193484175406, 17.22963786743054371 ) ) ;
#11094 = CIRCLE ( 'NONE', #13924, 0.4999999999999985567 ) ;
#11095 = CONICAL_SURFACE ( 'NONE', #9737, 25.14975229270001833, 0.4276056667390000787 ) ;
#11096 = AXIS2_PLACEMENT_3D ( 'NONE', #24149, #8827, #11310 ) ;
#11097 = FACE_OUTER_BOUND ( 'NONE', #4343, .T. ) ;
#11098 = CIRCLE ( 'NONE', #27443, 19.50000000000000000 ) ;
#11099 = CARTESIAN_POINT ( 'NONE',  ( 0.000000000000000000, -22.69689110870000093, 0.000000000000000000 ) ) ;
#11100 = CARTESIAN_POINT ( 'NONE',  ( 26.13951773519340094, -63.17363326945925195, 1.458190918673929248 ) ) ;
#11101 = CARTESIAN_POINT ( 'NONE',  ( -38.42216747628722828, -65.10234783419650739, -2.883361208460165859 ) ) ;
#11102 = DIRECTION ( 'NONE',  ( 0.000000000000000000, 1.000000000000000000, 0.000000000000000000 ) ) ;
#11103 = CARTESIAN_POINT ( 'NONE',  ( 25.11232611503765710, -93.38817447853173803, 11.60437395511254266 ) ) ;
#11104 = ORIENTED_EDGE ( 'NONE', *, *, #28406, .T. ) ;
#11105 = CARTESIAN_POINT ( 'NONE',  ( 8.076031017920000110, -18.85700242990000319, -20.35668352559999761 ) ) ;
#11106 = ORIENTED_EDGE ( 'NONE', *, *, #18170, .F. ) ;
#11107 = CARTESIAN_POINT ( 'NONE',  ( -11.79670204130000144, -63.63842289929999652, 21.46815698109999815 ) ) ;
#11108 = CARTESIAN_POINT ( 'NONE',  ( -18.69985100922852084, -92.84292036730930420, 22.78328761814548997 ) ) ;
#11109 = CARTESIAN_POINT ( 'NONE',  ( -27.15805213390000006, -93.30149055180000062, -0.5667321042260000663 ) ) ;
#11110 = EDGE_CURVE ( 'NONE', #25354, #26232, #4287, .T. ) ;
#11111 = CARTESIAN_POINT ( 'NONE',  ( -19.79577514300000018, -57.47815920199999340, 12.40824665329999910 ) ) ;
#11112 = DIRECTION ( 'NONE',  ( 0.000000000000000000, 1.000000000000000000, 0.000000000000000000 ) ) ;
#11114 = EDGE_CURVE ( 'NONE', #3774, #28309, #7296, .T. ) ;
#11113 = AXIS2_PLACEMENT_3D ( 'NONE', #6192, #28482, #8518 ) ;
#11115 = VECTOR ( 'NONE', #1158, 1000.000000000000000 ) ;
#11116 = CARTESIAN_POINT ( 'NONE',  ( -11.90992159604306622, -57.47815920418752711, -20.09952900877129878 ) ) ;
#11117 = ORIENTED_EDGE ( 'NONE', *, *, #23244, .F. ) ;
#11118 = FACE_OUTER_BOUND ( 'NONE', #16601, .T. ) ;
#11119 = CARTESIAN_POINT ( 'NONE',  ( 0.000000000000000000, -65.07443093669999712, 0.000000000000000000 ) ) ;
#11120 = CARTESIAN_POINT ( 'NONE',  ( -13.25045755180000029, -101.1889999979999999, -10.32789304109999939 ) ) ;
#11121 = ORIENTED_EDGE ( 'NONE', *, *, #806, .F. ) ;
#11122 = EDGE_CURVE ( 'NONE', #20659, #22866, #14138, .T. ) ;
#11123 = CARTESIAN_POINT ( 'NONE',  ( 6.981684465299999864, -111.0000000000000000, 29.03810821740000137 ) ) ;
#11124 = B_SPLINE_CURVE_WITH_KNOTS ( 'NONE', 5,
 ( #27638, #25578, #8080, #7679, #16545, #5610 ),
 .UNSPECIFIED., .F., .F.,
 ( 6, 6 ),
 ( 0.000000000000000000, 1.000000000000000000 ),
 .UNSPECIFIED. ) ;
#11125 = EDGE_CURVE ( 'NONE', #19131, #24445, #14028, .T. ) ;
#11126 = VERTEX_POINT ( 'NONE', #765 ) ;
#11127 = CARTESIAN_POINT ( 'NONE',  ( -24.64364036189999752, -92.50000000000000000, -17.97055897050000084 ) ) ;
#11128 = CARTESIAN_POINT ( 'NONE',  ( 20.12528277150000022, -32.73099401700000044, 10.22949540999999840 ) ) ;
#11129 = DIRECTION ( 'NONE',  ( 0.000000000000000000, 1.000000000000000000, 0.000000000000000000 ) ) ;
#11130 = CARTESIAN_POINT ( 'NONE',  ( 24.27280310300000110, -92.97898997910000674, -11.25989722030000095 ) ) ;
#11131 = CARTESIAN_POINT ( 'NONE',  ( 18.75935060549999989, -18.50000000000000000, 10.17575150659999927 ) ) ;
#11132 = CARTESIAN_POINT ( 'NONE',  ( -32.64751318483137510, -80.00000000000000000, -22.65605297795088191 ) ) ;
#11133 = CARTESIAN_POINT ( 'NONE',  ( 14.17788327750000121, -97.64874574789999429, -14.06651099139999950 ) ) ;
#11134 = ORIENTED_EDGE ( 'NONE', *, *, #15260, .F. ) ;
#11135 = CARTESIAN_POINT ( 'NONE',  ( -27.68682485439999752, -28.69999999999999929, -50.68039294919999804 ) ) ;
#11136 = CARTESIAN_POINT ( 'NONE',  ( 9.008529550149999565, -24.55588640339999884, -19.11129932280000077 ) ) ;
#11137 = CARTESIAN_POINT ( 'NONE',  ( -12.60239484230000073, -99.94549701829998867, -11.26274910859999956 ) ) ;
#11138 = CARTESIAN_POINT ( 'NONE',  ( 21.61954412840861295, -19.48585536712340271, 9.522048220035644661 ) ) ;
#11139 = CIRCLE ( 'NONE', #14869, 55.50192378860000275 ) ;
#11140 = CARTESIAN_POINT ( 'NONE',  ( 11.90927564517308745, -97.32634609770845202, 16.96552214579065776 ) ) ;
#11141 = ORIENTED_EDGE ( 'NONE', *, *, #12445, .T. ) ;
#11142 = AXIS2_PLACEMENT_3D ( 'NONE', #10294, #7858, #8257 ) ;
#11143 = AXIS2_PLACEMENT_3D ( 'NONE', #21233, #10126, #7967 ) ;
#11144 = DIRECTION ( 'NONE',  ( 0.000000000000000000, 1.000000000000000000, 0.000000000000000000 ) ) ;
#11145 = ORIENTED_EDGE ( 'NONE', *, *, #20622, .T. ) ;
#11146 = B_SPLINE_CURVE_WITH_KNOTS ( 'NONE', 5,
 ( #6225, #4182, #2159, #15228, #10994, #19907 ),
 .UNSPECIFIED., .F., .F.,
 ( 6, 6 ),
 ( 0.000000000000000000, 1.000000000000000000 ),
 .UNSPECIFIED. ) ;
#11147 = FACE_OUTER_BOUND ( 'NONE', #23037, .T. ) ;
#11148 = DIRECTION ( 'NONE',  ( 0.4794255386042036715, 0.000000000000000000, 0.8775825618903723147 ) ) ;
#11149 = CARTESIAN_POINT ( 'NONE',  ( -5.145566427369999474, -99.82967635509999127, 17.17619540129999933 ) ) ;
#11150 = CARTESIAN_POINT ( 'NONE',  ( -17.84952165019772607, -94.52419090328167783, 16.07137172613918707 ) ) ;
#11151 = ORIENTED_EDGE ( 'NONE', *, *, #10151, .T. ) ;
#11152 = EDGE_CURVE ( 'NONE', #25473, #11263, #14278, .T. ) ;
#11153 = DIRECTION ( 'NONE',  ( 1.000000000000000000, 0.000000000000000000, 0.000000000000000000 ) ) ;
#11154 = VERTEX_POINT ( 'NONE', #18663 ) ;
#11155 = CARTESIAN_POINT ( 'NONE',  ( -26.02252412820971017, -93.99439547200873335, -2.045450153116517900 ) ) ;
#11156 = CARTESIAN_POINT ( 'NONE',  ( 19.64032065480000000, -94.52419443349998573, 13.82578161140000006 ) ) ;
#11157 = CARTESIAN_POINT ( 'NONE',  ( 46.57616008939999830, -73.79912698820000116, -3.102537739159999752 ) ) ;
#11158 = ORIENTED_EDGE ( 'NONE', *, *, #27939, .T. ) ;
#11159 = AXIS2_PLACEMENT_3D ( 'NONE', #23027, #3078, #20838 ) ;
#11160 = FACE_OUTER_BOUND ( 'NONE', #27702, .T. ) ;
#11161 = CARTESIAN_POINT ( 'NONE',  ( -24.72072344461773952, -93.86980009075321618, -6.303046593384079799 ) ) ;
#11162 = CIRCLE ( 'NONE', #7003, 9.099999999999999645 ) ;
#11163 = EDGE_CURVE ( 'NONE', #14989, #11899, #558, .T. ) ;
#11164 = AXIS2_PLACEMENT_3D ( 'NONE', #420, #8976, #17883 ) ;
#11165 = ORIENTED_EDGE ( 'NONE', *, *, #6343, .F. ) ;
#11166 = CARTESIAN_POINT ( 'NONE',  ( 8.556786983500000332, -37.95394734039999918, -21.84310845219999919 ) ) ;
#11167 = CARTESIAN_POINT ( 'NONE',  ( -13.28804895260000052, -94.06807348040000250, -21.53763003719999958 ) ) ;
#11168 = DIRECTION ( 'NONE',  ( 1.000000000000000000, 0.000000000000000000, 0.000000000000000000 ) ) ;
#11169 = VERTEX_POINT ( 'NONE', #25779 ) ;
#11170 = CARTESIAN_POINT ( 'NONE',  ( 0.000000000000000000, -101.2530993010000060, 0.000000000000000000 ) ) ;
#11171 = CARTESIAN_POINT ( 'NONE',  ( -17.05934341600000081, -99.58396357329999660, 3.231284207160000310 ) ) ;
#11172 = DIRECTION ( 'NONE',  ( 0.2414462220490750377, 0.000000000000000000, 0.9704142011833034598 ) ) ;
#11173 = CARTESIAN_POINT ( 'NONE',  ( 0.1200718050890000055, -111.0000000000000000, -30.49976365090000030 ) ) ;
#11174 = CARTESIAN_POINT ( 'NONE',  ( -5.719111655694421259, -98.21781671762684596, -19.46371341358546658 ) ) ;
#11175 = DIRECTION ( 'NONE',  ( 0.000000000000000000, -1.000000000000000000, 0.000000000000000000 ) ) ;
#11176 = CARTESIAN_POINT ( 'NONE',  ( -13.46276276179999876, -19.49999999970000175, 20.39865906480000035 ) ) ;
#11177 = CARTESIAN_POINT ( 'NONE',  ( 7.600490370247736216, -74.00013394018854740, -38.79561088320171791 ) ) ;
#11178 = ORIENTED_EDGE ( 'NONE', *, *, #12743, .F. ) ;
#11179 = CARTESIAN_POINT ( 'NONE',  ( -9.671059929650001052, -94.07042739149999022, -23.11466436250000100 ) ) ;
#11180 = CARTESIAN_POINT ( 'NONE',  ( 7.675802467110550253, -57.47600031385420039, -22.13628273390180468 ) ) ;
#11181 = DIRECTION ( 'NONE',  ( 1.000000000000000000, 0.000000000000000000, 0.000000000000000000 ) ) ;
#11182 = DIRECTION ( 'NONE',  ( 0.000000000000000000, 1.000000000000000000, 0.000000000000000000 ) ) ;
#11183 = CIRCLE ( 'NONE', #21009, 3.749999999999996447 ) ;
#11184 = B_SPLINE_CURVE_WITH_KNOTS ( 'NONE', 3,
 ( #27410, #18812, #16027, #7741, #11800, #11942 ),
 .UNSPECIFIED., .F., .F.,
 ( 4, 2, 4 ),
 ( 0.000000000000000000, 0.5000000000000000000, 1.000000000000000000 ),
 .UNSPECIFIED. ) ;
#11185 = CIRCLE ( 'NONE', #14481, 29.91857981989999971 ) ;
#11186 = VECTOR ( 'NONE', #963, 1000.000000000000114 ) ;
#11187 = UNCERTAINTY_MEASURE_WITH_UNIT (LENGTH_MEASURE( 1.000000000000000082E-05 ), #6355, 'distance_accuracy_value', 'NONE');
#11188 = DIRECTION ( 'NONE',  ( 1.000000000000000000, 0.000000000000000000, 0.000000000000000000 ) ) ;
#11189 = CARTESIAN_POINT ( 'NONE',  ( 24.71478484869999903, -57.43018266680000039, 1.313252026010000018 ) ) ;
#11190 = AXIS2_PLACEMENT_3D ( 'NONE', #11288, #11129, #13479 ) ;
#11191 = CARTESIAN_POINT ( 'NONE',  ( -11.77049175740000209, -94.59276292389999696, -20.68200892780000189 ) ) ;
#11192 = ORIENTED_EDGE ( 'NONE', *, *, #22711, .F. ) ;
#11193 = EDGE_CURVE ( 'NONE', #726, #21723, #17746, .T. ) ;
#11194 = CARTESIAN_POINT ( 'NONE',  ( 19.09127226800000088, -98.29702512280000803, -0.7133363862450000648 ) ) ;
#11195 = EDGE_LOOP ( 'NONE', ( #14789, #12062 ) ) ;
#11196 = CARTESIAN_POINT ( 'NONE',  ( 34.89999999999999858, -86.00000000000000000, 4.273876174839999917E-15 ) ) ;
#11197 = LINE ( 'NONE', #22898, #6511 ) ;
#11198 = ORIENTED_EDGE ( 'NONE', *, *, #21421, .F. ) ;
#11199 = CARTESIAN_POINT ( 'NONE',  ( -40.00000000000000000, -69.50000000000000000, -8.881784197000000993E-16 ) ) ;
#11200 = EDGE_CURVE ( 'NONE', #12661, #9424, #20068, .T. ) ;
#11201 = CARTESIAN_POINT ( 'NONE',  ( -11.31661412480000095, -95.23933631519999210, -21.36055902369999870 ) ) ;
#11202 = CARTESIAN_POINT ( 'NONE',  ( 7.804759209956171340, -94.00303307110470996, -24.89030770455894270 ) ) ;
#11203 = CARTESIAN_POINT ( 'NONE',  ( 0.000000000000000000, -39.50000000000000000, 0.000000000000000000 ) ) ;
#11204 = CARTESIAN_POINT ( 'NONE',  ( -41.75000000000000000, -63.07912966450000880, 2.684678751729999480 ) ) ;
#11205 = FACE_OUTER_BOUND ( 'NONE', #20327, .T. ) ;
#11206 = AXIS2_PLACEMENT_3D ( 'NONE', #11056, #2662, #42 ) ;
#11207 = CARTESIAN_POINT ( 'NONE',  ( 12.05743353869999979, -65.07443093669999712, 22.07098404789999790 ) ) ;
#11208 = ORIENTED_EDGE ( 'NONE', *, *, #4036, .T. ) ;
#11209 = AXIS2_PLACEMENT_3D ( 'NONE', #15536, #13351, #11153 ) ;
#11210 = DIRECTION ( 'NONE',  ( -0.5301416321220548955, 0.000000000000000000, -0.8479091047340887588 ) ) ;
#11211 = AXIS2_PLACEMENT_3D ( 'NONE', #11586, #8970, #26776 ) ;
#11212 = CARTESIAN_POINT ( 'NONE',  ( -20.50880539726380292, -61.98877831146614170, 12.53749828487332252 ) ) ;
#11213 = CARTESIAN_POINT ( 'NONE',  ( 40.52471374997017506, -74.35734738321731641, 7.233314584394662461 ) ) ;
#11214 = ORIENTED_EDGE ( 'NONE', *, *, #7754, .F. ) ;
#11215 = CYLINDRICAL_SURFACE ( 'NONE', #17385, 2.999999999999998668 ) ;
#11216 = CARTESIAN_POINT ( 'NONE',  ( -16.76064802440000179, -92.85978345570001125, 21.58520938940000278 ) ) ;
#11217 = DIRECTION ( 'NONE',  ( 1.000000000000000000, 0.000000000000000000, 0.000000000000000000 ) ) ;
#11218 = ORIENTED_EDGE ( 'NONE', *, *, #3466, .F. ) ;
#11219 = CARTESIAN_POINT ( 'NONE',  ( 27.45110624719999848, -70.13570072960000346, 0.6191059290799999504 ) ) ;
#11220 = B_SPLINE_CURVE_WITH_KNOTS ( 'NONE', 5,
 ( #28339, #10967, #15199, #13174, #21649, #22085, #12735, #1698, #19451 ),
 .UNSPECIFIED., .F., .F.,
 ( 6, 3, 6 ),
 ( 0.000000000000000000, 0.5000000000000000000, 1.000000000000000000 ),
 .UNSPECIFIED. ) ;
#11221 = CARTESIAN_POINT ( 'NONE',  ( -12.57512233279243574, -101.1416252791420476, -9.133129954655776928 ) ) ;
#11222 = EDGE_CURVE ( 'NONE', #15463, #5258, #19553, .T. ) ;
#11223 = CARTESIAN_POINT ( 'NONE',  ( 0.9302366604389999960, -100.4808658609999981, -16.19480876779999790 ) ) ;
#11224 = CARTESIAN_POINT ( 'NONE',  ( 2.876553231629999985, -91.50000000000000000, 5.265495371340000119 ) ) ;
#11225 = LINE ( 'NONE', #11822, #18230 ) ;
#11226 = CARTESIAN_POINT ( 'NONE',  ( -11.34636246480000032, -49.86909869750000013, -20.35003598449999984 ) ) ;
#11227 = CARTESIAN_POINT ( 'NONE',  ( 22.33353861310135358, -57.45905989834243144, -8.600015579560372103 ) ) ;
#11228 = DIRECTION ( 'NONE',  ( 0.2162432783070565578, 0.000000000000000000, 0.9763395129702663322 ) ) ;
#11229 = CIRCLE ( 'NONE', #3362, 61.35000000000000142 ) ;
#11230 = CIRCLE ( 'NONE', #19623, 0.5000000000000027756 ) ;
#11231 = ORIENTED_EDGE ( 'NONE', *, *, #17942, .T. ) ;
#11232 = EDGE_CURVE ( 'NONE', #4093, #22777, #23045, .T. ) ;
#11233 = CARTESIAN_POINT ( 'NONE',  ( -39.73574291596239760, -65.71452780515839720, -2.210925124798794883 ) ) ;
#11234 = CARTESIAN_POINT ( 'NONE',  ( 14.95019707169999990, -101.2530993000000024, 2.710463435110000319 ) ) ;
#11235 = B_SPLINE_CURVE_WITH_KNOTS ( 'NONE', 3,
 ( #18402, #16348, #20882, #27290 ),
 .UNSPECIFIED., .F., .F.,
 ( 4, 4 ),
 ( -19.56549066489999689, -15.82800233080000041 ),
 .UNSPECIFIED. ) ;
#11236 = CARTESIAN_POINT ( 'NONE',  ( 14.95034095350000136, -97.23151611000000116, 15.27375035569999895 ) ) ;
#11237 = ORIENTED_EDGE ( 'NONE', *, *, #8370, .T. ) ;
#11238 = CARTESIAN_POINT ( 'NONE',  ( 23.52525244343676647, -92.58347372263170882, -19.41166030436781043 ) ) ;
#11239 = CARTESIAN_POINT ( 'NONE',  ( 22.57257117529999846, -92.75885938649999218, 15.68540759639999749 ) ) ;
#11240 = B_SPLINE_SURFACE_WITH_KNOTS ( 'NONE', 5, 5, ( 
 ( #28163, #8196, #17083, #26117, #25976, #6000, #12282, #23931, #14881 ),
 ( #1660, #23790, #16662, #5595, #7926, #3828, #1243, #25557, #12691 ),
 ( #14476, #10082, #27879, #22479, #24659, #28709, #6433, #26849, #4692 ),
 ( #8615, #6290, #26701, #22038, #10925, #19549, #2086, #19831, #21888 ),
 ( #13570, #10779, #8896, #15606, #15296, #11226, #13272, #20132, #22181 ),
 ( #15156, #8748, #17665, #2521, #17810, #202, #11063, #26549, #28437 ) ),
 .UNSPECIFIED., .F., .F., .F.,
 ( 6, 6 ),
 ( 6, 3, 6 ),
 ( 15.94303934740000095, 69.72897805050000386 ),
 ( 0.000000000000000000, 1.000000000000000000, 2.000000000000000000 ),
 .UNSPECIFIED. ) ;
#11241 = CARTESIAN_POINT ( 'NONE',  ( 23.51796030652247893, -19.48482983503955168, 1.427212532244023668 ) ) ;
#11242 = CARTESIAN_POINT ( 'NONE',  ( -7.423820152569999387, -100.9678331089999972, 14.37793136710000041 ) ) ;
#11243 = VERTEX_POINT ( 'NONE', #28368 ) ;
#11244 = CARTESIAN_POINT ( 'NONE',  ( 27.09220507755102858, -72.19826629891751679, -11.51208668783220013 ) ) ;
#11245 = ORIENTED_EDGE ( 'NONE', *, *, #17406, .T. ) ;
#11246 = CARTESIAN_POINT ( 'NONE',  ( 8.435862578959998359, -36.92586548770000121, -21.49743428369999521 ) ) ;
#11247 = CARTESIAN_POINT ( 'NONE',  ( -26.89647983300000078, -10.52212389379999991, -49.23367609159999603 ) ) ;
#11248 = ORIENTED_EDGE ( 'NONE', *, *, #28731, .F. ) ;
#11249 = CARTESIAN_POINT ( 'NONE',  ( 19.69582338720000081, -18.50000000000000000, -7.383548592259999488 ) ) ;
#11250 = LINE ( 'NONE', #5001, #559 ) ;
#11251 = DIRECTION ( 'NONE',  ( 0.000000000000000000, 1.000000000000000000, 0.000000000000000000 ) ) ;
#11252 = DIRECTION ( 'NONE',  ( 0.000000000000000000, 1.000000000000000000, 0.000000000000000000 ) ) ;
#11253 = CARTESIAN_POINT ( 'NONE',  ( -15.21246199350000161, -100.9405350259999921, 4.776674228709999248 ) ) ;
#11254 = CIRCLE ( 'NONE', #22927, 13.00000000000000178 ) ;
#11255 = CARTESIAN_POINT ( 'NONE',  ( -14.10948125060000002, -18.50000000000000000, 20.17033318009999832 ) ) ;
#11256 = CARTESIAN_POINT ( 'NONE',  ( 13.20594032278986774, -96.16332745752187350, 17.30516087073727505 ) ) ;
#11257 = CARTESIAN_POINT ( 'NONE',  ( -36.73717667715042978, -65.11500191527956360, 0.1170746919412273407 ) ) ;
#11258 = ADVANCED_FACE ( 'NONE', ( #24744 ), #15833, .T. ) ;
#11259 = CARTESIAN_POINT ( 'NONE',  ( 36.61022179955299549, -75.00000020938335865, -14.75000000000000178 ) ) ;
#11260 = DIRECTION ( 'NONE',  ( 0.000000000000000000, -1.000000000000000000, 0.000000000000000000 ) ) ;
#11261 = DIRECTION ( 'NONE',  ( 1.000000000000000000, 0.000000000000000000, 0.000000000000000000 ) ) ;
#11262 = CARTESIAN_POINT ( 'NONE',  ( -10.42741367090000004, -18.61794786490000320, 18.97192220850000055 ) ) ;
#11263 = VERTEX_POINT ( 'NONE', #6523 ) ;
#11264 = CARTESIAN_POINT ( 'NONE',  ( -32.20769383860636026, -80.36910031991209280, -22.43272069095936416 ) ) ;
#11265 = ADVANCED_FACE ( 'NONE', ( #18178 ), #17283, .T. ) ;
#11266 = ORIENTED_EDGE ( 'NONE', *, *, #14787, .F. ) ;
#11267 = CARTESIAN_POINT ( 'NONE',  ( -13.76017623309999927, -64.69849637139999743, 21.59184277249999795 ) ) ;
#11268 = CARTESIAN_POINT ( 'NONE',  ( -12.30235599149999892, -63.58904326009999153, 21.23101024950000237 ) ) ;
#11269 = CARTESIAN_POINT ( 'NONE',  ( 7.243843118859103924, -74.18716007600167472, 40.29875214202166944 ) ) ;
#11270 = AXIS2_PLACEMENT_3D ( 'NONE', #16531, #5459, #27884 ) ;
#11271 = VECTOR ( 'NONE', #14284, 1000.000000000000000 ) ;
#11272 = B_SPLINE_CURVE_WITH_KNOTS ( 'NONE', 3,
 ( #5322, #16813, #7664, #27624 ),
 .UNSPECIFIED., .F., .F.,
 ( 4, 4 ),
 ( 0.000000000000000000, 1.000000000000000000 ),
 .UNSPECIFIED. ) ;
#11273 = CARTESIAN_POINT ( 'NONE',  ( 0.000000000000000000, -108.5000000000000000, 0.000000000000000000 ) ) ;
#11274 = AXIS2_PLACEMENT_3D ( 'NONE', #10720, #19083, #21267 ) ;
#11275 = DIRECTION ( 'NONE',  ( 1.000000000000000000, 0.000000000000000000, 0.000000000000000000 ) ) ;
#11276 = CARTESIAN_POINT ( 'NONE',  ( 19.96273463004390081, -19.47964434323706939, -8.629719000944380269 ) ) ;
#11277 = CARTESIAN_POINT ( 'NONE',  ( -11.46863496920000003, -57.40875702469999453, -22.62382260909999943 ) ) ;
#11278 = ORIENTED_EDGE ( 'NONE', *, *, #130, .T. ) ;
#11279 = CARTESIAN_POINT ( 'NONE',  ( -7.250133233359999707, -73.75841684550000821, -39.12193274490000050 ) ) ;
#11280 =( LENGTH_UNIT ( ) NAMED_UNIT ( * ) SI_UNIT ( .MILLI., .METRE. ) );
#11281 = CARTESIAN_POINT ( 'NONE',  ( -19.66462998450000299, -97.01506441399999403, -6.707659482730000455 ) ) ;
#11282 = ORIENTED_EDGE ( 'NONE', *, *, #18136, .F. ) ;
#11283 = CARTESIAN_POINT ( 'NONE',  ( -30.47783378272416854, -92.54687141712493315, 1.162627035193506853 ) ) ;
#11284 = DIRECTION ( 'NONE',  ( 0.000000000000000000, 1.000000000000000000, 0.000000000000000000 ) ) ;
#11285 = CARTESIAN_POINT ( 'NONE',  ( 7.215414233289999757, -84.00000000000000000, -40.70731707320000226 ) ) ;
#11286 = CIRCLE ( 'NONE', #11781, 1.250000000000000000 ) ;
#11287 = CARTESIAN_POINT ( 'NONE',  ( 20.29473261270000251, -45.99930305829999355, 10.74246239310000028 ) ) ;
#11288 = CARTESIAN_POINT ( 'NONE',  ( 0.000000000000000000, -37.57799544290000426, 0.000000000000000000 ) ) ;
#11289 = CARTESIAN_POINT ( 'NONE',  ( 22.85992316819999814, -94.54719310899999130, -6.820851015779999749 ) ) ;
#11290 = CARTESIAN_POINT ( 'NONE',  ( -13.93619502189999970, -74.00000000010000178, 36.24163866030000491 ) ) ;
#11291 = CARTESIAN_POINT ( 'NONE',  ( 10.39238870299999995, -67.58693996879999588, -25.45267030080000126 ) ) ;
#11292 = CARTESIAN_POINT ( 'NONE',  ( 14.06911839400000019, -98.73889367950000917, -12.22485475130000054 ) ) ;
#11293 = ORIENTED_EDGE ( 'NONE', *, *, #4317, .F. ) ;
#11294 = AXIS2_PLACEMENT_3D ( 'NONE', #18628, #15840, #1020 ) ;
#11295 = DIRECTION ( 'NONE',  ( 0.000000000000000000, 1.000000000000000000, 0.000000000000000000 ) ) ;
#11296 = CARTESIAN_POINT ( 'NONE',  ( 38.08875739639999836, -84.00000000000000000, 9.476764215410000247 ) ) ;
#11297 = CARTESIAN_POINT ( 'NONE',  ( -12.90942923769999950, -100.2522625769999962, -11.08739780120000162 ) ) ;
#11298 = PRODUCT_DEFINITION ( 'UNKNOWN', '', #4566, #15567 ) ;
#11299 = CIRCLE ( 'NONE', #28061, 4.750000000000000888 ) ;
#11300 = DIRECTION ( 'NONE',  ( 1.000000000000000000, 0.000000000000000000, 0.000000000000000000 ) ) ;
#11301 = CARTESIAN_POINT ( 'NONE',  ( 22.76002593507040928, -61.37679267133752603, -7.241526953473480965 ) ) ;
#11302 = EDGE_LOOP ( 'NONE', ( #8630, #17375 ) ) ;
#11303 = EDGE_CURVE ( 'NONE', #18665, #26232, #24443, .T. ) ;
#11304 = CARTESIAN_POINT ( 'NONE',  ( -38.25000000000000000, -63.00000000000000000, -1.587713240270000048 ) ) ;
#11305 = ORIENTED_EDGE ( 'NONE', *, *, #10551, .T. ) ;
#11306 = EDGE_CURVE ( 'NONE', #22763, #2020, #88, .T. ) ;
#11307 = EDGE_CURVE ( 'NONE', #8189, #26635, #16357, .T. ) ;
#11308 = CARTESIAN_POINT ( 'NONE',  ( 0.000000000000000000, -2.000000000000000000, 0.000000000000000000 ) ) ;
#11309 = VECTOR ( 'NONE', #12681, 1000.000000000000114 ) ;
#11310 = DIRECTION ( 'NONE',  ( 0.3064653112860303286, -0.9430444279530931784, -0.1294071863730131000 ) ) ;
#11311 = CARTESIAN_POINT ( 'NONE',  ( 12.03509228579999935, -92.84019744260001517, 27.58265792150000095 ) ) ;
#11312 = VERTEX_POINT ( 'NONE', #21967 ) ;
#11313 = ORIENTED_EDGE ( 'NONE', *, *, #27972, .F. ) ;
#11314 = DIRECTION ( 'NONE',  ( 0.000000000000000000, -1.000000000000000000, 0.000000000000000000 ) ) ;
#11315 = CARTESIAN_POINT ( 'NONE',  ( 20.33590001279999981, -94.16310024840001347, 13.51329393089999975 ) ) ;
#11316 = DIRECTION ( 'NONE',  ( 0.000000000000000000, 1.000000000000000000, 0.000000000000000000 ) ) ;
#11317 = ORIENTED_EDGE ( 'NONE', *, *, #2949, .F. ) ;
#11318 = CIRCLE ( 'NONE', #20656, 1.499999999999999556 ) ;
#11319 = CARTESIAN_POINT ( 'NONE',  ( -42.06841198963231676, -65.70763704137388572, 0.8557820958490719443 ) ) ;
#11320 = CARTESIAN_POINT ( 'NONE',  ( -21.99312410279999952, -80.25114227570000480, -32.51123870579999675 ) ) ;
#11321 = CARTESIAN_POINT ( 'NONE',  ( 8.655529603599999788, -36.72098037409999449, -21.58808908319999986 ) ) ;
#11322 = CARTESIAN_POINT ( 'NONE',  ( 0.000000000000000000, -17.50000000000000000, 0.000000000000000000 ) ) ;
#11323 = CARTESIAN_POINT ( 'NONE',  ( -23.85440626824976107, -94.57749869815765464, -4.067369308893817426 ) ) ;
#11324 = ORIENTED_EDGE ( 'NONE', *, *, #7382, .F. ) ;
#11325 = CARTESIAN_POINT ( 'NONE',  ( 6.981684465299999864, -93.00000000000000000, 29.03810821740000137 ) ) ;
#11326 = CIRCLE ( 'NONE', #19715, 5.000000000000000888 ) ;
#11327 = CARTESIAN_POINT ( 'NONE',  ( 13.88148934900000064, -99.91102932019998661, -9.687780287520000755 ) ) ;
#11328 = CARTESIAN_POINT ( 'NONE',  ( -40.30304758909999663, -74.34471143260000758, 7.255215663249999558 ) ) ;
#11329 = DIRECTION ( 'NONE',  ( 0.8775825618903722036, 0.000000000000000000, -0.4794255386042041156 ) ) ;
#11330 = CARTESIAN_POINT ( 'NONE',  ( -1.981473163410000016, -57.45864773929999814, -23.83876219520000106 ) ) ;
#11331 = AXIS2_PLACEMENT_3D ( 'NONE', #14501, #23960, #7950 ) ;
#11332 = CARTESIAN_POINT ( 'NONE',  ( 0.000000000000000000, -84.75000000000000000, 0.000000000000000000 ) ) ;
#11333 = CARTESIAN_POINT ( 'NONE',  ( -7.489111472456650098, -73.99989317614092954, 38.95197877120744323 ) ) ;
#11334 = CARTESIAN_POINT ( 'NONE',  ( 25.26718046270000073, -19.50000000000000000, 6.129403842640000377 ) ) ;
#11335 = ORIENTED_EDGE ( 'NONE', *, *, #18906, .F. ) ;
#11336 = EDGE_CURVE ( 'NONE', #25460, #3543, #23396, .T. ) ;
#11337 = CARTESIAN_POINT ( 'NONE',  ( 6.831813925109999630, -13.50000000000000000, 12.50555150689999984 ) ) ;
#11338 = CARTESIAN_POINT ( 'NONE',  ( 22.29272167939999960, -65.04696937989999128, 11.61829170020000035 ) ) ;
#11339 = CARTESIAN_POINT ( 'NONE',  ( 8.987515397540001061, -35.19375992660000207, -19.46719241160000280 ) ) ;
#11340 = CARTESIAN_POINT ( 'NONE',  ( -24.20176002190990516, -92.56772982775143532, -18.56148008688876416 ) ) ;
#11341 = CARTESIAN_POINT ( 'NONE',  ( 4.794255386040000566, -54.00000000000000000, 8.775825618900000791 ) ) ;
#11342 = CARTESIAN_POINT ( 'NONE',  ( 46.47110230210000026, -80.14094940709999548, -3.615576172169999936 ) ) ;
#11343 = AXIS2_PLACEMENT_3D ( 'NONE', #24652, #23060, #5128 ) ;
#11344 = EDGE_CURVE ( 'NONE', #11758, #19059, #20616, .T. ) ;
#11345 = DIRECTION ( 'NONE',  ( 1.000000000000000000, 0.000000000000000000, 0.000000000000000000 ) ) ;
#11346 = CARTESIAN_POINT ( 'NONE',  ( -11.81933340930000043, -64.47176828549999072, -23.20996066840000083 ) ) ;
#11347 = CARTESIAN_POINT ( 'NONE',  ( -40.00000000000000000, -69.00000000000000000, -9.436895709309999441E-17 ) ) ;
#11348 = ORIENTED_EDGE ( 'NONE', *, *, #7699, .F. ) ;
#11349 = CARTESIAN_POINT ( 'NONE',  ( 17.45802118700000349, -99.55619081819999394, 0.9170739917250000373 ) ) ;
#11350 = ORIENTED_EDGE ( 'NONE', *, *, #15006, .T. ) ;
#11351 = CARTESIAN_POINT ( 'NONE',  ( -11.85013948020000107, -42.26697439500000542, 19.76414738429999929 ) ) ;
#11352 = CARTESIAN_POINT ( 'NONE',  ( -2.903039748510000351, -94.98812477769999418, 23.52859306979999943 ) ) ;
#11353 = ORIENTED_EDGE ( 'NONE', *, *, #2410, .F. ) ;
#11354 = CARTESIAN_POINT ( 'NONE',  ( 9.165580245683250027, -36.00000000019999646, -20.59810122320078918 ) ) ;
#11355 = CARTESIAN_POINT ( 'NONE',  ( 3.631617597942636166, -93.11247489620001261, -28.67783563263252589 ) ) ;
#11356 = DIRECTION ( 'NONE',  ( 0.000000000000000000, 1.000000000000000000, 0.000000000000000000 ) ) ;
#11357 = CARTESIAN_POINT ( 'NONE',  ( 25.94817478915412323, -70.08538442660875489, -8.904232401822897103 ) ) ;
#11358 = CIRCLE ( 'NONE', #10877, 7.250000000000000000 ) ;
#11359 = CARTESIAN_POINT ( 'NONE',  ( -10.17458377400000025, -18.50000000000000000, -22.50859265919999785 ) ) ;
#11360 = CARTESIAN_POINT ( 'NONE',  ( 21.52064452127972416, -37.42737532315320692, -7.718013524113811918 ) ) ;
#11361 = ORIENTED_EDGE ( 'NONE', *, *, #9170, .F. ) ;
#11362 = DIRECTION ( 'NONE',  ( 1.000000000000000000, 0.000000000000000000, 0.000000000000000000 ) ) ;
#11363 = CARTESIAN_POINT ( 'NONE',  ( -38.23463116603283396, -65.69529750896734299, -1.411076260621699330 ) ) ;
#11364 = CARTESIAN_POINT ( 'NONE',  ( -13.31491859036868775, -92.89593097429161617, 27.44017123060003627 ) ) ;
#11365 = ORIENTED_EDGE ( 'NONE', *, *, #19241, .T. ) ;
#11366 = AXIS2_PLACEMENT_3D ( 'NONE', #21226, #25602, #14513 ) ;
#11367 = CARTESIAN_POINT ( 'NONE',  ( 19.69582338720000081, -18.50000000000000000, -7.383548592259999488 ) ) ;
#11368 = CARTESIAN_POINT ( 'NONE',  ( -17.05574026919999753, -93.34713166629998682, 21.78488634390000200 ) ) ;
#11369 = CARTESIAN_POINT ( 'NONE',  ( -14.19188855770000046, -80.00000000000000000, 37.13021410070000883 ) ) ;
#11370 = ORIENTED_EDGE ( 'NONE', *, *, #18031, .T. ) ;
#11371 = EDGE_CURVE ( 'NONE', #5907, #17770, #16778, .T. ) ;
#11372 = CARTESIAN_POINT ( 'NONE',  ( -16.22299306009999853, -99.56341898720000927, 6.708263584790000067 ) ) ;
#11373 = VECTOR ( 'NONE', #25123, 1000.000000000000000 ) ;
#11374 = CARTESIAN_POINT ( 'NONE',  ( 0.6180977789570000214, -100.8746138070000029, -16.59152119279999837 ) ) ;
#11375 = CARTESIAN_POINT ( 'NONE',  ( 23.94732912799409164, -74.14839568665851743, -30.91612537757790946 ) ) ;
#11376 = DIRECTION ( 'NONE',  ( 0.4794255386042041156, 0.000000000000000000, 0.8775825618903720926 ) ) ;
#11377 = CARTESIAN_POINT ( 'NONE',  ( 0.000000000000000000, -26.90310889129999694, 0.000000000000000000 ) ) ;
#11378 = ADVANCED_FACE ( 'NONE', ( #19043 ), #3789, .T. ) ;
#11379 = DIRECTION ( 'NONE',  ( 0.000000000000000000, 1.000000000000000000, 0.000000000000000000 ) ) ;
#11380 = ORIENTED_EDGE ( 'NONE', *, *, #23181, .F. ) ;
#11381 = CARTESIAN_POINT ( 'NONE',  ( -15.60988350939999947, -92.64731536089999508, 23.37060113569999942 ) ) ;
#11382 = DIRECTION ( 'NONE',  ( 0.000000000000000000, -1.000000000000000000, 0.000000000000000000 ) ) ;
#11383 = VECTOR ( 'NONE', #2784, 1000.000000000000000 ) ;
#11384 = LINE ( 'NONE', #6895, #5136 ) ;
#11385 = ORIENTED_EDGE ( 'NONE', *, *, #24381, .T. ) ;
#11386 = CARTESIAN_POINT ( 'NONE',  ( 7.314390784529999578, -73.97626148509999666, 39.54176628510000313 ) ) ;
#11387 = CARTESIAN_POINT ( 'NONE',  ( -18.84946550835717005, -97.93129752234466423, 6.692286737796515617 ) ) ;
#11388 = B_SPLINE_CURVE_WITH_KNOTS ( 'NONE', 5,
 ( #14411, #21123, #9601, #18653, #2922, #25212, #14540, #11785, #25489 ),
 .UNSPECIFIED., .F., .F.,
 ( 6, 3, 6 ),
 ( 0.000000000000000000, 0.5000000000000000000, 1.000000000000000000 ),
 .UNSPECIFIED. ) ;
#11389 = CARTESIAN_POINT ( 'NONE',  ( 11.31179088046036441, -98.73470581857429806, -14.63453564218954739 ) ) ;
#11390 = CARTESIAN_POINT ( 'NONE',  ( -7.341283001269998998, -101.1412505549999992, 14.40471526709999850 ) ) ;
#11391 = VERTEX_POINT ( 'NONE', #1699 ) ;
#11392 = AXIS2_PLACEMENT_3D ( 'NONE', #21496, #21637, #23965 ) ;
#11393 = CARTESIAN_POINT ( 'NONE',  ( 27.02127222293052711, -72.26362179314627099, -11.39336057284735659 ) ) ;
#11394 = CARTESIAN_POINT ( 'NONE',  ( 8.981104793960000165, -36.05511643379999498, -20.59303662420000336 ) ) ;
#11395 = CARTESIAN_POINT ( 'NONE',  ( 45.84677420395677672, -73.65707963207451314, -4.286925635858382932 ) ) ;
#11396 = CARTESIAN_POINT ( 'NONE',  ( 7.560313589829999792, -99.58327329889999646, 15.94543460589999739 ) ) ;
#11397 = CARTESIAN_POINT ( 'NONE',  ( 3.166345171159999694, -93.00000000000000000, -25.30265318609999881 ) ) ;
#11398 = CARTESIAN_POINT ( 'NONE',  ( -3.841450593410000280, -96.73974214389998849, -20.89652819670000028 ) ) ;
#11399 = CARTESIAN_POINT ( 'NONE',  ( -2.552536252342168410, -19.48522775728675072, -23.44697642559193085 ) ) ;
#11400 = ORIENTED_EDGE ( 'NONE', *, *, #6076, .T. ) ;
#11401 = CARTESIAN_POINT ( 'NONE',  ( -14.79537254420000103, -100.9197086940000077, 5.022279801499999863 ) ) ;
#11402 = DIRECTION ( 'NONE',  ( 0.4794255386042040046, 0.000000000000000000, 0.8775825618903722036 ) ) ;
#11403 = EDGE_CURVE ( 'NONE', #7122, #24982, #23351, .T. ) ;
#11404 = EDGE_CURVE ( 'NONE', #15395, #3254, #23797, .T. ) ;
#11405 = CARTESIAN_POINT ( 'NONE',  ( 0.000000000000000000, -10.50000000000000000, 0.000000000000000000 ) ) ;
#11406 = AXIS2_PLACEMENT_3D ( 'NONE', #15431, #481, #22160 ) ;
#11407 = CARTESIAN_POINT ( 'NONE',  ( -12.37736070569999924, -67.43115654220000010, -23.30866868589999896 ) ) ;
#11408 = CARTESIAN_POINT ( 'NONE',  ( 24.71840331404647628, -93.41743724424139828, -12.20012907774811062 ) ) ;
#11409 = CARTESIAN_POINT ( 'NONE',  ( 29.52540673129999860, -93.00000000000000000, 7.168153169610000930 ) ) ;
#11410 = ORIENTED_EDGE ( 'NONE', *, *, #18709, .F. ) ;
#11411 = CARTESIAN_POINT ( 'NONE',  ( -32.25191193603353668, -80.23900669782145201, -22.46351872105675440 ) ) ;
#11412 = CARTESIAN_POINT ( 'NONE',  ( 8.085424419389999784, -101.4206919209999853, 14.00535675889999965 ) ) ;
#11413 = AXIS2_PLACEMENT_3D ( 'NONE', #23124, #23405, #3445 ) ;
#11414 = DIRECTION ( 'NONE',  ( 0.000000000000000000, 1.000000000000000000, 0.000000000000000000 ) ) ;
#11415 = CARTESIAN_POINT ( 'NONE',  ( -12.32689411409999991, -62.06831188909999497, 20.76176652019999835 ) ) ;
#11416 = DIRECTION ( 'NONE',  ( 0.000000000000000000, 1.000000000000000000, 0.000000000000000000 ) ) ;
#11417 = CARTESIAN_POINT ( 'NONE',  ( 20.06309763089999620, -36.00000000000000000, -9.476129751679998492 ) ) ;
#11418 = CARTESIAN_POINT ( 'NONE',  ( 21.20403895319999776, -36.23955850830000003, -8.971066259000000542 ) ) ;
#11419 = CARTESIAN_POINT ( 'NONE',  ( 6.015370493379999656E-15, -69.50000000000000000, -40.00000000000000000 ) ) ;
#11420 = EDGE_CURVE ( 'NONE', #3267, #452, #1176, .T. ) ;
#11421 = CARTESIAN_POINT ( 'NONE',  ( 46.25000000000000000, -75.00000000000000000, -7.375000000000000000 ) ) ;
#11422 = VERTEX_POINT ( 'NONE', #6338 ) ;
#11423 = CARTESIAN_POINT ( 'NONE',  ( -7.252015964940000003, -74.29298176469998793, -40.34085930499999506 ) ) ;
#11424 = CARTESIAN_POINT ( 'NONE',  ( 29.28445555986126791, -74.32986215128055107, -26.08911349325367723 ) ) ;
#11425 = CARTESIAN_POINT ( 'NONE',  ( -17.51014701730000311, -98.29702512480000109, -7.640698720650000553 ) ) ;
#11426 = ORIENTED_EDGE ( 'NONE', *, *, #6622, .F. ) ;
#11427 = CARTESIAN_POINT ( 'NONE',  ( -30.47866716000020659, -92.54383083955178790, 1.140710722936425281 ) ) ;
#11428 = CARTESIAN_POINT ( 'NONE',  ( -17.00715350810000004, -99.92967601899998442, 3.484608414699999823 ) ) ;
#11429 = CARTESIAN_POINT ( 'NONE',  ( -17.00715350810000004, -101.1889999979999999, 3.484608414699999823 ) ) ;
#11430 = DIRECTION ( 'NONE',  ( 0.000000000000000000, -1.000000000000000000, 0.000000000000000000 ) ) ;
#11431 = TOROIDAL_SURFACE ( 'NONE', #25431, 3.750000000000000000, 1.000000000000000000 ) ;
#11432 = CARTESIAN_POINT ( 'NONE',  ( 0.000000000000000000, -15.49689110870000164, 0.000000000000000000 ) ) ;
#11433 = CARTESIAN_POINT ( 'NONE',  ( 12.77500156440000012, -93.00000000000000000, 27.05403395929999988 ) ) ;
#11434 = CARTESIAN_POINT ( 'NONE',  ( 19.84950935299999841, -19.15770089200000115, 9.820435146359999479 ) ) ;
#11435 = CARTESIAN_POINT ( 'NONE',  ( 10.35051949290000017, -65.80242602599999202, -25.33509568779999910 ) ) ;
#11436 = CARTESIAN_POINT ( 'NONE',  ( -15.18759500087176306, -100.4790389224915401, 5.637615933027189108 ) ) ;
#11437 = VERTEX_POINT ( 'NONE', #15501 ) ;
#11438 = DIRECTION ( 'NONE',  ( 0.000000000000000000, 1.000000000000000000, 0.000000000000000000 ) ) ;
#11439 = CARTESIAN_POINT ( 'NONE',  ( -5.119737544835406773, -100.1470170834167419, 17.03205665007207159 ) ) ;
#11440 = APPLICATION_CONTEXT ( 'automotive_design' ) ;
#11441 = DIRECTION ( 'NONE',  ( 1.000000000000000000, 0.000000000000000000, 0.000000000000000000 ) ) ;
#11442 = CARTESIAN_POINT ( 'NONE',  ( 23.30839594958685268, -63.38792371584848695, -7.455862079869596926 ) ) ;
#11443 = EDGE_LOOP ( 'NONE', ( #21941, #10857, #324, #16398 ) ) ;
#11444 = CARTESIAN_POINT ( 'NONE',  ( -37.36725231429999639, -69.50000000000000000, 1.438276615809999992 ) ) ;
#11445 = ORIENTED_EDGE ( 'NONE', *, *, #23047, .F. ) ;
#11446 = B_SPLINE_CURVE_WITH_KNOTS ( 'NONE', 3,
 ( #19818, #28696, #22167, #8736, #2207, #26534, #17653, #8885, #26688, #6729 ),
 .UNSPECIFIED., .F., .F.,
 ( 4, 2, 2, 2, 4 ),
 ( 0.000000000000000000, 0.2500000000000000000, 0.5000000000000000000, 0.7500000000000000000, 1.000000000000000000 ),
 .UNSPECIFIED. ) ;
#11447 = CARTESIAN_POINT ( 'NONE',  ( -10.80933341492661448, -19.49660160594845948, -21.71230118854520796 ) ) ;
#11448 = CARTESIAN_POINT ( 'NONE',  ( -41.00000000000000000, -74.50000000000000000, 10.20110288159999890 ) ) ;
#11449 = CARTESIAN_POINT ( 'NONE',  ( -4.056245258659999742, -98.60488091210000050, 19.31197723180000025 ) ) ;
#11450 = CARTESIAN_POINT ( 'NONE',  ( 7.994999523870000679, -92.89940159850000612, 27.27230444749999805 ) ) ;
#11451 = EDGE_LOOP ( 'NONE', ( #3788, #1929, #25409, #18933 ) ) ;
#11452 = EDGE_CURVE ( 'NONE', #3127, #27117, #2407, .T. ) ;
#11453 = ORIENTED_EDGE ( 'NONE', *, *, #26379, .F. ) ;
#11454 = CYLINDRICAL_SURFACE ( 'NONE', #5589, 9.500000000000001776 ) ;
#11455 = CARTESIAN_POINT ( 'NONE',  ( -13.02626867543477829, -71.94658701398387279, -25.10627575233144171 ) ) ;
#11456 = CARTESIAN_POINT ( 'NONE',  ( 10.55611696420000101, -36.00000000000000000, -20.94239052940000079 ) ) ;
#11457 = VERTEX_POINT ( 'NONE', #4447 ) ;
#11458 = CARTESIAN_POINT ( 'NONE',  ( 7.239953483535906287, -73.75061506092028196, -39.61603006814522843 ) ) ;
#11459 = CARTESIAN_POINT ( 'NONE',  ( -22.13232311830000043, -79.50000004279999644, -32.73892520679999762 ) ) ;
#11460 = EDGE_CURVE ( 'NONE', #26414, #2354, #22408, .T. ) ;
#11461 = B_SPLINE_CURVE_WITH_KNOTS ( 'NONE', 3,
 ( #19583, #17412, #19308, #28054, #17115, #24103, #10525, #21923, #21353, #8357, #1410, #10255, #17259, #10818, #6326, #4140, #24398, #15637, #11408, #16080, #380, #26741, #7070, #10955, #22073, #28746, #18283, #24537, #6776, #27173, #4291, #17844, #27028, #7211, #9378, #13457, #20308 ),
 .UNSPECIFIED., .F., .F.,
 ( 4, 2, 2, 1, 1, 1, 2, 2, 2, 2, 1, 1, 1, 2, 2, 2, 2, 1, 1, 1, 2, 2, 4 ),
 ( 0.000000000000000000, 0.1250000000000197065, 0.1875000000000296707, 0.2187500000000343614, 0.2343750000000362488, 0.2421875000000367484, 0.2460937500000368872, 0.2500000000000370259, 0.3750000000000243694, 0.4375000000000178746, 0.4687500000000144329, 0.4843750000000129896, 0.4921875000000123235, 0.4960937500000122125, 0.5000000000000121014, 0.6250000000000108802, 0.6875000000000104361, 0.7187500000000101030, 0.7343750000000097700, 0.7421875000000094369, 0.7460937500000092149, 0.7500000000000091038, 1.000000000000000000 ),
 .UNSPECIFIED. ) ;
#11462 = CARTESIAN_POINT ( 'NONE',  ( 12.32527298249999959, -101.3256027139999986, -10.05536332369999997 ) ) ;
#11463 = ADVANCED_FACE ( 'NONE', ( #24116 ), #13556, .F. ) ;
#11464 = CARTESIAN_POINT ( 'NONE',  ( -12.47731372630000024, -94.18458606750000683, -20.89673554119999821 ) ) ;
#11465 = CARTESIAN_POINT ( 'NONE',  ( -39.50000000000000000, -65.00000000000000000, -2.309401076760000393 ) ) ;
#11466 = ORIENTED_EDGE ( 'NONE', *, *, #8004, .T. ) ;
#11467 = EDGE_CURVE ( 'NONE', #22328, #16026, #9829, .T. ) ;
#11468 = CARTESIAN_POINT ( 'NONE',  ( 36.32677412860000032, -74.12275851199999011, -14.57143996970000011 ) ) ;
#11469 = CARTESIAN_POINT ( 'NONE',  ( -2.595652345209999989, -59.96629798200000039, -25.39846653560000078 ) ) ;
#11470 = CARTESIAN_POINT ( 'NONE',  ( -40.35962647450000418, -74.26791556530000094, 7.250123090889999844 ) ) ;
#11471 = CARTESIAN_POINT ( 'NONE',  ( -21.74262969930000011, -74.09723562380000317, -32.46276855370000192 ) ) ;
#11472 = ORIENTED_EDGE ( 'NONE', *, *, #12195, .T. ) ;
#11473 = CARTESIAN_POINT ( 'NONE',  ( 27.19594722837873491, -66.52176723538890712, 1.775342338193904856 ) ) ;
#11474 = CARTESIAN_POINT ( 'NONE',  ( -7.371519361690793026, -73.99966369223987783, 39.28661307825520055 ) ) ;
#11475 = CARTESIAN_POINT ( 'NONE',  ( -18.92688961970000250, -18.86472494539999900, 14.06132894319999949 ) ) ;
#11476 = ORIENTED_EDGE ( 'NONE', *, *, #8390, .F. ) ;
#11477 = CARTESIAN_POINT ( 'NONE',  ( 0.000000000000000000, -102.8486084350000027, 0.000000000000000000 ) ) ;
#11478 = CARTESIAN_POINT ( 'NONE',  ( 23.92242908059999706, -63.31646347429999366, 10.69554000200000132 ) ) ;
#11479 = CARTESIAN_POINT ( 'NONE',  ( 7.969906462720000029, -35.15970427070000426, -21.19871012420000156 ) ) ;
#11480 = CARTESIAN_POINT ( 'NONE',  ( 16.13476677959289418, -100.7538407667569658, 4.305120634646285360 ) ) ;
#11481 = DIRECTION ( 'NONE',  ( 0.4794255386042040601, 0.000000000000000000, 0.8775825618903720926 ) ) ;
#11482 = ORIENTED_EDGE ( 'NONE', *, *, #13926, .T. ) ;
#11483 = CARTESIAN_POINT ( 'NONE',  ( 45.84677419350000349, -80.34292036729999609, -4.286925650119999709 ) ) ;
#11484 = B_SPLINE_SURFACE_WITH_KNOTS ( 'NONE', 5, 5, ( 
 ( #19013, #28303, #3702, #28174, #10237, #12564 ),
 ( #19151, #8337, #1670, #17097, #17242, #26134 ),
 ( #6157, #21203, #1126, #7801, #27892, #16826 ),
 ( #14629, #23528, #19992, #21900, #4265, #28723 ),
 ( #26714, #65, #8485, #13286, #10793, #8911 ),
 ( #8761, #26417, #15311, #6303, #26563, #13138 ) ),
 .UNSPECIFIED., .F., .F., .F.,
 ( 6, 6 ),
 ( 6, 6 ),
 ( 43.40831274110000493, 64.87293781390000902 ),
 ( 0.000000000000000000, 2.000000000000000000 ),
 .UNSPECIFIED. ) ;
#11485 = CARTESIAN_POINT ( 'NONE',  ( -11.53845963589999890, -61.97075362790000241, -21.57078944089999695 ) ) ;
#11486 = CARTESIAN_POINT ( 'NONE',  ( 26.27227914920000273, -70.89666188759998988, -10.69275250369999952 ) ) ;
#11487 = FACE_OUTER_BOUND ( 'NONE', #1194, .T. ) ;
#11488 = ORIENTED_EDGE ( 'NONE', *, *, #2247, .T. ) ;
#11489 = AXIS2_PLACEMENT_3D ( 'NONE', #22193, #20149, #13289 ) ;
#11490 = CARTESIAN_POINT ( 'NONE',  ( -14.65665286289999969, -74.50000000000000000, 36.94583910070000599 ) ) ;
#11491 = CARTESIAN_POINT ( 'NONE',  ( -41.75000000000000000, -65.19264941160000149, -2.595760183529999932 ) ) ;
#11492 = ORIENTED_EDGE ( 'NONE', *, *, #4237, .F. ) ;
#11493 = CARTESIAN_POINT ( 'NONE',  ( -13.91350890449018962, -18.60777309624396381, 20.23952179938335050 ) ) ;
#11494 = CARTESIAN_POINT ( 'NONE',  ( 9.385332722619999402, -98.68450614990000247, 16.47661810339999988 ) ) ;
#11495 = ORIENTED_EDGE ( 'NONE', *, *, #28319, .F. ) ;
#11496 = FACE_OUTER_BOUND ( 'NONE', #17677, .T. ) ;
#11497 = CARTESIAN_POINT ( 'NONE',  ( 41.00000000000000000, -84.50000000000000000, 10.20110288159999890 ) ) ;
#11498 = EDGE_CURVE ( 'NONE', #7420, #5746, #10733, .T. ) ;
#11499 = AXIS2_PLACEMENT_3D ( 'NONE', #22070, #2119, #529 ) ;
#11500 = CARTESIAN_POINT ( 'NONE',  ( 7.834729293268852146, -94.01603309712585599, -24.85338230034197693 ) ) ;
#11501 = CARTESIAN_POINT ( 'NONE',  ( -28.46472064010000125, -92.56290624670000966, 3.501361395690000045 ) ) ;
#11502 = CARTESIAN_POINT ( 'NONE',  ( -20.03691699049999997, -95.66927305889998934, 10.25834442809999913 ) ) ;
#11503 = EDGE_CURVE ( 'NONE', #3189, #2845, #5331, .T. ) ;
#11504 = CARTESIAN_POINT ( 'NONE',  ( -10.65197422049999965, -18.62337009750000050, -22.10007990119999732 ) ) ;
#11505 = DIRECTION ( 'NONE',  ( 0.000000000000000000, 1.000000000000000000, 0.000000000000000000 ) ) ;
#11506 = ORIENTED_EDGE ( 'NONE', *, *, #22626, .T. ) ;
#11507 = EDGE_CURVE ( 'NONE', #5924, #18376, #7533, .T. ) ;
#11508 = CYLINDRICAL_SURFACE ( 'NONE', #10172, 4.750000000000000888 ) ;
#11509 = CARTESIAN_POINT ( 'NONE',  ( -38.09325189486211372, -65.74401273906202903, -1.048281052909203925 ) ) ;
#11510 = CARTESIAN_POINT ( 'NONE',  ( -12.71070678442828772, -92.56772982770620217, 27.72528925393579868 ) ) ;
#11511 = ORIENTED_EDGE ( 'NONE', *, *, #2247, .F. ) ;
#11512 = CARTESIAN_POINT ( 'NONE',  ( 19.93551599202017499, -18.49999999997239186, -7.473404292298043039 ) ) ;
#11513 = DIRECTION ( 'NONE',  ( 0.000000000000000000, 0.000000000000000000, 1.000000000000000000 ) ) ;
#11514 = DIRECTION ( 'NONE',  ( 0.000000000000000000, 1.000000000000000000, 0.000000000000000000 ) ) ;
#11515 = VERTEX_POINT ( 'NONE', #5465 ) ;
#11516 = CARTESIAN_POINT ( 'NONE',  ( -27.68682485439999752, -24.80000000000000071, -50.68039294919999804 ) ) ;
#11517 = CARTESIAN_POINT ( 'NONE',  ( -19.41484581850000168, -39.36519097789999933, 11.81754271080000152 ) ) ;
#11518 = CARTESIAN_POINT ( 'NONE',  ( 7.279266295386986663, -36.17014819251620850, -21.46816513959021222 ) ) ;
#11519 = CARTESIAN_POINT ( 'NONE',  ( -13.16184031329999904, -70.12921433920000425, -24.09257711200000074 ) ) ;
#11520 = DIRECTION ( 'NONE',  ( 0.000000000000000000, 1.000000000000000000, 0.000000000000000000 ) ) ;
#11521 = CARTESIAN_POINT ( 'NONE',  ( 27.08636525929999905, -66.18149755910000920, 1.733009796709999994 ) ) ;
#11522 = CARTESIAN_POINT ( 'NONE',  ( -6.781378104809999030, -111.0000000000000000, 14.49182221120000058 ) ) ;
#11523 = TOROIDAL_SURFACE ( 'NONE', #18995, 15.50000000000000000, 0.5000000000000000000 ) ;
#11524 = ORIENTED_EDGE ( 'NONE', *, *, #26858, .T. ) ;
#11525 = B_SPLINE_CURVE_WITH_KNOTS ( 'NONE', 5,
 ( #21228, #10406, #5905, #10124, #23553, #23687, #21097, #12592, #7702 ),
 .UNSPECIFIED., .F., .F.,
 ( 6, 3, 6 ),
 ( 0.000000000000000000, 0.5000000000000000000, 1.000000000000000000 ),
 .UNSPECIFIED. ) ;
#11526 = CARTESIAN_POINT ( 'NONE',  ( -37.60355029590000697, -84.50000000000000000, 9.356041104380000917 ) ) ;
#11527 = DIRECTION ( 'NONE',  ( 0.5439177849611214199, 0.000000000000000000, -0.8391385125251892285 ) ) ;
#11528 = EDGE_CURVE ( 'NONE', #28438, #26536, #23741, .T. ) ;
#11529 = CARTESIAN_POINT ( 'NONE',  ( 8.140396429159999059, -100.8869814400000138, 13.38618259969999968 ) ) ;
#11530 = ORIENTED_EDGE ( 'NONE', *, *, #26572, .T. ) ;
#11531 = CARTESIAN_POINT ( 'NONE',  ( 7.432602092569998931, -73.95640471630001400, 39.04179453189999549 ) ) ;
#11532 = CARTESIAN_POINT ( 'NONE',  ( 0.000000000000000000, -37.08699221940000257, 0.000000000000000000 ) ) ;
#11533 = ADVANCED_FACE ( 'NONE', ( #21068 ), #11484, .T. ) ;
#11534 = CIRCLE ( 'NONE', #14368, 55.67692378859999991 ) ;
#11535 = CARTESIAN_POINT ( 'NONE',  ( 21.19011208810000113, -36.03998686679999963, -8.396978594420000164 ) ) ;
#11536 = AXIS2_PLACEMENT_3D ( 'NONE', #3919, #2, #12784 ) ;
#11537 = DIRECTION ( 'NONE',  ( 0.000000000000000000, 1.000000000000000000, 0.000000000000000000 ) ) ;
#11538 = CARTESIAN_POINT ( 'NONE',  ( 8.753883147839999879, -36.52594017789999725, -21.30736199240000062 ) ) ;
#11539 = EDGE_CURVE ( 'NONE', #10505, #22467, #10271, .T. ) ;
#11540 = CARTESIAN_POINT ( 'NONE',  ( 46.12332288492410015, -73.99999999901751835, -4.489694478895246199 ) ) ;
#11541 = VERTEX_POINT ( 'NONE', #1623 ) ;
#11542 = ADVANCED_FACE ( 'NONE', ( #1485 ), #27984, .T. ) ;
#11543 = CARTESIAN_POINT ( 'NONE',  ( 6.888450598059999486, -99.53431388120000634, 15.99365471700000008 ) ) ;
#11544 = CARTESIAN_POINT ( 'NONE',  ( -36.74526444670264169, -63.06504043304235552, 0.1318650859689453059 ) ) ;
#11545 = CARTESIAN_POINT ( 'NONE',  ( -12.77867724610393552, -19.48040540344112870, 19.46310901654912584 ) ) ;
#11546 = CARTESIAN_POINT ( 'NONE',  ( 0.000000000000000000, -101.6484611540000031, 0.000000000000000000 ) ) ;
#11547 = CARTESIAN_POINT ( 'NONE',  ( -2.645789240093490591, -19.49660179754663858, -24.10947003643325814 ) ) ;
#11548 = CARTESIAN_POINT ( 'NONE',  ( 11.86312790959999930, -101.5317765570000006, -10.86703365620000028 ) ) ;
#11549 = CARTESIAN_POINT ( 'NONE',  ( -2.127492191069999983, -26.08233090739999938, -22.84993033459999978 ) ) ;
#11550 = CARTESIAN_POINT ( 'NONE',  ( 13.81470970028357215, -95.86012411014323220, 17.32825506473149701 ) ) ;
#11551 = CARTESIAN_POINT ( 'NONE',  ( -39.32889484840046634, -73.62261561668437082, 7.218875474177834484 ) ) ;
#11552 = CARTESIAN_POINT ( 'NONE',  ( 21.78580818603761671, -37.64222968075310405, -8.476164595188171447 ) ) ;
#11553 = CARTESIAN_POINT ( 'NONE',  ( -38.25943422533623561, -65.12255024415871674, -2.746802154549074615 ) ) ;
#11554 = DIRECTION ( 'NONE',  ( 0.000000000000000000, -1.000000000000000000, 0.000000000000000000 ) ) ;
#11555 = CARTESIAN_POINT ( 'NONE',  ( -37.60355029590000697, -74.50000000000000000, -9.356041104380000917 ) ) ;
#11556 = VERTEX_POINT ( 'NONE', #14847 ) ;
#11557 = CARTESIAN_POINT ( 'NONE',  ( -32.40381740377279840, -80.05388657958994258, -22.56932125262067856 ) ) ;
#11558 = AXIS2_PLACEMENT_3D ( 'NONE', #23403, #3443, #12310 ) ;
#11559 = CIRCLE ( 'NONE', #10153, 22.39904313779999612 ) ;
#11560 = CARTESIAN_POINT ( 'NONE',  ( -13.99699122829999887, -67.43047917469999675, 22.37324552669999989 ) ) ;
#11561 = CARTESIAN_POINT ( 'NONE',  ( -13.71875444750000028, -58.84831425530000359, 21.01328297090000063 ) ) ;
#11562 = DIRECTION ( 'NONE',  ( 1.000000000000000000, 0.000000000000000000, 0.000000000000000000 ) ) ;
#11563 = DIRECTION ( 'NONE',  ( 0.000000000000000000, -1.000000000000000000, 0.000000000000000000 ) ) ;
#11564 = CARTESIAN_POINT ( 'NONE',  ( -14.54628291358669046, -94.01603309693408050, -21.62126842404864746 ) ) ;
#11565 = EDGE_CURVE ( 'NONE', #17228, #14724, #11683, .T. ) ;
#11566 = CARTESIAN_POINT ( 'NONE',  ( -11.37119059761108453, -49.51244866342480577, -22.45585869990737393 ) ) ;
#11567 = ORIENTED_EDGE ( 'NONE', *, *, #1880, .T. ) ;
#11568 = CIRCLE ( 'NONE', #940, 0.3500000000000003664 ) ;
#11569 = CARTESIAN_POINT ( 'NONE',  ( 30.27730015304011957, -74.21788658106061121, -24.84071712252042730 ) ) ;
#11570 = EDGE_CURVE ( 'NONE', #9669, #13629, #2895, .T. ) ;
#11571 = CARTESIAN_POINT ( 'NONE',  ( -21.78729678839999906, -95.70830610310001418, -5.566096626759999388 ) ) ;
#11572 = ORIENTED_EDGE ( 'NONE', *, *, #327, .T. ) ;
#11573 = CARTESIAN_POINT ( 'NONE',  ( 9.457795928940385011, -92.92035259857971141, 28.99786150557102715 ) ) ;
#11574 = CIRCLE ( 'NONE', #26264, 18.64285714289999873 ) ;
#11575 = AXIS2_PLACEMENT_3D ( 'NONE', #23880, #24018, #3917 ) ;
#11576 = CARTESIAN_POINT ( 'NONE',  ( 21.50956136779998573, -52.61368720119948250, 10.11639787089999132 ) ) ;
#11577 = DIRECTION ( 'NONE',  ( 0.000000000000000000, 0.000000000000000000, 1.000000000000000000 ) ) ;
#11578 = AXIS2_PLACEMENT_3D ( 'NONE', #14635, #23531, #14899 ) ;
#11579 = CARTESIAN_POINT ( 'NONE',  ( 36.28164458690000060, -74.50000000000000000, -14.97346873880000118 ) ) ;
#11580 = CARTESIAN_POINT ( 'NONE',  ( -7.242474372567466290, -73.77182148726545563, -39.65872146218941907 ) ) ;
#11581 = FACE_OUTER_BOUND ( 'NONE', #6559, .T. ) ;
#11582 = CARTESIAN_POINT ( 'NONE',  ( -21.64068549270000119, -66.52838475369999571, 15.77032591200000233 ) ) ;
#11583 = CARTESIAN_POINT ( 'NONE',  ( -17.08506256729766193, -97.54019988239669203, 10.37759590189724790 ) ) ;
#11584 = ORIENTED_EDGE ( 'NONE', *, *, #13776, .F. ) ;
#11585 = CARTESIAN_POINT ( 'NONE',  ( -12.54443447719999938, -72.70510876110000709, -25.73426150890000130 ) ) ;
#11586 = CARTESIAN_POINT ( 'NONE',  ( 0.000000000000000000, -92.50000000000000000, 0.000000000000000000 ) ) ;
#11587 = CARTESIAN_POINT ( 'NONE',  ( 7.830640929019831553, -101.5867234369360403, 14.00591651322954689 ) ) ;
#11588 = CARTESIAN_POINT ( 'NONE',  ( 21.58194535263011815, -19.48522775728685019, 9.512926974174723327 ) ) ;
#11589 = CARTESIAN_POINT ( 'NONE',  ( 0.000000000000000000, -92.50000000000000000, 0.000000000000000000 ) ) ;
#11590 = EDGE_LOOP ( 'NONE', ( #6360, #13430, #19441, #26953 ) ) ;
#11591 = EDGE_CURVE ( 'NONE', #8975, #12823, #4258, .T. ) ;
#11592 = AXIS2_PLACEMENT_3D ( 'NONE', #24801, #18088, #11513 ) ;
#11593 = CARTESIAN_POINT ( 'NONE',  ( 26.95513443413419452, -92.54687141712491893, -14.27132724549746534 ) ) ;
#11594 = VERTEX_POINT ( 'NONE', #26229 ) ;
#11595 = AXIS2_PLACEMENT_3D ( 'NONE', #20778, #11563, #24991 ) ;
#11596 = CIRCLE ( 'NONE', #15299, 0.4999999999999986122 ) ;
#11597 = CARTESIAN_POINT ( 'NONE',  ( 0.000000000000000000, -13.40000000000000036, 0.000000000000000000 ) ) ;
#11598 = CARTESIAN_POINT ( 'NONE',  ( 1.312652382290000030, -94.71481430560001513, 24.32357623499999733 ) ) ;
#11599 = CARTESIAN_POINT ( 'NONE',  ( 4.103525764680000520, -93.31218863639999483, 25.66466408690000023 ) ) ;
#11600 = ORIENTED_EDGE ( 'NONE', *, *, #861, .F. ) ;
#11601 = EDGE_CURVE ( 'NONE', #10333, #1165, #7992, .T. ) ;
#11602 = ORIENTED_EDGE ( 'NONE', *, *, #11904, .F. ) ;
#11603 = DIRECTION ( 'NONE',  ( 1.000000000000000000, 0.000000000000000000, 0.000000000000000000 ) ) ;
#11604 = CARTESIAN_POINT ( 'NONE',  ( 21.48399581230000166, -36.52810941199999917, -9.014522560119999639 ) ) ;
#11605 = CARTESIAN_POINT ( 'NONE',  ( 47.13175990429999729, -74.43591472970000211, -1.325790583919999932 ) ) ;
#11606 = EDGE_LOOP ( 'NONE', ( #11040, #18647, #18316, #16333 ) ) ;
#11607 = CARTESIAN_POINT ( 'NONE',  ( 7.243236069894179785, -73.78481856924898352, -39.68146194261722570 ) ) ;
#11608 = CARTESIAN_POINT ( 'NONE',  ( -11.76147443210928500, -63.18033547063078714, 21.37881495694788825 ) ) ;
#11609 = CARTESIAN_POINT ( 'NONE',  ( 7.584268347236687191, -101.5555611381076204, 14.08825305945834394 ) ) ;
#11610 = CARTESIAN_POINT ( 'NONE',  ( -2.889377628239999662, -70.54208558220000214, -27.60766051819999944 ) ) ;
#11611 = FACE_OUTER_BOUND ( 'NONE', #11809, .T. ) ;
#11612 = CARTESIAN_POINT ( 'NONE',  ( -15.78701019289999863, -72.82938648530000592, 23.94860758740000151 ) ) ;
#11613 = ORIENTED_EDGE ( 'NONE', *, *, #24788, .F. ) ;
#11614 = CIRCLE ( 'NONE', #27922, 4.750000000000000000 ) ;
#11615 = AXIS2_PLACEMENT_3D ( 'NONE', #27518, #5637, #1284 ) ;
#11616 = CARTESIAN_POINT ( 'NONE',  ( 36.39327240949999975, -74.35351771279999866, -14.75026165080000062 ) ) ;
#11617 = CARTESIAN_POINT ( 'NONE',  ( -16.89322606969999896, -99.75798417260000406, 3.074878952570000212 ) ) ;
#11618 = CARTESIAN_POINT ( 'NONE',  ( -21.99449553610000052, -74.01681409379999366, -32.14594688369999886 ) ) ;
#11619 = EDGE_LOOP ( 'NONE', ( #1866, #15166, #22835, #14436 ) ) ;
#11620 = CARTESIAN_POINT ( 'NONE',  ( 15.14880929390000119, -101.6484611540000031, 3.280789078519999791 ) ) ;
#11621 = CARTESIAN_POINT ( 'NONE',  ( -7.458790909887997422, -73.99982286725833092, 39.02883428035619318 ) ) ;
#11622 = FACE_OUTER_BOUND ( 'NONE', #14917, .T. ) ;
#11623 = ORIENTED_EDGE ( 'NONE', *, *, #17062, .F. ) ;
#11624 = EDGE_CURVE ( 'NONE', #24455, #4274, #20566, .T. ) ;
#11625 = ADVANCED_FACE ( 'NONE', ( #10887 ), #1497, .T. ) ;
#11626 = CARTESIAN_POINT ( 'NONE',  ( 21.46759780150000196, -62.96338283689998860, 11.34255856240000071 ) ) ;
#11627 = CARTESIAN_POINT ( 'NONE',  ( 8.043104929030000960, -34.87912771779999588, -21.12346526210000164 ) ) ;
#11628 = CARTESIAN_POINT ( 'NONE',  ( 16.22618840215064395, -100.6338045034763979, 4.332579364030344493 ) ) ;
#11629 = DIRECTION ( 'NONE',  ( 1.000000000000000000, 0.000000000000000000, 0.000000000000000000 ) ) ;
#11630 = ORIENTED_EDGE ( 'NONE', *, *, #27694, .T. ) ;
#11631 = CARTESIAN_POINT ( 'NONE',  ( 47.25063473080000165, -79.41040171960000293, -0.8747163666420000316 ) ) ;
#11632 = ITEM_DEFINED_TRANSFORMATION ( 'NONE', 'NONE', #27848,  #26433 ) ;
#11633 = CARTESIAN_POINT ( 'NONE',  ( -11.12754515849999848, -19.46434200899999922, 19.08244047510000030 ) ) ;
#11634 = CARTESIAN_POINT ( 'NONE',  ( -11.63050495949999963, -60.55397095009999475, -20.76951049480000222 ) ) ;
#11635 = EDGE_CURVE ( 'NONE', #7412, #24358, #6552, .T. ) ;
#11636 = AXIS2_PLACEMENT_3D ( 'NONE', #25002, #14075, #554 ) ;
#11637 = DIRECTION ( 'NONE',  ( -1.000000000000000000, 0.000000000000000000, 6.308085367188389255E-16 ) ) ;
#11638 = CARTESIAN_POINT ( 'NONE',  ( 50.00000000000000000, -15.00000000000000000, 4.500000000000000000 ) ) ;
#11639 = CIRCLE ( 'NONE', #27015, 29.91857981989999971 ) ;
#11640 = ORIENTED_EDGE ( 'NONE', *, *, #19460, .F. ) ;
#11641 = CIRCLE ( 'NONE', #23753, 55.67692378859999991 ) ;
#11642 = CARTESIAN_POINT ( 'NONE',  ( -38.44999999999999574, -65.00000000000000000, -2.684678751729999480 ) ) ;
#11643 = ORIENTED_EDGE ( 'NONE', *, *, #22594, .T. ) ;
#11644 = CARTESIAN_POINT ( 'NONE',  ( -13.46188194249999981, -19.39368401379999796, 20.39616198339999897 ) ) ;
#11645 = CARTESIAN_POINT ( 'NONE',  ( -21.83908241200000333, -74.03505044649999434, -32.25228936610000119 ) ) ;
#11646 = ORIENTED_EDGE ( 'NONE', *, *, #19056, .F. ) ;
#11647 = CARTESIAN_POINT ( 'NONE',  ( 45.84677419350000349, -80.50000000000000000, -4.286925650119999709 ) ) ;
#11648 = CARTESIAN_POINT ( 'NONE',  ( 22.82319683875572736, -42.27314267049876406, -0.5642692666673589930 ) ) ;
#11649 = CARTESIAN_POINT ( 'NONE',  ( -10.48404752216234570, -19.47261270939580058, -20.20374288751023428 ) ) ;
#11650 = CARTESIAN_POINT ( 'NONE',  ( -3.577689640331730203, -19.50000000000000000, -25.07857796645360793 ) ) ;
#11651 = CARTESIAN_POINT ( 'NONE',  ( -7.333297298759998917, -94.59276292389999696, -22.63874378639999563 ) ) ;
#11652 = CARTESIAN_POINT ( 'NONE',  ( 21.65968896626973361, -37.88705161499458995, -8.203619567505477050 ) ) ;
#11653 = ORIENTED_EDGE ( 'NONE', *, *, #9575, .F. ) ;
#11654 = CARTESIAN_POINT ( 'NONE',  ( -32.67527180329999936, -79.50000000000000000, -22.00249031559999935 ) ) ;
#11655 = CARTESIAN_POINT ( 'NONE',  ( -37.82487616201437675, -65.66931566142197596, -0.7649176087804624435 ) ) ;
#11656 = DIRECTION ( 'NONE',  ( 1.000000000000000000, 0.000000000000000000, 0.000000000000000000 ) ) ;
#11657 = CARTESIAN_POINT ( 'NONE',  ( -13.01302628178067700, -92.66191076874173405, 27.58469122193175949 ) ) ;
#11658 = VERTEX_POINT ( 'NONE', #15566 ) ;
#11659 = B_SPLINE_CURVE_WITH_KNOTS ( 'NONE', 5,
 ( #4964, #23049, #7610, #22752, #12088, #9901 ),
 .UNSPECIFIED., .F., .F.,
 ( 6, 6 ),
 ( 0.000000000000000000, 1.000000000000000000 ),
 .UNSPECIFIED. ) ;
#11660 = FACE_OUTER_BOUND ( 'NONE', #28193, .T. ) ;
#11661 = DIRECTION ( 'NONE',  ( 0.000000000000000000, -1.000000000000000000, 0.000000000000000000 ) ) ;
#11662 = DIRECTION ( 'NONE',  ( 0.000000000000000000, 1.000000000000000000, 0.000000000000000000 ) ) ;
#11663 = ORIENTED_EDGE ( 'NONE', *, *, #8666, .T. ) ;
#11664 = AXIS2_PLACEMENT_3D ( 'NONE', #13872, #6890, #4406 ) ;
#11665 = CARTESIAN_POINT ( 'NONE',  ( -18.04416748670000459, -95.71113290489999770, 13.55963794960000079 ) ) ;
#11666 = TOROIDAL_SURFACE ( 'NONE', #15867, 29.91857981989999971, 10.00000000000000000 ) ;
#11667 = CARTESIAN_POINT ( 'NONE',  ( -19.96385611919999903, -52.58489974409999945, 14.40794232450000045 ) ) ;
#11668 = CARTESIAN_POINT ( 'NONE',  ( -36.59277592640000165, -79.50000000000000000, -25.98617420859999783 ) ) ;
#11669 = DIRECTION ( 'NONE',  ( 0.000000000000000000, 1.000000000000000000, 0.000000000000000000 ) ) ;
#11670 = EDGE_CURVE ( 'NONE', #9243, #14226, #15726, .T. ) ;
#11671 = CARTESIAN_POINT ( 'NONE',  ( -14.93121066289999987, -74.50000000000000000, 36.29905574720000061 ) ) ;
#11672 = EDGE_CURVE ( 'NONE', #12707, #22756, #9382, .T. ) ;
#11673 = SHAPE_REPRESENTATION_RELATIONSHIP ( 'NONE' , 'NONE' ,  #24690, #23754 ) ;
#11674 = EDGE_CURVE ( 'NONE', #3120, #8180, #18212, .T. ) ;
#11675 = ADVANCED_FACE ( 'NONE', ( #27397 ), #14654, .T. ) ;
#11676 = VERTEX_POINT ( 'NONE', #10119 ) ;
#11677 = CARTESIAN_POINT ( 'NONE',  ( -0.1689899845689999958, -101.2530993010000060, -15.19297360289999865 ) ) ;
#11678 = CARTESIAN_POINT ( 'NONE',  ( 10.18609790949999905, -99.75094907060000082, 14.67385898429999891 ) ) ;
#11679 = VERTEX_POINT ( 'NONE', #25063 ) ;
#11680 = CIRCLE ( 'NONE', #15378, 18.64285714289999873 ) ;
#11681 = CARTESIAN_POINT ( 'NONE',  ( 7.252015964940000003, -74.29298176469998793, 40.34085930499999506 ) ) ;
#11682 = CARTESIAN_POINT ( 'NONE',  ( 7.880018115929998679, -18.50000000000000000, -19.31987738409999977 ) ) ;
#11683 = CIRCLE ( 'NONE', #6597, 7.750000000000000000 ) ;
#11684 = TOROIDAL_SURFACE ( 'NONE', #25216, 21.14285714289999873, 0.5000000000000000000 ) ;
#11685 = CARTESIAN_POINT ( 'NONE',  ( 21.47791241899999903, -36.56811125080000835, -7.356933755090000027 ) ) ;
#11686 = CARTESIAN_POINT ( 'NONE',  ( -7.417318425790000447, -100.8455998110000138, 14.22575192579999914 ) ) ;
#11687 = FACE_OUTER_BOUND ( 'NONE', #17889, .T. ) ;
#11688 = CARTESIAN_POINT ( 'NONE',  ( -17.42343749999999858, -74.50000000000000000, 43.92022684009999978 ) ) ;
#11689 = CARTESIAN_POINT ( 'NONE',  ( 9.104027697630002081, -35.96031139400000143, -20.29387716869999991 ) ) ;
#11690 = CARTESIAN_POINT ( 'NONE',  ( 7.405704750090000843, -101.1273033739999931, 13.62605079230000094 ) ) ;
#11691 = ORIENTED_EDGE ( 'NONE', *, *, #16529, .F. ) ;
#11692 = CARTESIAN_POINT ( 'NONE',  ( -43.25079786316290154, -65.12158389262772573, 0.1356225091523582948 ) ) ;
#11693 = CARTESIAN_POINT ( 'NONE',  ( -36.76943391352939727, -63.07120704560310998, -0.1555577424969001310 ) ) ;
#11694 = CARTESIAN_POINT ( 'NONE',  ( 0.6456114843440000639, -99.57787118740000665, -17.34593263700000421 ) ) ;
#11695 = EDGE_LOOP ( 'NONE', ( #11506, #16279, #2270, #24002, #22506 ) ) ;
#11696 = DIRECTION ( 'NONE',  ( 0.4794255386042040601, 0.000000000000000000, 0.8775825618903720926 ) ) ;
#11697 = CARTESIAN_POINT ( 'NONE',  ( 11.32586188939999872, -100.9728541479999961, -10.72774646679999933 ) ) ;
#11698 = CARTESIAN_POINT ( 'NONE',  ( -0.5268692886119999974, -39.36519097800000111, -22.72252104480000057 ) ) ;
#11699 = CARTESIAN_POINT ( 'NONE',  ( 15.40147643716055015, -95.08513980200086735, 17.29809606948850131 ) ) ;
#11700 = CYLINDRICAL_SURFACE ( 'NONE', #21622, 4.749999999999999112 ) ;
#11701 = DIRECTION ( 'NONE',  ( 0.000000000000000000, 1.000000000000000000, 0.000000000000000000 ) ) ;
#11702 = CARTESIAN_POINT ( 'NONE',  ( 22.26662627820000040, -57.47855601759999900, -7.066909182049999849 ) ) ;
#11703 = CARTESIAN_POINT ( 'NONE',  ( -40.00000000000000000, -69.50000000000000000, 0.000000000000000000 ) ) ;
#11704 = CARTESIAN_POINT ( 'NONE',  ( -16.77201711099999670, -99.85760268239999959, 2.755376769609999776 ) ) ;
#11705 = CIRCLE ( 'NONE', #23373, 6.999999999999997335 ) ;
#11706 = EDGE_LOOP ( 'NONE', ( #11001, #24331, #4597 ) ) ;
#11707 = VECTOR ( 'NONE', #23030, 1000.000000000000000 ) ;
#11708 = ADVANCED_FACE ( 'NONE', ( #3584 ), #5097, .F. ) ;
#11709 = CARTESIAN_POINT ( 'NONE',  ( 36.47289859480000729, -74.92271630800000537, -14.78463751350000166 ) ) ;
#11710 = FACE_OUTER_BOUND ( 'NONE', #10851, .T. ) ;
#11711 = CARTESIAN_POINT ( 'NONE',  ( -32.77174707999999725, -79.50000000000000000, -21.60034937969999902 ) ) ;
#11712 = EDGE_CURVE ( 'NONE', #23028, #13365, #27095, .T. ) ;
#11713 = CARTESIAN_POINT ( 'NONE',  ( 23.56050396080000198, -94.79581469870001342, -2.314010422780000464 ) ) ;
#11714 = CARTESIAN_POINT ( 'NONE',  ( 20.49277737539999933, -35.23997945060000347, -8.776869873949999956 ) ) ;
#11715 = CARTESIAN_POINT ( 'NONE',  ( 7.250083186822952719, -73.98707088500670181, 40.01432744662073304 ) ) ;
#11716 = CARTESIAN_POINT ( 'NONE',  ( -2.363861431290001924, -52.59522851919944486, -24.20187825489998090 ) ) ;
#11717 = CARTESIAN_POINT ( 'NONE',  ( 21.58808931389999586, -36.72098037479999988, -8.655529985299999396 ) ) ;
#11718 = DIRECTION ( 'NONE',  ( 0.000000000000000000, -1.000000000000000000, 0.000000000000000000 ) ) ;
#11719 = CARTESIAN_POINT ( 'NONE',  ( -18.72457341818005006, -96.53847999818908932, -10.28520624310983678 ) ) ;
#11720 = CIRCLE ( 'NONE', #21501, 0.7500000000000006661 ) ;
#11721 = DIRECTION ( 'NONE',  ( 0.000000000000000000, 1.000000000000000000, 0.000000000000000000 ) ) ;
#11722 = ORIENTED_EDGE ( 'NONE', *, *, #14908, .T. ) ;
#11723 = B_SPLINE_CURVE_WITH_KNOTS ( 'NONE', 5,
 ( #6944, #18306, #26905, #7094, #11576, #20041, #11729, #2279, #22383 ),
 .UNSPECIFIED., .F., .F.,
 ( 6, 3, 6 ),
 ( 0.000000000000000000, 0.5000000000000000000, 1.000000000000000000 ),
 .UNSPECIFIED. ) ;
#11724 = LINE ( 'NONE', #7375, #16163 ) ;
#11725 = CARTESIAN_POINT ( 'NONE',  ( -22.20135144879999700, -95.98460637919998817, -5.903444897400000002 ) ) ;
#11726 = EDGE_LOOP ( 'NONE', ( #7213, #5403, #21858, #24708 ) ) ;
#11727 = CIRCLE ( 'NONE', #19176, 12.00000000000000000 ) ;
#11728 = CARTESIAN_POINT ( 'NONE',  ( 9.093840868627895091, -92.81370807120056554, 29.11275331569328273 ) ) ;
#11729 = CARTESIAN_POINT ( 'NONE',  ( 22.45957212889998189, -52.58489974409948076, 10.08523539449999085 ) ) ;
#11730 = CARTESIAN_POINT ( 'NONE',  ( -38.23579088423348082, -63.33604893235135336, 1.392788587647418197 ) ) ;
#11731 = DIRECTION ( 'NONE',  ( 0.9704142011833034598, 0.000000000000000000, 0.2414462220490750377 ) ) ;
#11732 = CARTESIAN_POINT ( 'NONE',  ( -7.169550435265128030, -73.50000000000004263, -38.90587669234852797 ) ) ;
#11733 = CARTESIAN_POINT ( 'NONE',  ( -14.10481785270000010, -74.02367878169998505, 36.45432549239999531 ) ) ;
#11734 = CARTESIAN_POINT ( 'NONE',  ( 9.720248444560001033, -72.82938969829999110, -26.98670033600000195 ) ) ;
#11735 = CARTESIAN_POINT ( 'NONE',  ( -13.47268409989999860, -20.68842595469999779, 20.42652994440000214 ) ) ;
#11736 = B_SPLINE_SURFACE_WITH_KNOTS ( 'NONE', 5, 5, ( 
 ( #23492, #7640, #19115, #16507, #8040, #25405 ),
 ( #12390, #10200, #3123, #20748, #807, #5433 ),
 ( #14727, #8592, #26091, #3807, #23906, #24194 ),
 ( #5843, #17494, #23624, #3664, #8173, #19251 ),
 ( #10337, #28410, #22014, #10473, #8726, #3943 ),
 ( #8302, #12807, #28556, #6120, #4225, #19667 ) ),
 .UNSPECIFIED., .F., .F., .F.,
 ( 6, 6 ),
 ( 6, 6 ),
 ( 7.179549394140000373, 14.35382494800000153 ),
 ( 0.000000000000000000, 0.5000000000000000000 ),
 .UNSPECIFIED. ) ;
#11737 = ORIENTED_EDGE ( 'NONE', *, *, #18475, .T. ) ;
#11738 = CARTESIAN_POINT ( 'NONE',  ( -11.95864023049999858, -71.65979788389999783, -26.06651585250000025 ) ) ;
#11739 = FACE_OUTER_BOUND ( 'NONE', #21510, .T. ) ;
#11740 = FACE_OUTER_BOUND ( 'NONE', #8057, .T. ) ;
#11741 = DIRECTION ( 'NONE',  ( 0.000000000000000000, 1.000000000000000000, 0.000000000000000000 ) ) ;
#11742 = CARTESIAN_POINT ( 'NONE',  ( 15.67492025179999970, -101.0314399550000104, 2.383182498780000103 ) ) ;
#11743 = ORIENTED_EDGE ( 'NONE', *, *, #4581, .F. ) ;
#11744 = EDGE_CURVE ( 'NONE', #3132, #21723, #447, .T. ) ;
#11745 = TOROIDAL_SURFACE ( 'NONE', #28038, 18.14285714289999873, 0.5000000000000000000 ) ;
#11746 = CIRCLE ( 'NONE', #14984, 16.00000000000000000 ) ;
#11747 = ORIENTED_EDGE ( 'NONE', *, *, #11997, .T. ) ;
#11748 = AXIS2_PLACEMENT_3D ( 'NONE', #23873, #23729, #3772 ) ;
#11749 = EDGE_CURVE ( 'NONE', #8439, #18513, #1007, .T. ) ;
#11750 = CARTESIAN_POINT ( 'NONE',  ( 0.000000000000000000, -56.78056608349999834, 0.000000000000000000 ) ) ;
#11751 = CARTESIAN_POINT ( 'NONE',  ( -0.4238013828789999882, -95.77248565759998655, 22.35470455460000139 ) ) ;
#11752 = CARTESIAN_POINT ( 'NONE',  ( 5.659366841679999816, -92.97642175670000597, 26.32172450590000068 ) ) ;
#11753 = ORIENTED_EDGE ( 'NONE', *, *, #24082, .F. ) ;
#11754 = VERTEX_POINT ( 'NONE', #23409 ) ;
#11755 = CARTESIAN_POINT ( 'NONE',  ( -25.90513195527891099, -94.04667188315717397, -2.194660316649619691 ) ) ;
#11756 = CARTESIAN_POINT ( 'NONE',  ( -12.50340864429999854, -94.22763312360000043, -20.80754938939999832 ) ) ;
#11757 = CARTESIAN_POINT ( 'NONE',  ( 2.356750984242918623, -93.20709273738651746, 27.37396933629507600 ) ) ;
#11758 = VERTEX_POINT ( 'NONE', #12315 ) ;
#11759 = CARTESIAN_POINT ( 'NONE',  ( 7.215638845179813465, -73.61009970497924826, -39.29494613562393113 ) ) ;
#11760 = CARTESIAN_POINT ( 'NONE',  ( -11.63271255370046831, -62.50667214630417590, 21.20421611403313022 ) ) ;
#11761 = CARTESIAN_POINT ( 'NONE',  ( -8.841108207830000509, -95.92024868639998658, -20.36834459239999973 ) ) ;
#11762 = B_SPLINE_CURVE_WITH_KNOTS ( 'NONE', 5,
 ( #1816, #19577, #26293, #15178, #4130, #13004 ),
 .UNSPECIFIED., .F., .F.,
 ( 6, 6 ),
 ( 0.000000000000000000, 1.000000000000000000 ),
 .UNSPECIFIED. ) ;
#11763 = EDGE_CURVE ( 'NONE', #19780, #14378, #19853, .T. ) ;
#11764 = CARTESIAN_POINT ( 'NONE',  ( -4.062024957338500109, -70.93524644749820141, -28.43407472284975412 ) ) ;
#11765 = CONICAL_SURFACE ( 'NONE', #25280, 55.67692378859999280, 1.047197551199999799 ) ;
#11766 = CARTESIAN_POINT ( 'NONE',  ( -4.459622768110000024, -72.00000000000000000, -28.73485779310000154 ) ) ;
#11767 = CIRCLE ( 'NONE', #20632, 0.5000000000000004441 ) ;
#11768 = CARTESIAN_POINT ( 'NONE',  ( -11.18243144779999909, -57.47855601759999900, 20.51090144570000007 ) ) ;
#11769 = ORIENTED_EDGE ( 'NONE', *, *, #25740, .F. ) ;
#11770 = CARTESIAN_POINT ( 'NONE',  ( 7.460698725479999927E-15, -74.00000000000000000, 40.00000000000000000 ) ) ;
#11771 = CARTESIAN_POINT ( 'NONE',  ( -16.14211878319999727, -101.0779259520000011, 3.133147776259999961 ) ) ;
#11772 = CARTESIAN_POINT ( 'NONE',  ( 23.61566637130000146, -60.59571585039999775, -0.5691291156790000416 ) ) ;
#11773 = CARTESIAN_POINT ( 'NONE',  ( -21.99377254480000232, -74.28769487450000497, -32.60949123969999874 ) ) ;
#11774 = ORIENTED_EDGE ( 'NONE', *, *, #11200, .T. ) ;
#11775 = CARTESIAN_POINT ( 'NONE',  ( 26.46310988749999993, -64.24504445130001784, 1.532420830840000026 ) ) ;
#11776 = FACE_OUTER_BOUND ( 'NONE', #16898, .T. ) ;
#11777 = CARTESIAN_POINT ( 'NONE',  ( 23.76596721370000154, -92.50425969839999141, -17.55797138329999640 ) ) ;
#11778 = ORIENTED_EDGE ( 'NONE', *, *, #327, .F. ) ;
#11780 = EDGE_CURVE ( 'NONE', #12588, #4769, #13083, .T. ) ;
#11779 = CARTESIAN_POINT ( 'NONE',  ( 0.3059185938709999553, -111.0000000000000000, 14.72672055670000013 ) ) ;
#11781 = AXIS2_PLACEMENT_3D ( 'NONE', #21055, #2699, #25425 ) ;
#11782 = CARTESIAN_POINT ( 'NONE',  ( 21.06982195980000228, -60.33243244399999128, 10.82665592080000216 ) ) ;
#11783 = FACE_OUTER_BOUND ( 'NONE', #27605, .T. ) ;
#11784 = CARTESIAN_POINT ( 'NONE',  ( 16.41212907226823248, -100.4010812937642214, 4.355947949365128302 ) ) ;
#11785 = CARTESIAN_POINT ( 'NONE',  ( 19.94074090517771225, -94.89420224093041156, 14.19047658555035518 ) ) ;
#11786 = ORIENTED_EDGE ( 'NONE', *, *, #2613, .T. ) ;
#11787 = CARTESIAN_POINT ( 'NONE',  ( 20.49588873660000132, -52.63280639819999607, 10.85734681379999955 ) ) ;
#11788 = EDGE_CURVE ( 'NONE', #10257, #6300, #19041, .T. ) ;
#11789 = CARTESIAN_POINT ( 'NONE',  ( -11.41403033759999985, -60.27227161350000273, -22.50529123499999784 ) ) ;
#11790 = CARTESIAN_POINT ( 'NONE',  ( 37.26113007297411883, -80.00000001582722575, -13.81325807140697037 ) ) ;
#11791 = CONICAL_SURFACE ( 'NONE', #18336, 55.67692378859999280, 1.047197551199999799 ) ;
#11792 = LINE ( 'NONE', #3082, #8883 ) ;
#11793 = DIRECTION ( 'NONE',  ( -0.3390050494208429743, -0.7071067811866730279, -0.6205445805637129775 ) ) ;
#11794 = VERTEX_POINT ( 'NONE', #19035 ) ;
#11795 = CARTESIAN_POINT ( 'NONE',  ( -28.54979082390000045, -36.85000000000000142, -52.26004156059999417 ) ) ;
#11796 = ORIENTED_EDGE ( 'NONE', *, *, #14473, .T. ) ;
#11797 = CARTESIAN_POINT ( 'NONE',  ( 20.34628061899999807, -52.63293862069999562, 11.13082833170000008 ) ) ;
#11798 = CARTESIAN_POINT ( 'NONE',  ( -21.65925653600000444, -74.22385006870000268, -32.64405417670000276 ) ) ;
#11799 = ORIENTED_EDGE ( 'NONE', *, *, #10520, .T. ) ;
#11800 = CARTESIAN_POINT ( 'NONE',  ( -18.05095464379880354, -92.86910234287326205, -23.30076470957695634 ) ) ;
#11801 = CARTESIAN_POINT ( 'NONE',  ( 47.25000000000000000, -77.00000000000000000, 7.327133149349999745E-15 ) ) ;
#11802 = EDGE_CURVE ( 'NONE', #7860, #26269, #18759, .T. ) ;
#11803 = AXIS2_PLACEMENT_3D ( 'NONE', #25003, #5038, #4756 ) ;
#11804 = CARTESIAN_POINT ( 'NONE',  ( 0.000000000000000000, -84.75000000000000000, 0.000000000000000000 ) ) ;
#11805 = CARTESIAN_POINT ( 'NONE',  ( -10.44824884758171457, -19.47630530571390750, -20.50788404414224786 ) ) ;
#11806 = DIRECTION ( 'NONE',  ( -0.9704142011833033488, 0.000000000000000000, -0.2414462220490755373 ) ) ;
#11807 = CARTESIAN_POINT ( 'NONE',  ( -3.633282526024673054, -96.53847999809016756, -21.05218219683358072 ) ) ;
#11808 = CARTESIAN_POINT ( 'NONE',  ( 47.19127288053609703, -79.33764839652816647, -1.165204315948687119 ) ) ;
#11809 = EDGE_LOOP ( 'NONE', ( #26084, #24781, #473, #2294 ) ) ;
#11810 = CARTESIAN_POINT ( 'NONE',  ( -32.48908668560000024, -80.00000024250000763, -22.62871150349999638 ) ) ;
#11811 = DIRECTION ( 'NONE',  ( -0.8775825618903722036, 0.000000000000000000, 0.4794255386042041156 ) ) ;
#11812 = DIRECTION ( 'NONE',  ( 1.000000000000000000, 0.000000000000000000, 0.000000000000000000 ) ) ;
#11813 = ORIENTED_EDGE ( 'NONE', *, *, #23023, .F. ) ;
#11814 = AXIS2_PLACEMENT_3D ( 'NONE', #14375, #18898, #16413 ) ;
#11815 = CARTESIAN_POINT ( 'NONE',  ( 0.000000000000000000, 4.440892098500000496E-16, 0.000000000000000000 ) ) ;
#11816 = CARTESIAN_POINT ( 'NONE',  ( -12.59499905819999910, -101.4254868729999970, -9.817004629319999509 ) ) ;
#11817 = DIRECTION ( 'NONE',  ( 0.000000000000000000, -1.000000000000000000, 0.000000000000000000 ) ) ;
#11818 = ORIENTED_EDGE ( 'NONE', *, *, #2493, .F. ) ;
#11819 = CARTESIAN_POINT ( 'NONE',  ( -17.16832732159999964, -98.24896744320000153, 8.807259461759999297 ) ) ;
#11820 = CARTESIAN_POINT ( 'NONE',  ( -19.65068252670000248, -52.63280639819999607, 12.32128691209999971 ) ) ;
#11821 = LINE ( 'NONE', #25099, #17019 ) ;
#11822 = CARTESIAN_POINT ( 'NONE',  ( 2.876553231629999985, -100.0000000000000000, 5.265495371340000119 ) ) ;
#11823 = CARTESIAN_POINT ( 'NONE',  ( 23.52622274289999638, -57.40875708169999569, -9.564507863490000261 ) ) ;
#11824 = CIRCLE ( 'NONE', #17351, 32.39999999999999858 ) ;
#11825 = CARTESIAN_POINT ( 'NONE',  ( 26.32473474220000043, -67.65187322490000099, 0.01358298500609999779 ) ) ;
#11826 = VECTOR ( 'NONE', #25591, 999.9999999999998863 ) ;
#11827 = ORIENTED_EDGE ( 'NONE', *, *, #15873, .F. ) ;
#11828 = DIRECTION ( 'NONE',  ( 0.000000000000000000, 1.000000000000000000, 0.000000000000000000 ) ) ;
#11829 = CARTESIAN_POINT ( 'NONE',  ( 17.39024827180000088, -95.90105875090000609, 14.90673015379999988 ) ) ;
#11830 = EDGE_LOOP ( 'NONE', ( #26326, #19914 ) ) ;
#11831 = AXIS2_PLACEMENT_3D ( 'NONE', #3281, #824, #16376 ) ;
#11832 = DIRECTION ( 'NONE',  ( 0.000000000000000000, 0.000000000000000000, -1.000000000000000000 ) ) ;
#11833 = CARTESIAN_POINT ( 'NONE',  ( 16.49890011909999643, -94.79581646409999962, 16.97758076400000249 ) ) ;
#11834 = EDGE_CURVE ( 'NONE', #18068, #11263, #20236, .T. ) ;
#11835 = DIRECTION ( 'NONE',  ( 0.000000000000000000, -1.000000000000000000, 0.000000000000000000 ) ) ;
#11836 = CARTESIAN_POINT ( 'NONE',  ( -7.940795358099999923, -100.3063911739999980, 15.09437935239999895 ) ) ;
#11837 = CARTESIAN_POINT ( 'NONE',  ( 26.85202045726772013, -72.75638125331757067, -10.08991345884111723 ) ) ;
#11838 = CARTESIAN_POINT ( 'NONE',  ( -10.31966890614535082, -93.93488429366382775, -23.20916244078144075 ) ) ;
#11839 = APPLICATION_CONTEXT ( 'automotive_design' ) ;
#11840 = LINE ( 'NONE', #7497, #24329 ) ;
#11841 = CARTESIAN_POINT ( 'NONE',  ( -3.835404308829999831, -8.750000000000000000, -7.020660495120000455 ) ) ;
#11842 = ORIENTED_EDGE ( 'NONE', *, *, #23468, .F. ) ;
#11843 = EDGE_CURVE ( 'NONE', #23734, #7833, #25103, .T. ) ;
#11844 = CARTESIAN_POINT ( 'NONE',  ( -39.95935625357012100, -73.95086734775428283, 7.250038883934483813 ) ) ;
#11845 = CARTESIAN_POINT ( 'NONE',  ( 24.58030493329999899, -18.50000000000000000, 2.442848308399999890 ) ) ;
#11846 = CARTESIAN_POINT ( 'NONE',  ( 11.56323489949999939, -97.41042626769998947, -18.07474074250000129 ) ) ;
#11847 = EDGE_LOOP ( 'NONE', ( #1009, #14561, #484, #24013 ) ) ;
#11848 = CIRCLE ( 'NONE', #2081, 30.50000000000000000 ) ;
#11849 = CARTESIAN_POINT ( 'NONE',  ( -2.552856939384906543, -19.48524588020510961, -23.44805131028554968 ) ) ;
#11850 = ADVANCED_FACE ( 'NONE', ( #19312 ), #19474, .T. ) ;
#11851 = DIRECTION ( 'NONE',  ( 0.000000000000000000, 1.000000000000000000, 0.000000000000000000 ) ) ;
#11852 = DIRECTION ( 'NONE',  ( -0.09362217723111272705, 0.000000000000000000, 0.9956077982471339682 ) ) ;
#11853 = CARTESIAN_POINT ( 'NONE',  ( 15.97618948326800314, -94.80901416784320190, 17.25790605317358484 ) ) ;
#11854 = EDGE_CURVE ( 'NONE', #22747, #12473, #6464, .T. ) ;
#11855 = CARTESIAN_POINT ( 'NONE',  ( -25.37284092810000047, -92.50000000000000000, 2.543411731580000001 ) ) ;
#11856 = DIRECTION ( 'NONE',  ( 0.000000000000000000, 1.000000000000000000, 0.000000000000000000 ) ) ;
#11857 = CARTESIAN_POINT ( 'NONE',  ( 21.60733108839999872, -40.74566548650000186, -7.843434090929999769 ) ) ;
#11858 = CARTESIAN_POINT ( 'NONE',  ( -6.665307709260000379, -101.1889999979999999, -13.13558364449999871 ) ) ;
#11859 = DIRECTION ( 'NONE',  ( 0.9704142011833034598, 0.000000000000000000, 0.2414462220490750377 ) ) ;
#11860 = ORIENTED_EDGE ( 'NONE', *, *, #16271, .T. ) ;
#11861 = DIRECTION ( 'NONE',  ( 0.000000000000000000, 1.000000000000000000, 0.000000000000000000 ) ) ;
#11862 = CARTESIAN_POINT ( 'NONE',  ( 13.85716626522326322, -97.34036579237553610, -15.36281561190910949 ) ) ;
#11863 = AXIS2_PLACEMENT_3D ( 'NONE', #24928, #15874, #766 ) ;
#11864 = CARTESIAN_POINT ( 'NONE',  ( -13.17386516979999911, -67.65118726130000937, 22.79090083579999870 ) ) ;
#11865 = CARTESIAN_POINT ( 'NONE',  ( 20.80006503139999907, -34.76181304210000178, -8.489266088069999938 ) ) ;
#11866 = CARTESIAN_POINT ( 'NONE',  ( 7.198125313966591499, -73.54003775238612661, 39.10791602262280975 ) ) ;
#11867 = AXIS2_PLACEMENT_3D ( 'NONE', #22655, #5165, #5009 ) ;
#11868 = DIRECTION ( 'NONE',  ( -0.4692400087391613850, 0.000000000000000000, 0.8830706733883035842 ) ) ;
#11869 = CARTESIAN_POINT ( 'NONE',  ( 21.75659477429999811, -101.1889999979999999, -13.30039788230000042 ) ) ;
#11870 = CARTESIAN_POINT ( 'NONE',  ( -11.32307664130000013, -93.00000000000000000, 9.421136869679999748 ) ) ;
#11871 = CARTESIAN_POINT ( 'NONE',  ( -26.69293917519999937, -22.69689110870000093, -48.86109741659999628 ) ) ;
#11872 = VERTEX_POINT ( 'NONE', #8095 ) ;
#11873 = CYLINDRICAL_SURFACE ( 'NONE', #8243, 7.250000000000004441 ) ;
#11874 = CARTESIAN_POINT ( 'NONE',  ( -20.20541094980000096, -94.98812148390000232, 12.40015412250000004 ) ) ;
#11875 = ORIENTED_EDGE ( 'NONE', *, *, #11834, .F. ) ;
#11876 = CARTESIAN_POINT ( 'NONE',  ( -30.44632542846705192, -92.66777315148624439, 1.808678671120149462 ) ) ;
#11877 = EDGE_CURVE ( 'NONE', #10898, #26111, #1815, .T. ) ;
#11878 = CARTESIAN_POINT ( 'NONE',  ( 0.4337523258651289626, -101.2637735886937094, -16.29242920662442984 ) ) ;
#11879 = CARTESIAN_POINT ( 'NONE',  ( -7.342773311050000196, -74.12494612390000270, 39.65529513239999915 ) ) ;
#11880 = CARTESIAN_POINT ( 'NONE',  ( -11.69640386740000082, -101.0875971110000080, -10.03173011250000002 ) ) ;
#11881 = B_SPLINE_CURVE_WITH_KNOTS ( 'NONE', 5,
 ( #21207, #5747, #25859, #12156, #14762, #1129, #988, #25440, #16970 ),
 .UNSPECIFIED., .F., .F.,
 ( 6, 3, 6 ),
 ( 0.000000000000000000, 0.5000000000000000000, 1.000000000000000000 ),
 .UNSPECIFIED. ) ;
#11882 = CARTESIAN_POINT ( 'NONE',  ( 23.54490914119999800, -94.22485739640001157, -7.400599509700000134 ) ) ;
#11883 = ADVANCED_FACE ( 'NONE', ( #14377 ), #3313, .F. ) ;
#11884 = CARTESIAN_POINT ( 'NONE',  ( -21.38368943589999915, -65.50129831189998697, 15.49162513829999988 ) ) ;
#11885 = CARTESIAN_POINT ( 'NONE',  ( -13.60927699540000013, -35.85183931319999573, 20.77656409820000150 ) ) ;
#11886 = EDGE_LOOP ( 'NONE', ( #15297, #14245, #989, #16793 ) ) ;
#11887 = CARTESIAN_POINT ( 'NONE',  ( -12.44921432620000168, -70.96097656259999553, -25.01534913949999961 ) ) ;
#11888 = CARTESIAN_POINT ( 'NONE',  ( 7.718703860600000688, -22.46373279069999995, -20.74932018339999829 ) ) ;
#11889 = DIRECTION ( 'NONE',  ( 0.000000000000000000, -1.000000000000000000, 0.000000000000000000 ) ) ;
#11890 = DIRECTION ( 'NONE',  ( 0.000000000000000000, 1.000000000000000000, 0.000000000000000000 ) ) ;
#11891 = FACE_OUTER_BOUND ( 'NONE', #2550, .T. ) ;
#11892 = VERTEX_POINT ( 'NONE', #6330 ) ;
#11893 = EDGE_LOOP ( 'NONE', ( #13960, #7703, #8247 ) ) ;
#11894 = AXIS2_PLACEMENT_3D ( 'NONE', #11203, #29, #15588 ) ;
#11895 = DIRECTION ( 'NONE',  ( -0.8737996304181506746, 0.000000000000000000, 0.4862861358100837861 ) ) ;
#11896 = FACE_OUTER_BOUND ( 'NONE', #10805, .T. ) ;
#11897 = CARTESIAN_POINT ( 'NONE',  ( -13.18661228299999877, -93.00000000000000000, 26.85581268440000002 ) ) ;
#11898 = CARTESIAN_POINT ( 'NONE',  ( 1.342731302320000264, -94.57749190790001137, 24.16139931020000020 ) ) ;
#11899 = VERTEX_POINT ( 'NONE', #15188 ) ;
#11900 = B_SPLINE_CURVE_WITH_KNOTS ( 'NONE', 3,
 ( #17608, #21687, #24453, #14965 ),
 .UNSPECIFIED., .F., .F.,
 ( 4, 4 ),
 ( 0.000000000000000000, 1.000000000000000000 ),
 .UNSPECIFIED. ) ;
#11901 = B_SPLINE_CURVE_WITH_KNOTS ( 'NONE', 3,
 ( #18298, #8681, #2161, #2711, #17599, #6524, #26200, #17748, #11564, #27185, #7228, #5028, #12903, #21820, #10713, #19628, #8552, #17455, #26340, #6366, #22816, #20634, #23107, #1125, #1255, #7532, #25436, #5606, #5329, #18736, #9542, #16540, #14219, #18878, #9827, #12292, #27632 ),
 .UNSPECIFIED., .F., .F.,
 ( 4, 2, 2, 1, 1, 1, 2, 2, 2, 2, 1, 1, 1, 2, 2, 2, 2, 1, 1, 1, 2, 2, 4 ),
 ( 0.000000000000000000, 0.1249999999999938105, 0.1874999999999909239, 0.2187499999999897859, 0.2343749999999894529, 0.2421874999999897304, 0.2460937499999898692, 0.2499999999999900080, 0.3750000000000081046, 0.4375000000000174305, 0.4687500000000217604, 0.4843750000000236478, 0.4921875000000245914, 0.4960937500000250355, 0.5000000000000255351, 0.6250000000000371925, 0.6875000000000431877, 0.7187500000000457412, 0.7343750000000467404, 0.7421875000000471845, 0.7460937500000471845, 0.7500000000000471845, 1.000000000000000000 ),
 .UNSPECIFIED. ) ;
#11902 = DIRECTION ( 'NONE',  ( 0.000000000000000000, 1.000000000000000000, 0.000000000000000000 ) ) ;
#11903 = LINE ( 'NONE', #2748, #8861 ) ;
#11904 = EDGE_CURVE ( 'NONE', #11872, #21465, #4594, .T. ) ;
#11905 = CARTESIAN_POINT ( 'NONE',  ( -2.415535008216042723, -94.65677004888377155, 24.01682572601766807 ) ) ;
#11906 = ORIENTED_EDGE ( 'NONE', *, *, #17192, .F. ) ;
#11907 = CARTESIAN_POINT ( 'NONE',  ( 26.02259374959999860, -111.0000000000000000, -15.90831903569999994 ) ) ;
#11908 = CARTESIAN_POINT ( 'NONE',  ( -12.07354857445369589, -64.51954438327166486, 21.77354567074241132 ) ) ;
#11909 = VERTEX_POINT ( 'NONE', #10821 ) ;
#11910 = EDGE_CURVE ( 'NONE', #14582, #1224, #13309, .T. ) ;
#11911 = CARTESIAN_POINT ( 'NONE',  ( 21.56931447779999900, -36.56979901409999911, -6.850353625240000355 ) ) ;
#11912 = DIRECTION ( 'NONE',  ( 0.000000000000000000, 1.000000000000000000, 0.000000000000000000 ) ) ;
#11913 = ADVANCED_FACE ( 'NONE', ( #24257 ), #20340, .T. ) ;
#11914 = CARTESIAN_POINT ( 'NONE',  ( -3.967099564299999770, -72.37489743489999228, -28.45199697809999861 ) ) ;
#11915 = LINE ( 'NONE', #27532, #17263 ) ;
#11916 = VERTEX_POINT ( 'NONE', #28749 ) ;
#11917 = ADVANCED_FACE ( 'NONE', ( #15491 ), #28321, .F. ) ;
#11918 = CARTESIAN_POINT ( 'NONE',  ( -11.91266501540000000, -80.00000000000000000, 46.64429291560000479 ) ) ;
#11919 = CARTESIAN_POINT ( 'NONE',  ( -15.97429264209999999, -100.8622054559999981, 3.109706331429999970 ) ) ;
#11920 = CARTESIAN_POINT ( 'NONE',  ( 23.48147201540000140, -59.02987586149999544, 0.03822384682579999665 ) ) ;
#11921 = CARTESIAN_POINT ( 'NONE',  ( 0.000000000000000000, -83.75000000000000000, 0.000000000000000000 ) ) ;
#11922 = ORIENTED_EDGE ( 'NONE', *, *, #13993, .F. ) ;
#11923 = CARTESIAN_POINT ( 'NONE',  ( -14.42556421679999978, -93.00000000000000000, -2.978755036369999942 ) ) ;
#11924 = FACE_OUTER_BOUND ( 'NONE', #11066, .T. ) ;
#11925 = CARTESIAN_POINT ( 'NONE',  ( 36.65772703477473016, -74.21743014740448530, -14.37316385845866407 ) ) ;
#11926 = ORIENTED_EDGE ( 'NONE', *, *, #17856, .F. ) ;
#11927 = CARTESIAN_POINT ( 'NONE',  ( -12.16975423829999947, -18.50000000000000000, 18.10341905029999765 ) ) ;
#11928 = CARTESIAN_POINT ( 'NONE',  ( 24.22382765300000074, -64.24504439390000243, 10.76339935689999905 ) ) ;
#11929 = CARTESIAN_POINT ( 'NONE',  ( 8.005872823979998998, -35.01852739750000154, -21.16125435099999663 ) ) ;
#11930 = LINE ( 'NONE', #18499, #21520 ) ;
#11931 = DIRECTION ( 'NONE',  ( 1.000000000000000000, 0.000000000000000000, 0.000000000000000000 ) ) ;
#11932 = ORIENTED_EDGE ( 'NONE', *, *, #3117, .F. ) ;
#11933 = CARTESIAN_POINT ( 'NONE',  ( -11.48552613400000055, -58.81334883509999401, -22.65395064680000203 ) ) ;
#11934 = CARTESIAN_POINT ( 'NONE',  ( 24.89230495879999694, -66.03766500179999355, -10.10284571010000043 ) ) ;
#11935 = DIRECTION ( 'NONE',  ( -0.9295286103719527793, 0.000000000000000000, -0.3687499999999814260 ) ) ;
#11936 = ORIENTED_EDGE ( 'NONE', *, *, #9987, .F. ) ;
#11937 = DIRECTION ( 'NONE',  ( 0.000000000000000000, 1.000000000000000000, 0.000000000000000000 ) ) ;
#11938 = VERTEX_POINT ( 'NONE', #21639 ) ;
#11939 = CARTESIAN_POINT ( 'NONE',  ( -13.59612654140000032, -34.59960680470000227, 20.74868692960000160 ) ) ;
#11940 = CARTESIAN_POINT ( 'NONE',  ( -5.390284282690000595, -100.8869817940000075, 14.71056662440000018 ) ) ;
#11941 = ORIENTED_EDGE ( 'NONE', *, *, #15580, .F. ) ;
#11942 = CARTESIAN_POINT ( 'NONE',  ( -18.05096283909999855, -93.00000167610001256, -23.30076369320000040 ) ) ;
#11943 = DIRECTION ( 'NONE',  ( 1.000000000000000000, 0.000000000000000000, 0.000000000000000000 ) ) ;
#11944 = ADVANCED_FACE ( 'NONE', ( #26161 ), #3168, .T. ) ;
#11945 = DIRECTION ( 'NONE',  ( 0.4794255386042040601, 0.000000000000000000, 0.8775825618903719816 ) ) ;
#11946 = CARTESIAN_POINT ( 'NONE',  ( -10.46620651823172210, -19.48040574461845509, -20.79821394406996760 ) ) ;
#11947 = CARTESIAN_POINT ( 'NONE',  ( 22.85993575921586896, -94.54719627003775884, -6.820847890398427538 ) ) ;
#11948 = DIRECTION ( 'NONE',  ( 0.000000000000000000, 1.000000000000000000, 0.000000000000000000 ) ) ;
#11949 = DIRECTION ( 'NONE',  ( 1.000000000000000000, 0.000000000000000000, 0.000000000000000000 ) ) ;
#11950 = ORIENTED_EDGE ( 'NONE', *, *, #26589, .F. ) ;
#11951 = CARTESIAN_POINT ( 'NONE',  ( -32.83566817450000030, -79.50000000000000000, -22.22906645670000003 ) ) ;
#11952 = CARTESIAN_POINT ( 'NONE',  ( 19.83740677649999640, -97.64874574840000321, 2.314389350519999944 ) ) ;
#11953 = CARTESIAN_POINT ( 'NONE',  ( -15.78701020529999965, -72.82938648530000592, 23.94860758700000147 ) ) ;
#11954 = CARTESIAN_POINT ( 'NONE',  ( -12.16265938883512376, -92.50000000000000000, 27.97031705946124802 ) ) ;
#11955 = ORIENTED_EDGE ( 'NONE', *, *, #899, .T. ) ;
#11956 = CARTESIAN_POINT ( 'NONE',  ( -3.027554198780000316, -80.05649091640000847, 46.84443221839999438 ) ) ;
#11957 = CARTESIAN_POINT ( 'NONE',  ( -41.75000000000000000, -64.47022873560000278, 1.587713240270000048 ) ) ;
#11958 = DIRECTION ( 'NONE',  ( 0.000000000000000000, 1.000000000000000000, 0.000000000000000000 ) ) ;
#11959 = ORIENTED_EDGE ( 'NONE', *, *, #25763, .F. ) ;
#11960 = CARTESIAN_POINT ( 'NONE',  ( -17.54428790840000119, -94.59276292389999696, 16.07756064530000017 ) ) ;
#11961 = CARTESIAN_POINT ( 'NONE',  ( -19.13290195579999775, -39.36414254489999820, 12.40799806240000080 ) ) ;
#11962 = DIRECTION ( 'NONE',  ( 0.4794255386042000078, 0.000000000000000000, 0.8775825618903743131 ) ) ;
#11963 = CARTESIAN_POINT ( 'NONE',  ( 29.03740435909999817, -74.36193762290000109, -26.47099454660000362 ) ) ;
#11964 = CARTESIAN_POINT ( 'NONE',  ( 23.97384489419999909, -61.60336911379999947, -9.719973047129998989 ) ) ;
#11965 = EDGE_CURVE ( 'NONE', #519, #3448, #13760, .T. ) ;
#11966 = CARTESIAN_POINT ( 'NONE',  ( 26.37457956329999931, -67.43115654220000010, 0.9352255399990000440 ) ) ;
#11967 = ORIENTED_EDGE ( 'NONE', *, *, #9774, .F. ) ;
#11968 = CARTESIAN_POINT ( 'NONE',  ( -39.61603006850076980, -73.75061506112956522, -7.239953483554843139 ) ) ;
#11969 = AXIS2_PLACEMENT_3D ( 'NONE', #24978, #5166, #9811 ) ;
#11970 = FACE_OUTER_BOUND ( 'NONE', #12194, .T. ) ;
#11971 = ORIENTED_EDGE ( 'NONE', *, *, #1196, .F. ) ;
#11972 = DIRECTION ( 'NONE',  ( -0.4692400087391606633, 0.000000000000000000, 0.8830706733883038062 ) ) ;
#11973 = CARTESIAN_POINT ( 'NONE',  ( -13.31136913029999924, -101.0685849509999912, -9.042834681369999572 ) ) ;
#11974 = EDGE_CURVE ( 'NONE', #16418, #21532, #19950, .T. ) ;
#11975 = B_SPLINE_SURFACE_WITH_KNOTS ( 'NONE', 5, 5, ( 
 ( #34, #22464, #20266, #22612, #335, #19816 ),
 ( #18083, #28694, #26532, #15281, #7020, #4833 ),
 ( #26686, #4389, #13711, #2656, #15437, #13258 ),
 ( #20415, #22165, #8882, #485, #2205, #17795 ),
 ( #6727, #24492, #20567, #16035, #5410, #18527 ),
 ( #27417, #24940, #7615, #14293, #633, #4969 ) ),
 .UNSPECIFIED., .F., .F., .F.,
 ( 6, 6 ),
 ( 6, 6 ),
 ( 7.179431122730000503, 23.44689954309999891 ),
 ( 0.000000000000000000, 0.5000000000000000000 ),
 .UNSPECIFIED. ) ;
#11976 = DIRECTION ( 'NONE',  ( 0.000000000000000000, 1.000000000000000000, 0.000000000000000000 ) ) ;
#11977 = CARTESIAN_POINT ( 'NONE',  ( -7.630334818519999729, -100.8023006570000035, 13.80849637110000039 ) ) ;
#11978 = CARTESIAN_POINT ( 'NONE',  ( -26.33972759919999973, -80.00000000000000000, -36.23922253580000330 ) ) ;
#11979 = CARTESIAN_POINT ( 'NONE',  ( 3.459338121946999694E-15, -73.50000000000000000, -32.25000000000000000 ) ) ;
#11980 = CARTESIAN_POINT ( 'NONE',  ( 7.474780311509999109, -101.1715078010000042, 13.84506678670000035 ) ) ;
#11981 = VERTEX_POINT ( 'NONE', #20170 ) ;
#11982 = AXIS2_PLACEMENT_3D ( 'NONE', #11007, #6536, #22267 ) ;
#11983 = CARTESIAN_POINT ( 'NONE',  ( -40.70731707320000226, -74.50000000000000000, 7.215414233289999757 ) ) ;
#11984 = CARTESIAN_POINT ( 'NONE',  ( 26.60903970598167589, -33.79999999999999716, 48.70752046822583736 ) ) ;
#11985 = CARTESIAN_POINT ( 'NONE',  ( 23.41763709020000306, -53.52700728319999968, -9.527480143570000948 ) ) ;
#11986 = EDGE_LOOP ( 'NONE', ( #17946, #8738, #10862, #22597 ) ) ;
#11987 = CARTESIAN_POINT ( 'NONE',  ( 40.75609756099999714, -80.00000000000000000, -7.713029007999999465 ) ) ;
#11988 = DIRECTION ( 'NONE',  ( 0.000000000000000000, -1.000000000000000000, 0.000000000000000000 ) ) ;
#11989 = CARTESIAN_POINT ( 'NONE',  ( -2.597379844570000262, -26.02764329549999900, -24.46103497820000072 ) ) ;
#11990 = CARTESIAN_POINT ( 'NONE',  ( 0.000000000000000000, -82.25000000000000000, 0.000000000000000000 ) ) ;
#11991 = CARTESIAN_POINT ( 'NONE',  ( -24.63993737860000266, -72.00000000000000000, 17.98210258840000009 ) ) ;
#11992 = B_SPLINE_CURVE_WITH_KNOTS ( 'NONE', 3,
 ( #3370, #16904, #14433, #23190, #25794, #5823, #1471, #14705, #23470, #3510, #14156, #23324 ),
 .UNSPECIFIED., .F., .F.,
 ( 4, 2, 2, 2, 2, 4 ),
 ( 0.000000000000000000, 0.2499999999999840128, 0.3749999999999876210, 0.4374999999999744649, 0.4999999999999613087, 1.000000000000000000 ),
 .UNSPECIFIED. ) ;
#11993 = AXIS2_PLACEMENT_3D ( 'NONE', #26850, #11379, #4848 ) ;
#11994 = CARTESIAN_POINT ( 'NONE',  ( -31.00000000000000000, -15.00000000000000000, -2.398081733189999864E-14 ) ) ;
#11995 = CARTESIAN_POINT ( 'NONE',  ( -40.00000000000000000, -69.00000000000000000, 1.332267629549999902E-15 ) ) ;
#11996 = ORIENTED_EDGE ( 'NONE', *, *, #20104, .T. ) ;
#11997 = EDGE_CURVE ( 'NONE', #11090, #20924, #13245, .T. ) ;
#11998 = CARTESIAN_POINT ( 'NONE',  ( 6.390838521760000113, -101.2010924020000004, 13.85940160760000062 ) ) ;
#11999 = CARTESIAN_POINT ( 'NONE',  ( -22.22906645670000003, -74.50000000000000000, -32.83566817450000030 ) ) ;
#12000 = CARTESIAN_POINT ( 'NONE',  ( 7.610177731959999470, -101.4231532209999926, 14.04048934709999941 ) ) ;
#12001 = AXIS2_PLACEMENT_3D ( 'NONE', #17422, #1985, #12734 ) ;
#12002 = CARTESIAN_POINT ( 'NONE',  ( -11.58382158670000095, -95.11335285699999531, -21.40443484560000087 ) ) ;
#12003 = CARTESIAN_POINT ( 'NONE',  ( 20.83696519829999971, -34.90595158679999344, -8.468982500269998326 ) ) ;
#12004 = CARTESIAN_POINT ( 'NONE',  ( 11.19993727630000002, -57.47855601759999900, 20.50134766809999931 ) ) ;
#12005 = APPLICATION_CONTEXT ( 'automotive_design' ) ;
#12006 = EDGE_CURVE ( 'NONE', #17308, #21862, #18600, .T. ) ;
#12007 = CARTESIAN_POINT ( 'NONE',  ( 0.000000000000000000, -36.20000000000000284, 0.000000000000000000 ) ) ;
#12008 = FACE_OUTER_BOUND ( 'NONE', #12410, .T. ) ;
#12009 = CARTESIAN_POINT ( 'NONE',  ( 8.881784197000000993E-16, -19.50000000000000000, 1.776356839399999922E-14 ) ) ;
#12010 = DIRECTION ( 'NONE',  ( 0.000000000000000000, -1.000000000000000000, 0.000000000000000000 ) ) ;
#12011 = EDGE_LOOP ( 'NONE', ( #4217, #27533, #5919, #25832, #8334 ) ) ;
#12012 = CARTESIAN_POINT ( 'NONE',  ( -5.298192075760000286, -100.9197081840000010, 14.69882727599999939 ) ) ;
#12013 = ORIENTED_EDGE ( 'NONE', *, *, #16364, .T. ) ;
#12014 = DIRECTION ( 'NONE',  ( 0.4794255386042041711, 0.000000000000000000, 0.8775825618903720926 ) ) ;
#12015 = CARTESIAN_POINT ( 'NONE',  ( 0.5547406113394584004, -100.2392017794624053, -17.10134437667061036 ) ) ;
#12016 = CARTESIAN_POINT ( 'NONE',  ( -7.250116280630000354, -73.92445350479999888, 39.77266773049999671 ) ) ;
#12017 = CARTESIAN_POINT ( 'NONE',  ( -43.75000000000000000, -84.50000000000000000, 0.000000000000000000 ) ) ;
#12018 = CARTESIAN_POINT ( 'NONE',  ( -40.70731707320000226, -84.00000000000000000, 7.215414233289999757 ) ) ;
#12019 = CARTESIAN_POINT ( 'NONE',  ( 25.22253955729999930, -73.21919417370000360, -29.84906188120000081 ) ) ;
#12020 = AXIS2_PLACEMENT_3D ( 'NONE', #16234, #22373, #2419 ) ;
#12021 = CYLINDRICAL_SURFACE ( 'NONE', #23462, 58.55000000000003979 ) ;
#12022 = CARTESIAN_POINT ( 'NONE',  ( 12.88056774689999884, -94.79581469870001342, -19.86310563940000051 ) ) ;
#12023 = CARTESIAN_POINT ( 'NONE',  ( 0.000000000000000000, -23.30310889129999907, 0.000000000000000000 ) ) ;
#12024 = CARTESIAN_POINT ( 'NONE',  ( -17.94180966909999597, -18.50000000000000000, 18.81731824139999887 ) ) ;
#12025 = CARTESIAN_POINT ( 'NONE',  ( -36.59277592640000165, -79.50000000000000000, -27.40038777100000189 ) ) ;
#12026 = FACE_OUTER_BOUND ( 'NONE', #25438, .T. ) ;
#12027 = ORIENTED_EDGE ( 'NONE', *, *, #23379, .T. ) ;
#12028 = DIRECTION ( 'NONE',  ( 0.000000000000000000, 1.000000000000000000, 0.000000000000000000 ) ) ;
#12029 = ORIENTED_EDGE ( 'NONE', *, *, #19729, .T. ) ;
#12030 = EDGE_CURVE ( 'NONE', #7500, #8693, #4219, .T. ) ;
#12031 = EDGE_CURVE ( 'NONE', #13803, #20924, #17354, .T. ) ;
#12032 = CARTESIAN_POINT ( 'NONE',  ( -1.981473925119999757, -57.45864736019999697, -23.83876518969999836 ) ) ;
#12033 = AXIS2_PLACEMENT_3D ( 'NONE', #17752, #8555, #26634 ) ;
#12034 = ADVANCED_FACE ( 'NONE', ( #11205 ), #17648, .T. ) ;
#12035 = CARTESIAN_POINT ( 'NONE',  ( -2.607841079019999952, -97.32097376469998551, 21.26526383349999705 ) ) ;
#12036 = CARTESIAN_POINT ( 'NONE',  ( 11.26796299709999971, -92.84764728559999014, 27.58759766900000088 ) ) ;
#12037 = ADVANCED_FACE ( 'NONE', ( #3948 ), #15914, .T. ) ;
#12038 = ORIENTED_EDGE ( 'NONE', *, *, #19596, .T. ) ;
#12039 = VECTOR ( 'NONE', #5542, 1000.000000000000000 ) ;
#12040 = CARTESIAN_POINT ( 'NONE',  ( -11.16205695805461495, -94.83055549493140290, -21.09956338124505137 ) ) ;
#12041 = CIRCLE ( 'NONE', #7883, 0.5000000000000004441 ) ;
#12042 = ORIENTED_EDGE ( 'NONE', *, *, #19697, .F. ) ;
#12043 = DIRECTION ( 'NONE',  ( 0.000000000000000000, -1.000000000000000000, 0.000000000000000000 ) ) ;
#12044 = DIRECTION ( 'NONE',  ( -0.4692400087391606633, 0.000000000000000000, 0.8830706733883038062 ) ) ;
#12045 = CARTESIAN_POINT ( 'NONE',  ( 6.153546133999999945, -93.00000450890000536, 28.82528558229999760 ) ) ;
#12046 = ORIENTED_EDGE ( 'NONE', *, *, #11788, .F. ) ;
#12047 = DIRECTION ( 'NONE',  ( 0.4794255386042041156, 0.000000000000000000, 0.8775825618903722036 ) ) ;
#12048 = CARTESIAN_POINT ( 'NONE',  ( -11.39749306474008783, -60.86470925568636403, 20.85929151947415505 ) ) ;
#12049 = CARTESIAN_POINT ( 'NONE',  ( -14.50205784900000161, -80.23773587339999835, 36.47412430930000227 ) ) ;
#12050 = CARTESIAN_POINT ( 'NONE',  ( 26.98670340789999855, -72.82938977469999031, -9.720255250690000182 ) ) ;
#12051 = CARTESIAN_POINT ( 'NONE',  ( -1.372948704489999949, -68.20869413019998717, -26.54380258120000136 ) ) ;
#12052 = CARTESIAN_POINT ( 'NONE',  ( -17.13033210379999716, -72.00000000000000000, 23.49748962769999849 ) ) ;
#12053 = ORIENTED_EDGE ( 'NONE', *, *, #27354, .F. ) ;
#12054 = CYLINDRICAL_SURFACE ( 'NONE', #6488, 58.55000000000003979 ) ;
#12055 = CARTESIAN_POINT ( 'NONE',  ( -15.86504038540000039, -100.9725757459999897, 3.161101131529999719 ) ) ;
#12056 = CARTESIAN_POINT ( 'NONE',  ( 24.62957909909999898, -63.53922775760000263, 0.3042768451749999770 ) ) ;
#12057 = CARTESIAN_POINT ( 'NONE',  ( -20.13976432299999786, -61.97101110970000093, 13.88607754689999929 ) ) ;
#12058 = ORIENTED_EDGE ( 'NONE', *, *, #21252, .T. ) ;
#12059 = DIRECTION ( 'NONE',  ( 0.000000000000000000, 1.000000000000000000, 0.000000000000000000 ) ) ;
#12060 = CARTESIAN_POINT ( 'NONE',  ( -1.024287211530000130, -18.85467989400000022, -21.87431971389999674 ) ) ;
#12061 = CARTESIAN_POINT ( 'NONE',  ( 22.78264860270000014, -94.59276292389999696, -6.873201011689999085 ) ) ;
#12062 = ORIENTED_EDGE ( 'NONE', *, *, #8004, .F. ) ;
#12063 = TOROIDAL_SURFACE ( 'NONE', #6965, 30.50381168839999901, 2.000000000000000000 ) ;
#12064 = AXIS2_PLACEMENT_3D ( 'NONE', #4238, #15734, #15888 ) ;
#12065 = LINE ( 'NONE', #26305, #5330 ) ;
#12066 = TOROIDAL_SURFACE ( 'NONE', #20932, 4.500000000000000000, 0.5000000000000000000 ) ;
#12067 = DIRECTION ( 'NONE',  ( -0.4151946956541399669, 0.5000000000001689759, -0.7600087925152558821 ) ) ;
#12068 = FACE_OUTER_BOUND ( 'NONE', #24153, .T. ) ;
#12069 = CARTESIAN_POINT ( 'NONE',  ( 15.82576138244594333, -101.2021794473940162, 4.092296143312620593 ) ) ;
#12070 = CARTESIAN_POINT ( 'NONE',  ( 0.000000000000000000, -26.90310889129999694, 0.000000000000000000 ) ) ;
#12071 = EDGE_LOOP ( 'NONE', ( #2079, #13251, #25508, #26555 ) ) ;
#12072 = EDGE_CURVE ( 'NONE', #22989, #24255, #27414, .T. ) ;
#12073 = CONTEXT_DEPENDENT_SHAPE_REPRESENTATION ( #2540, #8978 ) ;
#12074 = CARTESIAN_POINT ( 'NONE',  ( 36.96401661549065665, -79.81539336509945315, -14.32979729325936979 ) ) ;
#12075 = DIRECTION ( 'NONE',  ( 0.4794255386042059475, 0.000000000000000000, 0.8775825618903710934 ) ) ;
#12076 = CARTESIAN_POINT ( 'NONE',  ( 5.621891740541981264, -93.55104906477529880, 26.56729936354081190 ) ) ;
#12077 = EDGE_CURVE ( 'NONE', #813, #25610, #17478, .T. ) ;
#12078 = EDGE_LOOP ( 'NONE', ( #13679, #11511, #15717, #1810 ) ) ;
#12079 = CARTESIAN_POINT ( 'NONE',  ( 47.05360719204802677, -74.23346858368026346, -1.678317851455894072 ) ) ;
#12080 = ORIENTED_EDGE ( 'NONE', *, *, #26072, .F. ) ;
#12081 = CARTESIAN_POINT ( 'NONE',  ( -11.76056861240000018, -34.66497403020000689, 19.52111231130000135 ) ) ;
#12082 = CARTESIAN_POINT ( 'NONE',  ( -5.774731795730000172, -101.2530993039999885, 14.05532693159999980 ) ) ;
#12083 = ORIENTED_EDGE ( 'NONE', *, *, #19249, .T. ) ;
#12084 = CARTESIAN_POINT ( 'NONE',  ( -36.79999999999999716, -63.07912966450000880, -0.1732050807570000017 ) ) ;
#12085 = VECTOR ( 'NONE', #1948, 1000.000000000000000 ) ;
#12086 = AXIS2_PLACEMENT_3D ( 'NONE', #9661, #14331, #25416 ) ;
#12087 = ORIENTED_EDGE ( 'NONE', *, *, #16956, .F. ) ;
#12088 = CARTESIAN_POINT ( 'NONE',  ( -20.34965187303443557, -94.63959659917352951, 12.21935051695949603 ) ) ;
#12089 = SPHERICAL_SURFACE ( 'NONE', #684, 2.000000000000000000 ) ;
#12090 = DIRECTION ( 'NONE',  ( 0.7791198649362079953, 0.000000000000000000, -0.6268749764201669850 ) ) ;
#12091 = CARTESIAN_POINT ( 'NONE',  ( 8.036479196959999201E-15, -79.00000000000000000, -43.75000000000000000 ) ) ;
#12092 = ORIENTED_EDGE ( 'NONE', *, *, #22182, .T. ) ;
#12093 = CARTESIAN_POINT ( 'NONE',  ( -32.83566817450000030, -79.65853147379999655, -22.22906645670000003 ) ) ;
#12094 = CARTESIAN_POINT ( 'NONE',  ( 21.22741177940000057, -96.73974214489999213, 0.9047775657389999227 ) ) ;
#12095 = DIRECTION ( 'NONE',  ( 1.000000000000000000, 0.000000000000000000, 0.000000000000000000 ) ) ;
#12096 = VERTEX_POINT ( 'NONE', #4672 ) ;
#12097 = CARTESIAN_POINT ( 'NONE',  ( -1.461556060870000007, -80.00014850240000897, 47.15629441589999971 ) ) ;
#12098 = CARTESIAN_POINT ( 'NONE',  ( -15.22757417880000119, -66.82180077600000345, 22.72230046389999814 ) ) ;
#12099 = ORIENTED_EDGE ( 'NONE', *, *, #24953, .F. ) ;
#12100 = LINE ( 'NONE', #27985, #15041 ) ;
#12101 = CARTESIAN_POINT ( 'NONE',  ( -19.29510002299999982, -26.05152176790000240, 14.13598958989999765 ) ) ;
#12102 = CARTESIAN_POINT ( 'NONE',  ( -40.00000000000000000, -63.50000000000000000, 0.000000000000000000 ) ) ;
#12103 = CARTESIAN_POINT ( 'NONE',  ( 31.02678878629999559, -72.72326922419999562, -21.89553410619999951 ) ) ;
#12104 = CARTESIAN_POINT ( 'NONE',  ( -16.27748161717928710, -72.55114741086336494, 23.56761092879465735 ) ) ;
#12105 = CIRCLE ( 'NONE', #28376, 21.03431122519999974 ) ;
#12106 = AXIS2_PLACEMENT_3D ( 'NONE', #12255, #1089, #9927 ) ;
#12107 = ADVANCED_FACE ( 'NONE', ( #22609 ), #3234, .F. ) ;
#12108 = EDGE_CURVE ( 'NONE', #18837, #7118, #5664, .T. ) ;
#12109 = ORIENTED_EDGE ( 'NONE', *, *, #20581, .T. ) ;
#12110 = CYLINDRICAL_SURFACE ( 'NONE', #9533, 15.99999999999999467 ) ;
#12111 = CARTESIAN_POINT ( 'NONE',  ( 19.64679318960000032, -35.95469792330000303, -9.266762188240001308 ) ) ;
#12112 = CARTESIAN_POINT ( 'NONE',  ( 7.618259826220000086, -101.6474417639999928, 14.07078423930000000 ) ) ;
#12113 = EDGE_LOOP ( 'NONE', ( #3670, #7897, #18361, #17927 ) ) ;
#12114 = CARTESIAN_POINT ( 'NONE',  ( 0.000000000000000000, -102.5000000000000000, 0.000000000000000000 ) ) ;
#12115 = DIRECTION ( 'NONE',  ( 0.000000000000000000, -1.000000000000000000, 0.000000000000000000 ) ) ;
#12116 = CARTESIAN_POINT ( 'NONE',  ( -7.864778453279999582, -100.4808658609999981, 14.18740396090000111 ) ) ;
#12117 = DIRECTION ( 'NONE',  ( 0.000000000000000000, 1.000000000000000000, 0.000000000000000000 ) ) ;
#12118 = CARTESIAN_POINT ( 'NONE',  ( 7.194012074090000652, -40.75181153199999784, -21.61346702620000215 ) ) ;
#12119 = CIRCLE ( 'NONE', #4680, 55.50192378860000275 ) ;
#12120 = CARTESIAN_POINT ( 'NONE',  ( 7.350260020649999504, -101.1292391010000102, 13.65356784849999983 ) ) ;
#12121 = ORIENTED_EDGE ( 'NONE', *, *, #1406, .F. ) ;
#12122 = AXIS2_PLACEMENT_3D ( 'NONE', #6446, #26281, #6304 ) ;
#12123 = CARTESIAN_POINT ( 'NONE',  ( -40.33192879147393484, -74.21175622409107575, 7.242418264996894450 ) ) ;
#12124 = CIRCLE ( 'NONE', #5157, 2.000000494510000504 ) ;
#12125 = EDGE_CURVE ( 'NONE', #12804, #14272, #13708, .T. ) ;
#12126 = CARTESIAN_POINT ( 'NONE',  ( 0.000000000000000000, -101.6484611540000031, 0.000000000000000000 ) ) ;
#12127 = CARTESIAN_POINT ( 'NONE',  ( 12.11264993960000069, -99.91547912590000635, -13.29325542860000020 ) ) ;
#12128 = ORIENTED_EDGE ( 'NONE', *, *, #23777, .F. ) ;
#12129 = CARTESIAN_POINT ( 'NONE',  ( 23.93312658989999875, -65.07443093669999712, -7.727579958389999781 ) ) ;
#12130 = FACE_BOUND ( 'NONE', #19663, .T. ) ;
#12131 = CARTESIAN_POINT ( 'NONE',  ( -1.237516097069999876, -26.09793778660000285, -22.31349595290000210 ) ) ;
#12132 = CARTESIAN_POINT ( 'NONE',  ( -17.63818201149086207, -92.64884742711599586, 24.88264283798182319 ) ) ;
#12133 = CARTESIAN_POINT ( 'NONE',  ( -2.289506448460466359, -74.01267423981741445, 46.88251229324449554 ) ) ;
#12134 = CARTESIAN_POINT ( 'NONE',  ( 20.59810750441412708, -36.05978015059736208, -9.165578419059432491 ) ) ;
#12135 = CARTESIAN_POINT ( 'NONE',  ( 21.70991749090000056, -40.75155002489999845, -6.890073352940000007 ) ) ;
#12136 = CARTESIAN_POINT ( 'NONE',  ( 12.96030886027237905, -98.56104087989207585, 15.02160250790822893 ) ) ;
#12137 = CARTESIAN_POINT ( 'NONE',  ( -15.54744790750000050, -100.8070272189999912, 2.643184715480000335 ) ) ;
#12138 = ORIENTED_EDGE ( 'NONE', *, *, #24879, .F. ) ;
#12139 = EDGE_CURVE ( 'NONE', #22328, #4674, #25106, .T. ) ;
#12140 = CARTESIAN_POINT ( 'NONE',  ( 6.916664799299999444, -101.1716782170000073, 14.13220977900000008 ) ) ;
#12141 = CARTESIAN_POINT ( 'NONE',  ( 0.000000000000000000, -101.1889999979999999, 0.000000000000000000 ) ) ;
#12142 = CARTESIAN_POINT ( 'NONE',  ( 7.500294343269999331, -101.1699703470000031, 13.83260060669999980 ) ) ;
#12143 = CIRCLE ( 'NONE', #17723, 7.249999999999999112 ) ;
#12144 = TOROIDAL_SURFACE ( 'NONE', #15359, 6.750000000000000000, 2.000000000000000000 ) ;
#12145 = VECTOR ( 'NONE', #12287, 1000.000000000000000 ) ;
#12146 = CARTESIAN_POINT ( 'NONE',  ( -11.73626313630000162, -94.71481430550001335, -21.34524641919999866 ) ) ;
#12147 = CARTESIAN_POINT ( 'NONE',  ( 19.44233901680000187, -34.85245972529999392, -8.988706454689999958 ) ) ;
#12148 = DIRECTION ( 'NONE',  ( 0.000000000000000000, 1.000000000000000000, 0.000000000000000000 ) ) ;
#12149 = AXIS2_PLACEMENT_3D ( 'NONE', #10276, #21514, #26321 ) ;
#12150 = DIRECTION ( 'NONE',  ( 0.000000000000000000, 1.000000000000000000, 0.000000000000000000 ) ) ;
#12151 = CARTESIAN_POINT ( 'NONE',  ( -40.00438978219865049, -74.28332971660954342, 7.315286554457401280 ) ) ;
#12152 = LINE ( 'NONE', #21065, #16419 ) ;
#12153 = DIRECTION ( 'NONE',  ( 1.000000000000000000, 0.000000000000000000, 0.000000000000000000 ) ) ;
#12154 = ORIENTED_EDGE ( 'NONE', *, *, #2410, .T. ) ;
#12155 = CARTESIAN_POINT ( 'NONE',  ( 8.137534397419999621, -101.2306315539999986, 14.02341335179999859 ) ) ;
#12156 = CARTESIAN_POINT ( 'NONE',  ( -16.98428476389999631, -99.78393587620000460, 3.406952114930000164 ) ) ;
#12157 = ORIENTED_EDGE ( 'NONE', *, *, #13276, .T. ) ;
#12158 = CARTESIAN_POINT ( 'NONE',  ( 9.476764215410000247, -84.00000000000000000, 38.08875739639999836 ) ) ;
#12159 = CARTESIAN_POINT ( 'NONE',  ( 0.6026929693157587753, -100.4507315469087843, -16.92988022290758110 ) ) ;
#12160 = MECHANICAL_DESIGN_GEOMETRIC_PRESENTATION_REPRESENTATION (  '', ( #28040 ), #17276 ) ;
#12161 = EDGE_CURVE ( 'NONE', #26794, #12777, #21628, .T. ) ;
#12162 = CARTESIAN_POINT ( 'NONE',  ( -11.57749895095710357, -19.46656749805027076, 19.05743507200596909 ) ) ;
#12163 = CARTESIAN_POINT ( 'NONE',  ( -7.260189318799999292, -74.10695981599999982, 39.96660922950000128 ) ) ;
#12164 = CARTESIAN_POINT ( 'NONE',  ( -25.57735248450000043, -26.54349610970000128, -46.81902967690000139 ) ) ;
#12165 = DIRECTION ( 'NONE',  ( 0.000000000000000000, 0.000000000000000000, 1.000000000000000000 ) ) ;
#12166 = CARTESIAN_POINT ( 'NONE',  ( 27.75394116159999669, -74.50000000000000000, -27.75394116159999669 ) ) ;
#12167 = AXIS2_PLACEMENT_3D ( 'NONE', #21853, #24186, #21431 ) ;
#12168 = CARTESIAN_POINT ( 'NONE',  ( -17.54428855099999751, -94.59276292389999696, 16.07755916609999858 ) ) ;
#12169 = CARTESIAN_POINT ( 'NONE',  ( 13.48409207689999967, -95.94970068820001075, -18.04862505909999726 ) ) ;
#12170 = CARTESIAN_POINT ( 'NONE',  ( -14.94683085001314282, -101.1292394719999379, 4.127768892864509986 ) ) ;
#12171 = CARTESIAN_POINT ( 'NONE',  ( 9.024081099289999131, -19.49999992740000110, -18.94592230980000380 ) ) ;
#12172 = EDGE_CURVE ( 'NONE', #4529, #26855, #13623, .T. ) ;
#12173 = FACE_OUTER_BOUND ( 'NONE', #13167, .T. ) ;
#12174 = ORIENTED_EDGE ( 'NONE', *, *, #8900, .T. ) ;
#12175 = DIRECTION ( 'NONE',  ( 0.000000000000000000, -1.000000000000000000, 0.000000000000000000 ) ) ;
#12176 = ORIENTED_EDGE ( 'NONE', *, *, #25916, .T. ) ;
#12177 = CIRCLE ( 'NONE', #28460, 55.67692378859999991 ) ;
#12178 = CARTESIAN_POINT ( 'NONE',  ( 38.08875739639999836, -82.25000000000000000, 9.476764215410000247 ) ) ;
#12179 = CIRCLE ( 'NONE', #8466, 15.19391340349999986 ) ;
#12180 = CARTESIAN_POINT ( 'NONE',  ( 10.15270808350000031, -36.18298320499999932, -21.93668074720000050 ) ) ;
#12181 = CARTESIAN_POINT ( 'NONE',  ( -29.71161909530000145, -92.92146929989999649, 6.352307300799999723 ) ) ;
#12182 = AXIS2_PLACEMENT_3D ( 'NONE', #15294, #1937, #13124 ) ;
#12183 = DIRECTION ( 'NONE',  ( 1.000000000000000000, 0.000000000000000000, 0.000000000000000000 ) ) ;
#12184 = ORIENTED_EDGE ( 'NONE', *, *, #9105, .F. ) ;
#12185 = ORIENTED_EDGE ( 'NONE', *, *, #10924, .F. ) ;
#12186 = CARTESIAN_POINT ( 'NONE',  ( 0.000000000000000000, -15.00000000000000000, 0.000000000000000000 ) ) ;
#12187 = CYLINDRICAL_SURFACE ( 'NONE', #1373, 9.500000000000001776 ) ;
#12188 = ORIENTED_EDGE ( 'NONE', *, *, #12139, .F. ) ;
#12189 = CARTESIAN_POINT ( 'NONE',  ( -38.55000000000000426, -64.11445222650000630, -2.857883832489999776 ) ) ;
#12190 = CYLINDRICAL_SURFACE ( 'NONE', #18320, 18.64285714289998808 ) ;
#12191 = CARTESIAN_POINT ( 'NONE',  ( -14.66608910859999959, -79.49999990050001486, 36.47374631070000106 ) ) ;
#12192 = ADVANCED_FACE ( 'NONE', ( #23732 ), #27832, .T. ) ;
#12193 = CARTESIAN_POINT ( 'NONE',  ( 6.308882621530000456, -101.1889999979999999, -29.19167084780000110 ) ) ;
#12194 = EDGE_LOOP ( 'NONE', ( #25464, #18393 ) ) ;
#12195 = EDGE_CURVE ( 'NONE', #25480, #14582, #14559, .T. ) ;
#12196 = FACE_OUTER_BOUND ( 'NONE', #20076, .T. ) ;
#12197 = CARTESIAN_POINT ( 'NONE',  ( -16.29874522269999915, -100.6375206259999970, 3.070048125000000017 ) ) ;
#12198 = CARTESIAN_POINT ( 'NONE',  ( 25.71993452759999954, -61.59933877579999972, 1.389394059650000068 ) ) ;
#12199 = CARTESIAN_POINT ( 'NONE',  ( -20.88544710529999904, -61.59957509759999539, 15.07454172879999987 ) ) ;
#12200 = VECTOR ( 'NONE', #23253, 1000.000000000000000 ) ;
#12201 = ORIENTED_EDGE ( 'NONE', *, *, #22175, .T. ) ;
#12202 = CARTESIAN_POINT ( 'NONE',  ( 18.83155579810272684, -99.33527509199842598, 0.2391732240786322572 ) ) ;
#12203 = ADVANCED_FACE ( 'NONE', ( #14429 ), #14831, .F. ) ;
#12204 = AXIS2_PLACEMENT_3D ( 'NONE', #23937, #3976, #26276 ) ;
#12205 = CARTESIAN_POINT ( 'NONE',  ( -1.878544191320000278, -18.85622860559999836, -22.19735407900000013 ) ) ;
#12206 = CARTESIAN_POINT ( 'NONE',  ( 36.75967600126188728, -74.56302832687016746, -14.65138518224945052 ) ) ;
#12207 = VERTEX_POINT ( 'NONE', #19221 ) ;
#12208 = EDGE_CURVE ( 'NONE', #15620, #1234, #26954, .T. ) ;
#12209 = CARTESIAN_POINT ( 'NONE',  ( 24.78974732560000405, -64.24504771300000527, -10.08508462690000052 ) ) ;
#12210 = CARTESIAN_POINT ( 'NONE',  ( 8.986258419809999509, -35.50000000000000000, -19.49544308430000328 ) ) ;
#12211 = CARTESIAN_POINT ( 'NONE',  ( 36.32249705850000510, -79.79205832529999043, -14.87545865919999954 ) ) ;
#12212 = CARTESIAN_POINT ( 'NONE',  ( -36.79999999999999716, -63.07912966450000880, 0.1732050807570000017 ) ) ;
#12213 = EDGE_LOOP ( 'NONE', ( #21708, #27086, #28595 ) ) ;
#12214 = B_SPLINE_SURFACE_WITH_KNOTS ( 'NONE', 5, 5, ( 
 ( #17584, #6509, #15370, #22107, #15822, #15522 ),
 ( #9120, #4470, #22243, #2293, #20059, #8974 ),
 ( #18021, #6809, #24575, #26919, #24733, #22551 ),
 ( #1376, #14745, #8194, #16114, #18322, #12547 ),
 ( #7924, #8062, #7398, #16952, #20497, #2735 ),
 ( #28161, #5204, #16261, #17080, #13789, #27352 ) ),
 .UNSPECIFIED., .F., .F., .F.,
 ( 6, 6 ),
 ( 6, 6 ),
 ( 0.000000000000000000, 3.318582258109999739 ),
 ( 0.000000000000000000, 0.5000000000000000000 ),
 .UNSPECIFIED. ) ;
#12215 = CARTESIAN_POINT ( 'NONE',  ( 37.11608278482759005, -79.94792962045367801, -14.06916263102740494 ) ) ;
#12216 = DIRECTION ( 'NONE',  ( -0.3687499999999814260, 0.000000000000000000, 0.9295286103719527793 ) ) ;
#12217 = CARTESIAN_POINT ( 'NONE',  ( -2.119605539977385877, -80.25103533751058649, 46.93499847706560502 ) ) ;
#12218 = ORIENTED_EDGE ( 'NONE', *, *, #6039, .F. ) ;
#12219 = CARTESIAN_POINT ( 'NONE',  ( 12.04737265770000043, -101.1889999979999999, -10.52904611289999970 ) ) ;
#12220 = CARTESIAN_POINT ( 'NONE',  ( -17.52027961638587783, -99.14332933491964184, 3.769849805601797499 ) ) ;
#12221 = ORIENTED_EDGE ( 'NONE', *, *, #14196, .T. ) ;
#12222 = CIRCLE ( 'NONE', #3404, 6.749999999999999112 ) ;
#12223 = AXIS2_PLACEMENT_3D ( 'NONE', #13995, #5400, #9897 ) ;
#12224 = FACE_OUTER_BOUND ( 'NONE', #8803, .T. ) ;
#12225 = CARTESIAN_POINT ( 'NONE',  ( -5.963512921169999537, -101.1292389529999980, 14.31440776300000017 ) ) ;
#12226 = ORIENTED_EDGE ( 'NONE', *, *, #23115, .F. ) ;
#12227 = AXIS2_PLACEMENT_3D ( 'NONE', #19737, #8657, #19322 ) ;
#12228 = CARTESIAN_POINT ( 'NONE',  ( 9.561259125210000320, -36.00000000000000000, -20.11250876450000291 ) ) ;
#12229 = CARTESIAN_POINT ( 'NONE',  ( 40.30310653829999978, -74.34472676610000974, 7.255206491210000053 ) ) ;
#12230 = DIRECTION ( 'NONE',  ( 0.000000000000000000, -1.000000000000000000, 0.000000000000000000 ) ) ;
#12231 = CARTESIAN_POINT ( 'NONE',  ( 18.85230044170000241, -18.50000000000000000, -8.028472989549999994 ) ) ;
#12232 = ORIENTED_EDGE ( 'NONE', *, *, #21253, .F. ) ;
#12233 = EDGE_CURVE ( 'NONE', #8616, #25599, #17446, .T. ) ;
#12234 = CARTESIAN_POINT ( 'NONE',  ( -32.60788492590000232, -79.95698119190001307, -21.93599790929999926 ) ) ;
#12235 = FACE_OUTER_BOUND ( 'NONE', #20270, .T. ) ;
#12236 = FACE_OUTER_BOUND ( 'NONE', #17950, .T. ) ;
#12237 = ORIENTED_EDGE ( 'NONE', *, *, #7227, .T. ) ;
#12238 = AXIS2_PLACEMENT_3D ( 'NONE', #20620, #9529, #27320 ) ;
#12239 = CARTESIAN_POINT ( 'NONE',  ( 14.36320985907368453, -97.53591929634409041, -14.01783439808674991 ) ) ;
#12240 = CARTESIAN_POINT ( 'NONE',  ( 41.00000000000000000, -74.50000000000000000, 10.20110288159999890 ) ) ;
#12242 = VERTEX_POINT ( 'NONE', #23186 ) ;
#12241 = B_SPLINE_CURVE_WITH_KNOTS ( 'NONE', 3,
 ( #7459, #16607, #27563, #12084 ),
 .UNSPECIFIED., .F., .F.,
 ( 4, 4 ),
 ( 0.000000000000000000, 1.000000000000000000 ),
 .UNSPECIFIED. ) ;
#12243 = EDGE_CURVE ( 'NONE', #2354, #9232, #11094, .T. ) ;
#12244 = CARTESIAN_POINT ( 'NONE',  ( 0.000000000000000000, -25.10000000000000142, 0.000000000000000000 ) ) ;
#12245 = LINE ( 'NONE', #12649, #25023 ) ;
#12246 = CARTESIAN_POINT ( 'NONE',  ( 20.55132429533163219, -97.41291607309865697, 1.353383486903313671 ) ) ;
#12247 = CARTESIAN_POINT ( 'NONE',  ( 31.55438929119999614, -73.56648946160001401, -21.86866566000000134 ) ) ;
#12248 = CARTESIAN_POINT ( 'NONE',  ( -14.48353243600127449, -74.09718790024807333, 36.26064929535388615 ) ) ;
#12249 = CIRCLE ( 'NONE', #15969, 6.000000000000000000 ) ;
#12250 = CARTESIAN_POINT ( 'NONE',  ( -10.61287167039999879, -19.46510050319999863, 19.30934957549999709 ) ) ;
#12251 = DIRECTION ( 'NONE',  ( 0.000000000000000000, 1.000000000000000000, 0.000000000000000000 ) ) ;
#12252 = EDGE_LOOP ( 'NONE', ( #6975, #1244, #16732, #27851 ) ) ;
#12253 = CARTESIAN_POINT ( 'NONE',  ( 21.01622931789999882, -35.47958268320000030, -8.366917739139999810 ) ) ;
#12254 = VECTOR ( 'NONE', #12819, 1000.000000000000000 ) ;
#12255 = CARTESIAN_POINT ( 'NONE',  ( -13.66168260340000096, -72.00000000000000000, -27.27344781959999764 ) ) ;
#12256 = ORIENTED_EDGE ( 'NONE', *, *, #538, .F. ) ;
#12257 = CARTESIAN_POINT ( 'NONE',  ( -13.15133982419999903, -100.9197086960000007, -8.436149064220000326 ) ) ;
#12258 = DIRECTION ( 'NONE',  ( 0.000000000000000000, 1.000000000000000000, 0.000000000000000000 ) ) ;
#12259 = B_SPLINE_CURVE_WITH_KNOTS ( 'NONE', 3,
 ( #20284, #13578, #8619, #17523, #26411, #2530, #6599, #9197, #17673, #22045, #4547, #6894, #2094, #7041, #15907, #26556, #4409, #13280, #2225, #11067, #56, #26853, #8904, #26707, #6745, #15610, #24511, #22331, #2376, #27148 ),
 .UNSPECIFIED., .F., .F.,
 ( 4, 1, 1, 1, 1, 2, 2, 1, 1, 1, 1, 2, 2, 2, 1, 1, 1, 1, 2, 2, 4 ),
 ( 0.000000000000000000, 0.1250000000000360545, 0.1875000000000534572, 0.2187500000000621725, 0.2343750000000665579, 0.2421875000000698330, 0.2500000000000731082, 0.3750000000000863198, 0.4375000000000920375, 0.4687500000000958122, 0.4843750000000985878, 0.4921875000000990319, 0.5000000000000994760, 0.6250000000001237899, 0.6875000000001372236, 0.7187500000001429967, 0.7343750000001472156, 0.7421875000001466605, 0.7460937500001444400, 0.7500000000001422196, 1.000000000000000000 ),
 .UNSPECIFIED. ) ;
#12260 = CARTESIAN_POINT ( 'NONE',  ( 47.25000000000000000, -79.00000000000000000, -7.709388683000000122E-13 ) ) ;
#12261 = CARTESIAN_POINT ( 'NONE',  ( -7.755678108949999761, -100.8746138070000029, 14.68026149039999950 ) ) ;
#12262 = B_SPLINE_CURVE_WITH_KNOTS ( 'NONE', 3,
 ( #6612, #22500, #2392, #20000, #2238, #6761, #11084, #6905, #13438, #15769, #9514, #15623 ),
 .UNSPECIFIED., .F., .F.,
 ( 4, 2, 2, 2, 2, 4 ),
 ( 0.000000000000000000, 0.2500000000000059952, 0.5000000000000119904, 0.6250000000000104361, 0.7500000000000088818, 1.000000000000000000 ),
 .UNSPECIFIED. ) ;
#12263 = CARTESIAN_POINT ( 'NONE',  ( 40.50000000000000000, -12.50000000000000000, 4.500000000000000000 ) ) ;
#12264 = TOROIDAL_SURFACE ( 'NONE', #660, 3.750000000000000000, 1.000000000000000000 ) ;
#12265 = CARTESIAN_POINT ( 'NONE',  ( 7.372139244490000465, -101.1290456289999895, 13.64202221559999906 ) ) ;
#12266 = EDGE_LOOP ( 'NONE', ( #8399, #18285, #3490, #17054 ) ) ;
#12267 = EDGE_CURVE ( 'NONE', #20422, #7753, #19886, .T. ) ;
#12268 = CARTESIAN_POINT ( 'NONE',  ( -43.30001519683280264, -65.09473604209610187, -0.03967052575387554347 ) ) ;
#12269 = CARTESIAN_POINT ( 'NONE',  ( -22.29269736170000016, -94.98812656900000206, -8.065862048359999648 ) ) ;
#12270 = CARTESIAN_POINT ( 'NONE',  ( 23.52622212079999997, -57.40875702419999982, -9.564509902230000193 ) ) ;
#12271 = ORIENTED_EDGE ( 'NONE', *, *, #6717, .T. ) ;
#12273 = EDGE_CURVE ( 'NONE', #3056, #27225, #3505, .T. ) ;
#12272 = CARTESIAN_POINT ( 'NONE',  ( -14.38874196869999977, -74.12911414260001663, 36.70801399449999991 ) ) ;
#12274 = CARTESIAN_POINT ( 'NONE',  ( -14.59919359709999931, -74.50000000000000000, 36.80099833719999936 ) ) ;
#12275 = LINE ( 'NONE', #21187, #26585 ) ;
#12276 = EDGE_CURVE ( 'NONE', #23028, #6664, #20930, .T. ) ;
#12277 = TOROIDAL_SURFACE ( 'NONE', #6690, 3.500000000000000000, 0.5000000000000000000 ) ;
#12278 = CARTESIAN_POINT ( 'NONE',  ( 41.23922093270000033, -74.00000000000000000, -13.75000000000000000 ) ) ;
#12279 = AXIS2_PLACEMENT_3D ( 'NONE', #6623, #4135, #4722 ) ;
#12280 = FACE_OUTER_BOUND ( 'NONE', #20372, .T. ) ;
#12281 = FACE_OUTER_BOUND ( 'NONE', #6510, .T. ) ;
#12282 = CARTESIAN_POINT ( 'NONE',  ( -10.86152808080000121, -19.46485671829999831, -19.26947891709999894 ) ) ;
#12283 = VERTEX_POINT ( 'NONE', #25922 ) ;
#12284 = CARTESIAN_POINT ( 'NONE',  ( -32.83566817900000245, -74.50000000069999828, -22.22906645790000013 ) ) ;
#12285 = CARTESIAN_POINT ( 'NONE',  ( 13.83663993448646323, -97.24405583930904129, -15.54750970113168229 ) ) ;
#12286 = CIRCLE ( 'NONE', #15053, 18.14285714289999873 ) ;
#12287 = DIRECTION ( 'NONE',  ( 0.000000000000000000, 1.000000000000000000, 0.000000000000000000 ) ) ;
#12288 = CARTESIAN_POINT ( 'NONE',  ( 21.08831565240000216, -34.74142176009999616, -8.079293962379999527 ) ) ;
#12289 = CARTESIAN_POINT ( 'NONE',  ( 7.249313954219629430, -73.91187068868498500, 39.89765284896063946 ) ) ;
#12290 = CARTESIAN_POINT ( 'NONE',  ( -12.71547034009999955, -65.00127802399998700, 21.72228991030000245 ) ) ;
#12291 = DIRECTION ( 'NONE',  ( 1.000000000000000000, 0.000000000000000000, 0.000000000000000000 ) ) ;
#12292 = CARTESIAN_POINT ( 'NONE',  ( -22.49587410578730839, -93.00000237470423770, -19.82286531042224098 ) ) ;
#12293 = ORIENTED_EDGE ( 'NONE', *, *, #13439, .F. ) ;
#12294 = CIRCLE ( 'NONE', #23484, 20.64285714289999873 ) ;
#12295 = CARTESIAN_POINT ( 'NONE',  ( -32.20769385759999892, -80.50000045429999318, -22.43272066369999962 ) ) ;
#12296 = LINE ( 'NONE', #16677, #21365 ) ;
#12297 = VERTEX_POINT ( 'NONE', #12231 ) ;
#12298 = DIRECTION ( 'NONE',  ( -0.9704142011833032377, 0.000000000000000000, 0.2414462220490753985 ) ) ;
#12299 = EDGE_LOOP ( 'NONE', ( #12176, #9717, #209, #20264 ) ) ;
#12300 = EDGE_CURVE ( 'NONE', #5390, #2868, #13279, .T. ) ;
#12301 = EDGE_CURVE ( 'NONE', #16727, #24784, #5319, .T. ) ;
#12302 = CARTESIAN_POINT ( 'NONE',  ( 0.5649143243405088111, -100.9616911410344926, -16.52536945643391775 ) ) ;
#12303 = CARTESIAN_POINT ( 'NONE',  ( -7.222916535669999583, -73.70405155900000693, 39.27999006289999784 ) ) ;
#12304 = CARTESIAN_POINT ( 'NONE',  ( 13.69010830728659478, -92.58347372262932140, 27.25492602878164305 ) ) ;
#12305 = FACE_OUTER_BOUND ( 'NONE', #6319, .T. ) ;
#12306 = TOROIDAL_SURFACE ( 'NONE', #17428, 60.66666666670000296, 10.00000000000000000 ) ;
#12307 = DIRECTION ( 'NONE',  ( 0.000000000000000000, -1.000000000000000000, 0.000000000000000000 ) ) ;
#12308 = CARTESIAN_POINT ( 'NONE',  ( -22.62548402540000225, -71.48510949040000639, 17.99032368389999803 ) ) ;
#12309 = AXIS2_PLACEMENT_3D ( 'NONE', #11750, #7402, #10121 ) ;
#12310 = DIRECTION ( 'NONE',  ( 1.000000000000000000, 0.000000000000000000, 0.000000000000000000 ) ) ;
#12311 = CARTESIAN_POINT ( 'NONE',  ( 9.006609686890000077, -25.56710209000000233, -19.14378067089999647 ) ) ;
#12312 = DIRECTION ( 'NONE',  ( -0.8349149399068952482, 0.000000000000000000, -0.5503789995269311452 ) ) ;
#12313 = CARTESIAN_POINT ( 'NONE',  ( 20.07635942769760717, -19.46686856774696750, 9.756771846234537193 ) ) ;
#12314 = ORIENTED_EDGE ( 'NONE', *, *, #15909, .F. ) ;
#12315 = CARTESIAN_POINT ( 'NONE',  ( -11.25326567110000120, -94.84395216780001192, -20.59896464009999661 ) ) ;
#12316 = AXIS2_PLACEMENT_3D ( 'NONE', #11058, #45, #6285 ) ;
#12317 = EDGE_LOOP ( 'NONE', ( #22929, #2863, #18642, #12847 ) ) ;
#12318 = EDGE_CURVE ( 'NONE', #14297, #5567, #11900, .T. ) ;
#12319 = CARTESIAN_POINT ( 'NONE',  ( 0.000000000000000000, 0.000000000000000000, 0.000000000000000000 ) ) ;
#12320 = CARTESIAN_POINT ( 'NONE',  ( 9.382534041599999597, -37.36473931380000124, -22.70474454669999886 ) ) ;
#12321 = CARTESIAN_POINT ( 'NONE',  ( -29.43780281349999939, -92.91851489729999969, 4.711604253540000009 ) ) ;
#12322 = CARTESIAN_POINT ( 'NONE',  ( 0.000000000000000000, -26.59999999999999787, 0.000000000000000000 ) ) ;
#12323 = CARTESIAN_POINT ( 'NONE',  ( 19.86393766627161384, -19.48166550808161190, -8.699994293302530934 ) ) ;
#12324 = CIRCLE ( 'NONE', #4897, 18.14285714289999518 ) ;
#12325 = VERTEX_POINT ( 'NONE', #15242 ) ;
#12326 = PLANE ( 'NONE',  #2814 ) ;
#12327 = ORIENTED_EDGE ( 'NONE', *, *, #9782, .F. ) ;
#12328 = CARTESIAN_POINT ( 'NONE',  ( -5.873418876839999747, -101.1889999979999999, 15.15334698740000086 ) ) ;
#12329 = CARTESIAN_POINT ( 'NONE',  ( 8.638917257509998393, -36.16233246459999862, -20.97577343430000241 ) ) ;
#12330 = CARTESIAN_POINT ( 'NONE',  ( -14.93121080350000085, -79.49999975080000070, 36.29905574549999869 ) ) ;
#12331 = CARTESIAN_POINT ( 'NONE',  ( 25.81290055409999695, -93.01584738559999721, -5.657397443709999862 ) ) ;
#12332 = CARTESIAN_POINT ( 'NONE',  ( -40.00000000000000000, -69.00000000000000000, 0.000000000000000000 ) ) ;
#12333 = VERTEX_POINT ( 'NONE', #26496 ) ;
#12334 = CARTESIAN_POINT ( 'NONE',  ( -15.35765514150000044, -101.3349956970000108, 4.566393778230000144 ) ) ;
#12335 = CARTESIAN_POINT ( 'NONE',  ( -16.34872446949999869, -100.7006823539999942, 3.091720520159999985 ) ) ;
#12336 = CARTESIAN_POINT ( 'NONE',  ( -32.54749500401306506, -74.13779231108122758, -22.15949318078843433 ) ) ;
#12337 = CARTESIAN_POINT ( 'NONE',  ( 36.29989756469999662, -74.04896632250000721, -14.30540807509999901 ) ) ;
#12338 = ORIENTED_EDGE ( 'NONE', *, *, #18745, .T. ) ;
#12339 = CARTESIAN_POINT ( 'NONE',  ( 10.00000000000000000, -89.00000000000000000, 0.000000000000000000 ) ) ;
#12340 = CARTESIAN_POINT ( 'NONE',  ( -2.954912485889999552, -18.62107711730000048, -23.35157406449999939 ) ) ;
#12341 = CARTESIAN_POINT ( 'NONE',  ( 36.45653638919409190, -74.05039938899749075, -14.06393186641748549 ) ) ;
#12342 = ORIENTED_EDGE ( 'NONE', *, *, #25122, .F. ) ;
#12343 = AXIS2_PLACEMENT_3D ( 'NONE', #15555, #24459, #152 ) ;
#12344 = DIRECTION ( 'NONE',  ( 0.000000000000000000, 1.000000000000000000, 0.000000000000000000 ) ) ;
#12345 = DIRECTION ( 'NONE',  ( 0.000000000000000000, 1.000000000000000000, 0.000000000000000000 ) ) ;
#12346 = CARTESIAN_POINT ( 'NONE',  ( 7.135467526410000261, -73.50000000000000000, 38.71641004229999794 ) ) ;
#12347 = ORIENTED_EDGE ( 'NONE', *, *, #10987, .F. ) ;
#12348 = CARTESIAN_POINT ( 'NONE',  ( 6.757998639866319657, -100.5550990438330956, 15.44352938470917991 ) ) ;
#12349 = CARTESIAN_POINT ( 'NONE',  ( -3.016175157618312674, -80.46478795248187055, 46.60229631513919202 ) ) ;
#12350 = EDGE_CURVE ( 'NONE', #10205, #19075, #1382, .T. ) ;
#12351 = EDGE_LOOP ( 'NONE', ( #11335, #1147, #8824, #12674 ) ) ;
#12352 = ORIENTED_EDGE ( 'NONE', *, *, #27358, .F. ) ;
#12353 = CARTESIAN_POINT ( 'NONE',  ( 21.57230431649999858, -55.03616289790000593, 10.16045490650000005 ) ) ;
#12354 = CARTESIAN_POINT ( 'NONE',  ( -5.547446579819999890, -101.0848057460000007, 14.37961489299999940 ) ) ;
#12355 = EDGE_CURVE ( 'NONE', #2148, #22592, #5086, .T. ) ;
#12356 = ORIENTED_EDGE ( 'NONE', *, *, #6404, .T. ) ;
#12357 = CARTESIAN_POINT ( 'NONE',  ( 0.000000000000000000, -102.5000000000000000, 0.000000000000000000 ) ) ;
#12358 = CARTESIAN_POINT ( 'NONE',  ( -28.95818204711633115, -93.00000166546705316, -1.362778528346119566 ) ) ;
#12359 = ADVANCED_FACE ( 'NONE', ( #10575 ), #25009, .T. ) ;
#12360 = CARTESIAN_POINT ( 'NONE',  ( 39.54203581910000054, -73.97629583779999507, 7.314380512899999687 ) ) ;
#12361 = B_SPLINE_CURVE_WITH_KNOTS ( 'NONE', 3,
 ( #20009, #17835, #15479, #15632, #10948, #19858, #6462, #9078, #24390, #27021, #17981, #26873, #18125, #15928 ),
 .UNSPECIFIED., .F., .F.,
 ( 4, 2, 1, 1, 1, 1, 2, 2, 4 ),
 ( 0.000000000000000000, 0.2500000000000070499, 0.3750000000000102696, 0.4375000000000084377, 0.4687500000000041078, 0.4843750000000019429, 0.4921875000000042188, 0.5000000000000064393, 1.000000000000000000 ),
 .UNSPECIFIED. ) ;
#12362 = FACE_OUTER_BOUND ( 'NONE', #16463, .T. ) ;
#12363 = CARTESIAN_POINT ( 'NONE',  ( 16.76176042277295863, -99.62767017971319206, 4.428935492921096895 ) ) ;
#12364 = DIRECTION ( 'NONE',  ( 0.000000000000000000, 1.000000000000000000, 0.000000000000000000 ) ) ;
#12365 = EDGE_LOOP ( 'NONE', ( #12372, #21497, #2228, #219, #4263 ) ) ;
#12366 = CARTESIAN_POINT ( 'NONE',  ( -20.59660110919999809, -95.94970068810000896, -9.129820831349999111 ) ) ;
#12367 = CARTESIAN_POINT ( 'NONE',  ( 16.79023019859999977, -99.83167544280000527, 4.266711010680000804 ) ) ;
#12368 = CARTESIAN_POINT ( 'NONE',  ( 23.96865075879999907, -92.76843000840000286, -18.60167795649999789 ) ) ;
#12369 = DIRECTION ( 'NONE',  ( 1.000000000000000000, 0.000000000000000000, 0.000000000000000000 ) ) ;
#12370 = CARTESIAN_POINT ( 'NONE',  ( -2.674853241030000038E-13, -79.50000000000000000, 47.25000000000000000 ) ) ;
#12371 = CARTESIAN_POINT ( 'NONE',  ( 22.77479925683983453, -18.50000000000000000, 9.339609901686905857 ) ) ;
#12372 = ORIENTED_EDGE ( 'NONE', *, *, #5502, .F. ) ;
#12373 = LINE ( 'NONE', #10181, #20181 ) ;
#12374 = DIRECTION ( 'NONE',  ( 0.000000000000000000, 1.000000000000000000, 0.000000000000000000 ) ) ;
#12375 = CARTESIAN_POINT ( 'NONE',  ( 4.500000000000000000, -11.00000000000000000, 40.50000000000000000 ) ) ;
#12376 = CARTESIAN_POINT ( 'NONE',  ( 27.75394116159999669, -74.50000000000000000, -27.75394116159999669 ) ) ;
#12377 = CARTESIAN_POINT ( 'NONE',  ( -6.665307709260000379, -92.50000000000000000, -13.13558364449999871 ) ) ;
#12378 = B_SPLINE_CURVE_WITH_KNOTS ( 'NONE', 3,
 ( #17659, #28432, #28576, #13267 ),
 .UNSPECIFIED., .F., .F.,
 ( 4, 4 ),
 ( 0.000000000000000000, 1.000000000000000000 ),
 .UNSPECIFIED. ) ;
#12379 = DIRECTION ( 'NONE',  ( 0.000000000000000000, 1.000000000000000000, 0.000000000000000000 ) ) ;
#12380 = EDGE_CURVE ( 'NONE', #25468, #25683, #24613, .T. ) ;
#12381 = ADVANCED_FACE ( 'NONE', ( #6980 ), #21364, .F. ) ;
#12382 = ORIENTED_EDGE ( 'NONE', *, *, #9937, .T. ) ;
#12383 = CARTESIAN_POINT ( 'NONE',  ( 21.47202455769999929, -36.32770022289999901, -7.310015199259999541 ) ) ;
#12384 = CARTESIAN_POINT ( 'NONE',  ( 21.48170913309999719, -36.74612371620000317, -7.403099323020000178 ) ) ;
#12385 = DIRECTION ( 'NONE',  ( 0.000000000000000000, -1.000000000000000000, 0.000000000000000000 ) ) ;
#12386 = ADVANCED_FACE ( 'NONE', ( #7686 ), #17174, .T. ) ;
#12387 = EDGE_LOOP ( 'NONE', ( #7976, #5788, #117, #11313, #28149, #12838, #28375 ) ) ;
#12388 = CARTESIAN_POINT ( 'NONE',  ( 9.385332722619999402, -98.68450614990000247, 16.47661810339999988 ) ) ;
#12389 = EDGE_CURVE ( 'NONE', #27931, #19426, #7875, .T. ) ;
#12390 = CARTESIAN_POINT ( 'NONE',  ( -17.06978221569999832, -93.00000000760000773, -23.47580390800000316 ) ) ;
#12391 = CARTESIAN_POINT ( 'NONE',  ( 3.778421007439999979, -92.49999846069999876, 28.62986538160000194 ) ) ;
#12392 = CARTESIAN_POINT ( 'NONE',  ( 7.810721577829999873, -36.56420440790000015, -21.46720264389999855 ) ) ;
#12393 = DIRECTION ( 'NONE',  ( 0.000000000000000000, 1.000000000000000000, 0.000000000000000000 ) ) ;
#12394 = EDGE_LOOP ( 'NONE', ( #7244, #19318, #25091, #18133, #18661 ) ) ;
#12395 = CARTESIAN_POINT ( 'NONE',  ( 12.82719021566207473, -101.4304678898291172, -9.842949757285465395 ) ) ;
#12396 = CARTESIAN_POINT ( 'NONE',  ( 16.62464038829999780, -111.0000000000000000, 13.20435077039999960 ) ) ;
#12397 = CARTESIAN_POINT ( 'NONE',  ( 27.68682485439999752, -17.89999999999999858, 50.68039294919999804 ) ) ;
#12398 = ORIENTED_EDGE ( 'NONE', *, *, #1186, .F. ) ;
#12399 = CARTESIAN_POINT ( 'NONE',  ( 47.25000000000000000, -75.00000000000000000, -1.245115460929999944E-12 ) ) ;
#12400 = CARTESIAN_POINT ( 'NONE',  ( -14.76023875769999982, -74.50000000000000000, 45.51464203040000456 ) ) ;
#12401 = CARTESIAN_POINT ( 'NONE',  ( -14.65986943260000075, -74.43317772470001614, 36.47430876989999859 ) ) ;
#12402 = CARTESIAN_POINT ( 'NONE',  ( -2.184883600050000041, -19.44981017030000103, -22.64094073680000108 ) ) ;
#12403 = CARTESIAN_POINT ( 'NONE',  ( -17.06205513267597240, -92.82334897402063234, 25.28114489634798900 ) ) ;
#12404 = ORIENTED_EDGE ( 'NONE', *, *, #23716, .T. ) ;
#12405 = DIRECTION ( 'NONE',  ( 1.000000000000000000, 0.000000000000000000, 0.000000000000000000 ) ) ;
#12406 = CARTESIAN_POINT ( 'NONE',  ( 9.004237477329999351, -35.65077419509999146, -19.54737253879999770 ) ) ;
#12407 = CARTESIAN_POINT ( 'NONE',  ( 9.970358942569999883, -64.36570081249999475, -24.55403841179999702 ) ) ;
#12408 = CARTESIAN_POINT ( 'NONE',  ( 15.86628499849999940, -101.4334236450000049, 2.533787873950000158 ) ) ;
#12409 = CARTESIAN_POINT ( 'NONE',  ( 6.929578963970000061, -35.67530021650000549, -21.51138254459999999 ) ) ;
#12410 = EDGE_LOOP ( 'NONE', ( #1783, #10672, #15965, #18325 ) ) ;
#12411 = CARTESIAN_POINT ( 'NONE',  ( 6.525449878219999889, -99.97545561319999763, 15.58947632439999964 ) ) ;
#12412 = CARTESIAN_POINT ( 'NONE',  ( 15.01376502369999955, -101.1030539030000028, 3.591278379049999803 ) ) ;
#12413 = EDGE_CURVE ( 'NONE', #14792, #11909, #21268, .T. ) ;
#12414 = CARTESIAN_POINT ( 'NONE',  ( -11.57961683250000107, -94.58575303309999072, -20.85094915950000072 ) ) ;
#12415 = CARTESIAN_POINT ( 'NONE',  ( 7.872101281680000007, -35.50412903890000393, -21.29303334629999966 ) ) ;
#12416 = CARTESIAN_POINT ( 'NONE',  ( 6.161525631346291831, -92.49999999999998579, -29.87131533446021692 ) ) ;
#12417 = CARTESIAN_POINT ( 'NONE',  ( -8.015006079049999954, -99.64579499010000063, 15.35521677919999917 ) ) ;
#12418 = CARTESIAN_POINT ( 'NONE',  ( 8.320075280630000236, -93.86380869120000625, -23.56309038849999737 ) ) ;
#12419 = CIRCLE ( 'NONE', #3599, 5.500000000000000000 ) ;
#12420 = EDGE_CURVE ( 'NONE', #9643, #22, #5545, .T. ) ;
#12421 = CIRCLE ( 'NONE', #28703, 61.35000000000000142 ) ;
#12422 = CARTESIAN_POINT ( 'NONE',  ( -37.75000000000000000, -63.30468293320000583, 0.7216878364859999895 ) ) ;
#12423 = DIRECTION ( 'NONE',  ( 0.000000000000000000, 1.000000000000000000, 0.000000000000000000 ) ) ;
#12424 = VERTEX_POINT ( 'NONE', #22716 ) ;
#12425 = SURFACE_STYLE_USAGE ( .BOTH. , #8340 ) ;
#12426 = CARTESIAN_POINT ( 'NONE',  ( -5.582121642149999730, -100.8816835080000089, 14.77497840909999915 ) ) ;
#12427 = EDGE_LOOP ( 'NONE', ( #6274, #18370, #9888, #15289, #8841 ) ) ;
#12428 = AXIS2_PLACEMENT_3D ( 'NONE', #2042, #15256, #24468 ) ;
#12429 = DIRECTION ( 'NONE',  ( 1.000000000000000000, 0.000000000000000000, 0.000000000000000000 ) ) ;
#12430 = CARTESIAN_POINT ( 'NONE',  ( 0.1502068069240189152, -101.5526869445977667, -16.07314774595968743 ) ) ;
#12431 = CARTESIAN_POINT ( 'NONE',  ( -11.36637761219085974, -19.46558541313919122, 19.07288134243155042 ) ) ;
#12432 = DIRECTION ( 'NONE',  ( 0.000000000000000000, 1.000000000000000000, 0.000000000000000000 ) ) ;
#12433 = CARTESIAN_POINT ( 'NONE',  ( 27.18988201479999844, -29.29844555429999886, 49.77074518290000071 ) ) ;
#12434 = TOROIDAL_SURFACE ( 'NONE', #3615, 3.500000000000000000, 0.5000000000000000000 ) ;
#12435 = CARTESIAN_POINT ( 'NONE',  ( 15.45219090089999980, -100.9364576079999978, 3.957211818329999797 ) ) ;
#12436 = CARTESIAN_POINT ( 'NONE',  ( 26.54452309970000101, -74.08494070260000797, -28.96748645319999937 ) ) ;
#12437 = CARTESIAN_POINT ( 'NONE',  ( -22.51355778779999994, -71.15590230399999427, 17.45830423950000210 ) ) ;
#12438 = FACE_OUTER_BOUND ( 'NONE', #12365, .T. ) ;
#12439 = CARTESIAN_POINT ( 'NONE',  ( -19.05610772012959586, -19.48585536715970790, 13.96205032450363070 ) ) ;
#12440 = CARTESIAN_POINT ( 'NONE',  ( 7.745600378490000715, -35.22612198869999389, -21.28939742640000077 ) ) ;
#12441 = ORIENTED_EDGE ( 'NONE', *, *, #14572, .T. ) ;
#12442 = TOROIDAL_SURFACE ( 'NONE', #28722, 29.91857981989999971, 10.00000000000000000 ) ;
#12443 = VERTEX_POINT ( 'NONE', #2755 ) ;
#12444 = ADVANCED_FACE ( 'NONE', ( #11611 ), #592, .T. ) ;
#12445 = EDGE_CURVE ( 'NONE', #6367, #17644, #21812, .T. ) ;
#12446 = ORIENTED_EDGE ( 'NONE', *, *, #11200, .F. ) ;
#12447 = CARTESIAN_POINT ( 'NONE',  ( -2.349966181920000174, -58.68498324069999939, -24.40456951870000069 ) ) ;
#12448 = VECTOR ( 'NONE', #13727, 1000.000000000000000 ) ;
#12449 = CYLINDRICAL_SURFACE ( 'NONE', #28340, 7.250000000000004441 ) ;
#12450 = CARTESIAN_POINT ( 'NONE',  ( 21.23424069599999697, -35.30313414209999934, -7.936589188299999265 ) ) ;
#12451 = ADVANCED_FACE ( 'NONE', ( #12305 ), #25725, .T. ) ;
#12452 = ORIENTED_EDGE ( 'NONE', *, *, #6148, .F. ) ;
#12453 = LINE ( 'NONE', #23135, #18619 ) ;
#12454 = CARTESIAN_POINT ( 'NONE',  ( -7.600472224666014576, -74.00014642295832346, -38.79568063749085383 ) ) ;
#12455 = ORIENTED_EDGE ( 'NONE', *, *, #27753, .F. ) ;
#12456 = CARTESIAN_POINT ( 'NONE',  ( 7.356933064080000584, -36.56811125840000187, -21.47791245320000186 ) ) ;
#12457 = CYLINDRICAL_SURFACE ( 'NONE', #1557, 4.750000000000001776 ) ;
#12458 = CIRCLE ( 'NONE', #15755, 10.50000000000000000 ) ;
#12459 = CARTESIAN_POINT ( 'NONE',  ( -14.65665294340000102, -79.49999999100000991, 36.94583912339999898 ) ) ;
#12460 = CARTESIAN_POINT ( 'NONE',  ( -17.82598797839999705, -18.50000000000000000, 11.16764024010000078 ) ) ;
#12461 = CARTESIAN_POINT ( 'NONE',  ( -16.33619708059999809, -111.0000000000000000, 3.920288885250000188 ) ) ;
#12462 = CARTESIAN_POINT ( 'NONE',  ( -15.15090857039999861, -101.1124885629999994, 3.392036723980000001 ) ) ;
#12463 = CARTESIAN_POINT ( 'NONE',  ( 23.42789392040000251, -57.47571038070000782, 0.04069498556230000119 ) ) ;
#12464 = CARTESIAN_POINT ( 'NONE',  ( -20.24912682730000313, -60.33063645209999493, 14.55614817839999908 ) ) ;
#12465 = EDGE_CURVE ( 'NONE', #17023, #23155, #4621, .T. ) ;
#12466 = ORIENTED_EDGE ( 'NONE', *, *, #4107, .T. ) ;
#12467 = AXIS2_PLACEMENT_3D ( 'NONE', #4508, #13090, #24030 ) ;
#12468 = DIRECTION ( 'NONE',  ( -0.9704142011833034598, 0.000000000000000000, -0.2414462220490750932 ) ) ;
#12469 = CARTESIAN_POINT ( 'NONE',  ( 7.734359568749999525, -19.46510050329999686, -20.63161913629999944 ) ) ;
#12470 = CARTESIAN_POINT ( 'NONE',  ( -1.123994816189999746, -18.50000000000000000, -21.31890798069999704 ) ) ;
#12471 = CARTESIAN_POINT ( 'NONE',  ( 0.000000000000000000, -92.50000000000000000, 29.91857981989999971 ) ) ;
#12473 = VERTEX_POINT ( 'NONE', #27909 ) ;
#12472 = B_SPLINE_CURVE_WITH_KNOTS ( 'NONE', 5,
 ( #14104, #2749, #583, #27224, #11456, #27367, #16129, #7411, #5064 ),
 .UNSPECIFIED., .F., .F.,
 ( 6, 3, 6 ),
 ( -2.709627183969999908, -2.032180022599999969, 0.000000000000000000 ),
 .UNSPECIFIED. ) ;
#12474 = CARTESIAN_POINT ( 'NONE',  ( -18.78219790299999659, -19.46510053389999939, 11.52011550950000007 ) ) ;
#12475 = CARTESIAN_POINT ( 'NONE',  ( -41.88392290732132750, -65.74504297427023403, -1.085364455063224209 ) ) ;
#12476 = CARTESIAN_POINT ( 'NONE',  ( 36.44456167670000468, -80.16838065170000505, -14.57571988100000127 ) ) ;
#12477 = ORIENTED_EDGE ( 'NONE', *, *, #3383, .F. ) ;
#12478 = AXIS2_PLACEMENT_3D ( 'NONE', #15183, #10952, #2118 ) ;
#12479 = EDGE_CURVE ( 'NONE', #21398, #19169, #453, .T. ) ;
#12480 = ADVANCED_FACE ( 'NONE', ( #23812 ), #27881, .T. ) ;
#12481 = AXIS2_PLACEMENT_3D ( 'NONE', #16206, #13589, #810 ) ;
#12482 = CARTESIAN_POINT ( 'NONE',  ( -0.8937627406131904984, -79.83893697280288393, 47.19469876916298290 ) ) ;
#12483 = ORIENTED_EDGE ( 'NONE', *, *, #962, .T. ) ;
#12484 = CARTESIAN_POINT ( 'NONE',  ( 46.35082477299641113, -73.60002620146318009, -3.497084493779065273 ) ) ;
#12485 = VERTEX_POINT ( 'NONE', #10519 ) ;
#12486 = B_SPLINE_CURVE_WITH_KNOTS ( 'NONE', 3,
 ( #23848, #4170, #26034, #28216, #12613, #8250, #21525, #14941, #19340, #3888 ),
 .UNSPECIFIED., .F., .F.,
 ( 4, 2, 2, 2, 4 ),
 ( 0.000000000000000000, 0.2500000000000000000, 0.5000000000000000000, 0.7500000000000000000, 1.000000000000000000 ),
 .UNSPECIFIED. ) ;
#12487 = CARTESIAN_POINT ( 'NONE',  ( 20.77029242319999724, -55.05312981980000586, 10.65636466579999997 ) ) ;
#12488 = CARTESIAN_POINT ( 'NONE',  ( 20.33566493080000015, -36.00000000000000000, -9.885503730140001721 ) ) ;
#12489 = CARTESIAN_POINT ( 'NONE',  ( -7.432602092569998931, -73.95640471630001400, -39.04179453189999549 ) ) ;
#12490 = ORIENTED_EDGE ( 'NONE', *, *, #21359, .F. ) ;
#12491 = CARTESIAN_POINT ( 'NONE',  ( -3.528528669317067656, -97.24405583809684117, -20.51163445666866636 ) ) ;
#12492 = CARTESIAN_POINT ( 'NONE',  ( 19.55164490770000185, -35.69157978159999800, -9.020399939569999859 ) ) ;
#12493 = AXIS2_PLACEMENT_3D ( 'NONE', #20429, #17957, #6887 ) ;
#12494 = CARTESIAN_POINT ( 'NONE',  ( -43.20000000000000284, -63.07912966450000880, 0.1732050807559999961 ) ) ;
#12495 = CARTESIAN_POINT ( 'NONE',  ( 7.579179873580000226, -101.3235621230000021, 13.98627925510000125 ) ) ;
#12496 = CARTESIAN_POINT ( 'NONE',  ( -17.76804213369999985, -93.83763213849999829, 19.50200951540000105 ) ) ;
#12497 = ORIENTED_EDGE ( 'NONE', *, *, #2956, .T. ) ;
#12498 = AXIS2_PLACEMENT_3D ( 'NONE', #11322, #4790, #22573 ) ;
#12499 = CIRCLE ( 'NONE', #26018, 7.250000000000000000 ) ;
#12500 = CYLINDRICAL_SURFACE ( 'NONE', #19951, 7.250000000000004441 ) ;
#12501 = CARTESIAN_POINT ( 'NONE',  ( 18.39461646259999839, -98.93445099689999722, 3.291678619879999879 ) ) ;
#12502 = CARTESIAN_POINT ( 'NONE',  ( 2.798556025240000070E-15, -74.00000000000000000, 3.175502518160000051E-15 ) ) ;
#12503 = EDGE_CURVE ( 'NONE', #13839, #26488, #9204, .T. ) ;
#12504 = CARTESIAN_POINT ( 'NONE',  ( 23.83720300980000317, -93.60790942699999562, -8.962666302020000586 ) ) ;
#12505 = CARTESIAN_POINT ( 'NONE',  ( -0.5335602090409999887, -52.63293862069999562, -23.18581005440000098 ) ) ;
#12506 = AXIS2_PLACEMENT_3D ( 'NONE', #17797, #36, #10911 ) ;
#12507 = EDGE_CURVE ( 'NONE', #17829, #1871, #5021, .T. ) ;
#12508 = CARTESIAN_POINT ( 'NONE',  ( -3.730706918080000545, -79.99999997399999074, 46.61318877480000111 ) ) ;
#12509 = CARTESIAN_POINT ( 'NONE',  ( -2.619606055569999814, -19.50000000000000000, -24.29997775220000023 ) ) ;
#12510 = ORIENTED_EDGE ( 'NONE', *, *, #18989, .F. ) ;
#12511 = CARTESIAN_POINT ( 'NONE',  ( -15.36947826900000003, -101.0685828069999985, 4.769131590209999771 ) ) ;
#12512 = FACE_OUTER_BOUND ( 'NONE', #288, .T. ) ;
#12513 = DIRECTION ( 'NONE',  ( 1.000000000000000000, 0.000000000000000000, 0.000000000000000000 ) ) ;
#12514 = CARTESIAN_POINT ( 'NONE',  ( 30.15764098150000194, -74.11221873130000404, -25.07651571669999768 ) ) ;
#12515 = EDGE_CURVE ( 'NONE', #21652, #3233, #23196, .T. ) ;
#12516 = DIRECTION ( 'NONE',  ( 0.000000000000000000, -1.000000000000000000, 0.000000000000000000 ) ) ;
#12517 = TOROIDAL_SURFACE ( 'NONE', #11595, 38.75000000000000000, 0.5000000000000000000 ) ;
#12518 = VECTOR ( 'NONE', #27235, 1000.000000000000000 ) ;
#12519 = EDGE_LOOP ( 'NONE', ( #8992, #16130, #19469, #21806 ) ) ;
#12520 = CARTESIAN_POINT ( 'NONE',  ( 19.55068593369999874, -35.72724450179999423, -9.038647877299998967 ) ) ;
#12521 = VERTEX_POINT ( 'NONE', #1527 ) ;
#12522 = CARTESIAN_POINT ( 'NONE',  ( 19.55285847160000046, -35.83289739509999805, -9.107180759300000261 ) ) ;
#12523 = CARTESIAN_POINT ( 'NONE',  ( 7.635702898730000854, -101.6454117330000031, 14.06304778130000166 ) ) ;
#12524 = ORIENTED_EDGE ( 'NONE', *, *, #5885, .T. ) ;
#12525 = B_SPLINE_CURVE_WITH_KNOTS ( 'NONE', 3,
 ( #24559, #19883, #17719, #26603, #6645, #8953, #17864, #15507, #4598, #24417, #13475, #22381, #22675, #7234, #26903, #5034, #2719, #551, #20483, #2867, #24713, #20789, #11728, #9398, #16243, #13773, #18304, #15955, #11573, #7538 ),
 .UNSPECIFIED., .F., .F.,
 ( 4, 1, 1, 1, 1, 2, 2, 1, 1, 1, 1, 2, 2, 2, 1, 1, 1, 1, 2, 2, 4 ),
 ( 0.000000000000000000, 0.1249999999999861222, 0.1874999999999780731, 0.2187499999999731881, 0.2343749999999721334, 0.2421874999999739375, 0.2499999999999757416, 0.3749999999999756861, 0.4374999999999746869, 0.4687499999999725775, 0.4843749999999715228, 0.4921874999999713007, 0.4999999999999710232, 0.6249999999999793499, 0.6874999999999844569, 0.7187499999999875655, 0.7343749999999872324, 0.7421874999999861222, 0.7460937499999883427, 0.7499999999999905631, 1.000000000000000000 ),
 .UNSPECIFIED. ) ;
#12526 = CARTESIAN_POINT ( 'NONE',  ( -13.02193338449999871, -101.6484611580000035, -9.297634755529999850 ) ) ;
#12527 = CARTESIAN_POINT ( 'NONE',  ( -8.138356485639999249, -99.77922884479998800, 15.08989400399999958 ) ) ;
#12528 = CARTESIAN_POINT ( 'NONE',  ( -2.749191855459999889, -99.88544659679999427, -17.64021669569999773 ) ) ;
#12529 = CYLINDRICAL_SURFACE ( 'NONE', #16438, 2.000000000000001776 ) ;
#12530 = CARTESIAN_POINT ( 'NONE',  ( 11.70394544829403216, -98.37417905365539639, -16.31992250965110003 ) ) ;
#12531 = ORIENTED_EDGE ( 'NONE', *, *, #24534, .T. ) ;
#12532 = CARTESIAN_POINT ( 'NONE',  ( 13.30228833790079612, -100.9229461902416887, -9.872452464501236591 ) ) ;
#12533 = CARTESIAN_POINT ( 'NONE',  ( 27.68682485439999752, -24.80000000000000071, 50.68039294919999804 ) ) ;
#12534 = CARTESIAN_POINT ( 'NONE',  ( -27.68682485439999752, -25.10000000000000142, -50.68039294919999804 ) ) ;
#12535 = VERTEX_POINT ( 'NONE', #10234 ) ;
#12536 = CARTESIAN_POINT ( 'NONE',  ( 18.88171271619999914, -18.50000000000000000, -8.341252404190001357 ) ) ;
#12537 = CARTESIAN_POINT ( 'NONE',  ( -14.60455326470000159, -74.31496036839999419, 36.89972645289999775 ) ) ;
#12538 = LINE ( 'NONE', #19541, #22293 ) ;
#12539 = ORIENTED_EDGE ( 'NONE', *, *, #21552, .F. ) ;
#12541 = ADVANCED_FACE ( 'NONE', ( #19148 ), #5875, .T. ) ;
#12540 = AXIS2_PLACEMENT_3D ( 'NONE', #26973, #177, #20109 ) ;
#12542 = VECTOR ( 'NONE', #22533, 1000.000000000000000 ) ;
#12543 = CARTESIAN_POINT ( 'NONE',  ( 0.000000000000000000, -84.00000000000000000, 0.000000000000000000 ) ) ;
#12544 = B_SPLINE_CURVE_WITH_KNOTS ( 'NONE', 3,
 ( #6087, #23876, #10306, #12494 ),
 .UNSPECIFIED., .F., .F.,
 ( 4, 4 ),
 ( 0.000000000000000000, 1.000000000000000000 ),
 .UNSPECIFIED. ) ;
#12545 = CARTESIAN_POINT ( 'NONE',  ( 0.05051043905469999873, -101.1284992150000051, -15.40552557020000002 ) ) ;
#12546 = CARTESIAN_POINT ( 'NONE',  ( 9.605468207570000416, -64.60177787579999631, -24.16120251349999748 ) ) ;
#12547 = CARTESIAN_POINT ( 'NONE',  ( -39.45579440579999897, -74.12477399269999978, -7.440489808749999767 ) ) ;
#12548 = ADVANCED_FACE ( 'NONE', ( #28256 ), #9647, .F. ) ;
#12549 = CARTESIAN_POINT ( 'NONE',  ( 20.49658111199999766, -57.47855574479999774, 11.20865868970000001 ) ) ;
#12550 = CARTESIAN_POINT ( 'NONE',  ( -37.10038231309999901, -65.31510159580000163, 0.3466308900749999755 ) ) ;
#12551 = ORIENTED_EDGE ( 'NONE', *, *, #3910, .F. ) ;
#12552 = ADVANCED_FACE ( 'NONE', ( #26515 ), #12442, .F. ) ;
#12553 = B_SPLINE_CURVE_WITH_KNOTS ( 'NONE', 3,
 ( #8231, #17127, #18907, #21505, #3732, #27788, #26015, #18767, #14786, #27663 ),
 .UNSPECIFIED., .F., .F.,
 ( 4, 2, 2, 2, 4 ),
 ( 0.000000000000000000, 0.2500000000000000000, 0.5000000000000000000, 0.7500000000000000000, 1.000000000000000000 ),
 .UNSPECIFIED. ) ;
#12554 = CARTESIAN_POINT ( 'NONE',  ( 6.072376808220000477, -100.9137139110000021, 14.40534646189999890 ) ) ;
#12555 = CARTESIAN_POINT ( 'NONE',  ( 15.63748056140000209, -101.6484611540000031, 3.386620984279999913 ) ) ;
#12556 = DIRECTION ( 'NONE',  ( -0.3687499999999814260, 0.000000000000000000, 0.9295286103719527793 ) ) ;
#12557 = CARTESIAN_POINT ( 'NONE',  ( 24.05168182727625847, -63.71467881788436927, 10.72464045306219660 ) ) ;
#12558 = DIRECTION ( 'NONE',  ( 0.000000000000000000, -1.000000000000000000, 0.000000000000000000 ) ) ;
#12559 = TOROIDAL_SURFACE ( 'NONE', #16307, 55.85192378860000417, 0.3499999999999999778 ) ;
#12560 = CARTESIAN_POINT ( 'NONE',  ( 0.000000000000000000, -86.00000000000000000, 0.000000000000000000 ) ) ;
#12561 = CARTESIAN_POINT ( 'NONE',  ( 8.649323485130000932, -94.16309976680000204, -22.83302821760000256 ) ) ;
#12562 = CIRCLE ( 'NONE', #1006, 7.249999999999999112 ) ;
#12563 = TOROIDAL_SURFACE ( 'NONE', #22367, 6.750000000000000000, 0.5000000000000000000 ) ;
#12564 = CARTESIAN_POINT ( 'NONE',  ( 21.21808873300000187, -34.59820414320000026, -7.670973475509999417 ) ) ;
#12565 = CARTESIAN_POINT ( 'NONE',  ( -13.26856174610000139, -93.91547326100000248, -20.89962974999999901 ) ) ;
#12566 = CARTESIAN_POINT ( 'NONE',  ( -6.781378104809999030, -101.6484611540000031, 14.49182221120000058 ) ) ;
#12567 = EDGE_LOOP ( 'NONE', ( #3907, #24496, #27242, #26882 ) ) ;
#12568 = DIRECTION ( 'NONE',  ( 1.000000000000000000, 0.000000000000000000, 0.000000000000000000 ) ) ;
#12569 = ORIENTED_EDGE ( 'NONE', *, *, #4441, .T. ) ;
#12570 = EDGE_LOOP ( 'NONE', ( #23900, #10918, #2093, #6376, #17173, #10995, #13389 ) ) ;
#12571 = CARTESIAN_POINT ( 'NONE',  ( -0.8744470429980000237, -101.1848541600000004, -15.25816383929999986 ) ) ;
#12572 = CARTESIAN_POINT ( 'NONE',  ( 7.286238495500000134, -101.2500498790000023, 13.33737010350000141 ) ) ;
#12573 = CARTESIAN_POINT ( 'NONE',  ( 13.13193815604943460, -92.93978723899418526, 27.52821129672017264 ) ) ;
#12574 = DIRECTION ( 'NONE',  ( 0.000000000000000000, 0.000000000000000000, -1.000000000000000000 ) ) ;
#12575 = CARTESIAN_POINT ( 'NONE',  ( 27.75394116159999669, -74.50000000000000000, -27.75394116159999669 ) ) ;
#12576 = EDGE_CURVE ( 'NONE', #4271, #13019, #19656, .T. ) ;
#12577 = DIRECTION ( 'NONE',  ( 1.000000000000000000, 0.000000000000000000, 0.000000000000000000 ) ) ;
#12578 = DIRECTION ( 'NONE',  ( 0.000000000000000000, 1.000000000000000000, 0.000000000000000000 ) ) ;
#12579 = CARTESIAN_POINT ( 'NONE',  ( -11.92913933939999893, -65.75576304719999143, -23.66118000710000047 ) ) ;
#12580 = CARTESIAN_POINT ( 'NONE',  ( 7.049162148299999764, -36.56981899800000235, -21.51316774079999661 ) ) ;
#12581 = CARTESIAN_POINT ( 'NONE',  ( -10.31531692359999930, -18.50000000000000000, 18.33249795759999756 ) ) ;
#12582 = CIRCLE ( 'NONE', #6072, 9.500000000000001776 ) ;
#12583 = ORIENTED_EDGE ( 'NONE', *, *, #28496, .T. ) ;
#12584 = B_SPLINE_CURVE_WITH_KNOTS ( 'NONE', 5,
 ( #24786, #26377, #15582, #15427, #6405, #22157, #2059, #17640, #17787 ),
 .UNSPECIFIED., .F., .F.,
 ( 6, 3, 6 ),
 ( 0.000000000000000000, 0.5000000000000000000, 1.000000000000000000 ),
 .UNSPECIFIED. ) ;
#12585 = AXIS2_PLACEMENT_3D ( 'NONE', #11027, #169, #17925 ) ;
#12586 = EDGE_CURVE ( 'NONE', #1954, #14463, #2704, .T. ) ;
#12587 = AXIS2_PLACEMENT_3D ( 'NONE', #27164, #7202, #16068 ) ;
#12588 = VERTEX_POINT ( 'NONE', #9608 ) ;
#12589 = CARTESIAN_POINT ( 'NONE',  ( 22.27494768480000076, -37.97325501589999419, -9.063917176249999486 ) ) ;
#12590 = CARTESIAN_POINT ( 'NONE',  ( -2.596377074909999916, -62.44588796569999545, -25.54838417140000217 ) ) ;
#12591 = CARTESIAN_POINT ( 'NONE',  ( -29.69641156999999865, -92.84292833370000153, 6.354845228289999426 ) ) ;
#12592 = CARTESIAN_POINT ( 'NONE',  ( 9.397459420459995272, -94.89420224095998435, -22.59846300103535199 ) ) ;
#12593 = CARTESIAN_POINT ( 'NONE',  ( 19.65745263667615816, -19.48583448325832634, -8.821903065879004302 ) ) ;
#12594 = ORIENTED_EDGE ( 'NONE', *, *, #3588, .F. ) ;
#12595 = CARTESIAN_POINT ( 'NONE',  ( -17.90995366394907862, -97.42330309962233059, -10.14262162657689359 ) ) ;
#12596 = FACE_OUTER_BOUND ( 'NONE', #26214, .T. ) ;
#12597 = VERTEX_POINT ( 'NONE', #13694 ) ;
#12598 = CIRCLE ( 'NONE', #24740, 15.19391340349999986 ) ;
#12599 = DIRECTION ( 'NONE',  ( 0.000000000000000000, -1.000000000000000000, 0.000000000000000000 ) ) ;
#12600 = AXIS2_PLACEMENT_3D ( 'NONE', #5289, #946, #5568 ) ;
#12601 = ORIENTED_EDGE ( 'NONE', *, *, #27187, .F. ) ;
#12602 = AXIS2_PLACEMENT_3D ( 'NONE', #17842, #26738, #15635 ) ;
#12603 = CARTESIAN_POINT ( 'NONE',  ( -14.34007285459999892, -80.00000123130000418, 37.07570051250000631 ) ) ;
#12604 = EDGE_CURVE ( 'NONE', #26971, #12597, #2155, .T. ) ;
#12605 = CARTESIAN_POINT ( 'NONE',  ( -22.22906645670000003, -74.50000000000000000, -32.83566817450000030 ) ) ;
#12606 = EDGE_CURVE ( 'NONE', #27953, #20968, #24078, .T. ) ;
#12607 = CARTESIAN_POINT ( 'NONE',  ( 22.14119312130000239, -18.50000000000000000, 8.928410838750000522 ) ) ;
#12608 = CARTESIAN_POINT ( 'NONE',  ( -32.47338858185761268, -74.10435492515816236, -22.14149567788639317 ) ) ;
#12609 = DIRECTION ( 'NONE',  ( 0.000000000000000000, -1.000000000000000000, 0.000000000000000000 ) ) ;
#12610 = EDGE_LOOP ( 'NONE', ( #21954, #19586, #24998, #18477 ) ) ;
#12611 = CARTESIAN_POINT ( 'NONE',  ( 24.78974732560000405, -64.24504771300000527, -10.08508462690000052 ) ) ;
#12612 = CARTESIAN_POINT ( 'NONE',  ( -12.36343567480000161, -101.1716782170000073, -9.731652660190000859 ) ) ;
#12613 = CARTESIAN_POINT ( 'NONE',  ( 22.01067795732654275, -93.33134965528456917, 15.58958953133906000 ) ) ;
#12614 = CARTESIAN_POINT ( 'NONE',  ( -7.679489405794825529, -100.9609609849295424, 14.64415966093239874 ) ) ;
#12615 = EDGE_LOOP ( 'NONE', ( #3516, #10823 ) ) ;
#12616 = ADVANCED_FACE ( 'NONE', ( #3214 ), #9887, .T. ) ;
#12617 = AXIS2_PLACEMENT_3D ( 'NONE', #3565, #12423, #838 ) ;
#12618 = CARTESIAN_POINT ( 'NONE',  ( -41.53002200404621647, -65.11500191528324422, -2.884225231620696661 ) ) ;
#12619 = CARTESIAN_POINT ( 'NONE',  ( -31.89935321680000158, -74.00000000000000000, -21.99985828019999801 ) ) ;
#12620 = CARTESIAN_POINT ( 'NONE',  ( 36.39191644179999940, -79.45170616170001665, -14.80043607370000025 ) ) ;
#12621 = ORIENTED_EDGE ( 'NONE', *, *, #1592, .F. ) ;
#12622 = TOROIDAL_SURFACE ( 'NONE', #5661, 3.500000000000000000, 0.5000000000000000000 ) ;
#12623 = CARTESIAN_POINT ( 'NONE',  ( 6.671273368871432297, -100.8738282931630863, 15.20505492520185875 ) ) ;
#12624 = CARTESIAN_POINT ( 'NONE',  ( 11.77387480661665187, -101.1586404113069335, -10.29001710982078777 ) ) ;
#12625 = EDGE_LOOP ( 'NONE', ( #2604, #18256, #1047, #27676 ) ) ;
#12626 = CARTESIAN_POINT ( 'NONE',  ( 46.01499598271041691, -73.50000000000001421, -4.057494375605252834 ) ) ;
#12627 = ORIENTED_EDGE ( 'NONE', *, *, #9124, .T. ) ;
#12628 = CARTESIAN_POINT ( 'NONE',  ( 21.63571023749999966, -57.45864773929999814, 10.20337500120000129 ) ) ;
#12629 = CARTESIAN_POINT ( 'NONE',  ( -23.77081188420000046, -111.0000000000000000, -19.11016751280000037 ) ) ;
#12630 = CARTESIAN_POINT ( 'NONE',  ( -7.268571389559999929, -74.08839659379999887, -39.96417052329999819 ) ) ;
#12631 = VERTEX_POINT ( 'NONE', #14136 ) ;
#12632 = DIRECTION ( 'NONE',  ( 0.5301416321220551175, 0.000000000000000000, 0.8479091047340886478 ) ) ;
#12633 = FACE_OUTER_BOUND ( 'NONE', #17814, .T. ) ;
#12634 = CARTESIAN_POINT ( 'NONE',  ( -30.34790777679999962, -93.00000000000000000, 3.042119914239999723 ) ) ;
#12635 = CARTESIAN_POINT ( 'NONE',  ( 20.98778206287693493, -96.61062616032549499, -3.223209917027987093 ) ) ;
#12636 = AXIS2_PLACEMENT_3D ( 'NONE', #6106, #21994, #19236 ) ;
#12637 = CARTESIAN_POINT ( 'NONE',  ( -18.17993916029999824, -94.51629284240000572, 17.35042103430000182 ) ) ;
#12638 = ORIENTED_EDGE ( 'NONE', *, *, #8477, .F. ) ;
#12639 = CARTESIAN_POINT ( 'NONE',  ( -16.85779618499999799, -97.58045781630001159, -10.78314124750000147 ) ) ;
#12640 = ADVANCED_FACE ( 'NONE', ( #11487 ), #23034, .T. ) ;
#12641 = CARTESIAN_POINT ( 'NONE',  ( 12.82866288339999983, -100.7707614970000094, -9.316536369119999605 ) ) ;
#12642 = DIRECTION ( 'NONE',  ( 0.8775825618903722036, 0.000000000000000000, -0.4794255386042041156 ) ) ;
#12643 = CARTESIAN_POINT ( 'NONE',  ( 23.73696482120000084, -93.59856727309998803, -8.983699850290001621 ) ) ;
#12644 = VERTEX_POINT ( 'NONE', #22892 ) ;
#12645 = CARTESIAN_POINT ( 'NONE',  ( -38.29487672305123169, -65.09473114940418270, 2.826095656349198570 ) ) ;
#12646 = CARTESIAN_POINT ( 'NONE',  ( -44.38791280949999418, -69.00000000000000000, -2.397127693020000283 ) ) ;
#12647 = ORIENTED_EDGE ( 'NONE', *, *, #23406, .T. ) ;
#12648 = CARTESIAN_POINT ( 'NONE',  ( 34.06016921999999880, -74.00000000000000000, -13.75000000000000000 ) ) ;
#12649 = CARTESIAN_POINT ( 'NONE',  ( 11.86655840719999944, -101.1889999979999999, -11.10431293650000129 ) ) ;
#12650 = CARTESIAN_POINT ( 'NONE',  ( 27.18988201479999844, -20.30155444569999901, 49.77074518290000071 ) ) ;
#12651 = CARTESIAN_POINT ( 'NONE',  ( -1.013078509969999973E-15, -101.6484611540000031, -5.329070518200000398E-15 ) ) ;
#12652 = CARTESIAN_POINT ( 'NONE',  ( -27.68682485439999752, -35.29999999999999716, -50.68039294919999804 ) ) ;
#12653 = VECTOR ( 'NONE', #1246, 1000.000000000000000 ) ;
#12654 = AXIS2_PLACEMENT_3D ( 'NONE', #20406, #7302, #20996 ) ;
#12655 = DIRECTION ( 'NONE',  ( 9.280770596480004008E-17, 0.000000000000000000, -1.000000000000000000 ) ) ;
#12656 = TOROIDAL_SURFACE ( 'NONE', #26642, 6.750000000000000000, 0.5000000000000000000 ) ;
#12657 = VERTEX_POINT ( 'NONE', #11638 ) ;
#12658 = EDGE_CURVE ( 'NONE', #25468, #19780, #12902, .T. ) ;
#12659 = LINE ( 'NONE', #1627, #4730 ) ;
#12660 = CARTESIAN_POINT ( 'NONE',  ( 21.38475920739999836, -35.91217828539999601, -7.828362488440000710 ) ) ;
#12661 = VERTEX_POINT ( 'NONE', #13984 ) ;
#12662 = CARTESIAN_POINT ( 'NONE',  ( 21.49488803819999916, -36.89279931859999806, -7.765148297399999677 ) ) ;
#12663 = CARTESIAN_POINT ( 'NONE',  ( 7.599202867396026129, -18.61794787490824277, -20.27108518235802137 ) ) ;
#12664 = ORIENTED_EDGE ( 'NONE', *, *, #26640, .F. ) ;
#12665 = CARTESIAN_POINT ( 'NONE',  ( -12.98104160269999952, -101.4254868690000109, -9.301111302380000723 ) ) ;
#12666 = B_SPLINE_SURFACE_WITH_KNOTS ( 'NONE', 5, 5, ( 
 ( #13763, #2705, #16230, #247, #18290, #27180 ),
 ( #11864, #2414, #11560, #6781, #4587, #5022 ),
 ( #25142, #16087, #22964, #13910, #20627, #14057 ),
 ( #9673, #5175, #15791, #3006, #20775, #13612 ),
 ( #26889, #22522, #831, #18584, #15643, #24701 ),
 ( #4735, #24547, #13462, #11267, #20176, #9090 ) ),
 .UNSPECIFIED., .F., .F., .F.,
 ( 6, 6 ),
 ( 6, 6 ),
 ( 9.718751496520001254, 14.66109853230000049 ),
 ( 0.000000000000000000, 2.000000000000000000 ),
 .UNSPECIFIED. ) ;
#12667 = CARTESIAN_POINT ( 'NONE',  ( -9.348798002780000616, -10.50000000000000000, -17.11285995690000306 ) ) ;
#12668 = CARTESIAN_POINT ( 'NONE',  ( -8.046121148190000127, -99.85455315880000171, 15.13041121020000013 ) ) ;
#12669 = ORIENTED_EDGE ( 'NONE', *, *, #22616, .F. ) ;
#12670 = DIRECTION ( 'NONE',  ( 0.000000000000000000, 1.000000000000000000, 0.000000000000000000 ) ) ;
#12671 = CIRCLE ( 'NONE', #23857, 57.75000000000000000 ) ;
#12672 = CARTESIAN_POINT ( 'NONE',  ( 8.563702697320000112, -53.27760474060000462, -22.19980545599999999 ) ) ;
#12673 = LINE ( 'NONE', #26386, #16707 ) ;
#12674 = ORIENTED_EDGE ( 'NONE', *, *, #11452, .F. ) ;
#12675 = CARTESIAN_POINT ( 'NONE',  ( 12.51632808644059836, -101.6297509123139235, -9.990436032579999903 ) ) ;
#12676 = CARTESIAN_POINT ( 'NONE',  ( 22.30116796419999758, -27.06785567060000020, -0.1709765798629999944 ) ) ;
#12677 = CARTESIAN_POINT ( 'NONE',  ( 22.98572682540000045, -65.40406720010000186, 11.05257029390000056 ) ) ;
#12678 = CARTESIAN_POINT ( 'NONE',  ( 8.920182828499999772, -94.54719592040000009, -22.12534720020000023 ) ) ;
#12679 = ORIENTED_EDGE ( 'NONE', *, *, #1413, .F. ) ;
#12680 = B_SPLINE_CURVE_WITH_KNOTS ( 'NONE', 3,
 ( #16503, #14723, #25676, #14587, #27731, #23346 ),
 .UNSPECIFIED., .F., .F.,
 ( 4, 2, 4 ),
 ( 0.000000000000000000, 0.5000000000000000000, 1.000000000000000000 ),
 .UNSPECIFIED. ) ;
#12681 = DIRECTION ( 'NONE',  ( 0.3790931394101558771, -0.6121731929912518355, 0.6939253370752848094 ) ) ;
#12682 = CIRCLE ( 'NONE', #15007, 0.4999999999999981126 ) ;
#12683 = CARTESIAN_POINT ( 'NONE',  ( -14.18001136240000015, -74.03309514170000227, 36.27836971480000017 ) ) ;
#12684 = CARTESIAN_POINT ( 'NONE',  ( -17.55208023420000174, -93.64386272749999307, 18.16437695980000200 ) ) ;
#12685 = DIRECTION ( 'NONE',  ( 0.7748485350940619298, 0.000000000000000000, -0.6321469351840490747 ) ) ;
#12686 = ORIENTED_EDGE ( 'NONE', *, *, #18731, .F. ) ;
#12687 = CARTESIAN_POINT ( 'NONE',  ( 12.61209325099999923, -111.0000000000000000, -11.02259514940000074 ) ) ;
#12688 = DIRECTION ( 'NONE',  ( 0.8775825618903722036, 0.000000000000000000, -0.4794255386042041156 ) ) ;
#12689 = CARTESIAN_POINT ( 'NONE',  ( -13.18754275750000104, -69.02891040180000459, -23.50545369980000032 ) ) ;
#12690 = CARTESIAN_POINT ( 'NONE',  ( 21.69654716690000029, -58.73757401350000151, 10.24315597560000057 ) ) ;
#12691 = CARTESIAN_POINT ( 'NONE',  ( -11.58786380919999992, -27.06642317520000063, -19.05189997919999811 ) ) ;
#12692 = EDGE_LOOP ( 'NONE', ( #5271, #17128, #27257, #7724 ) ) ;
#12693 = CARTESIAN_POINT ( 'NONE',  ( 6.968069840630000122, -100.0482783049999966, 15.72019133129999879 ) ) ;
#12694 = CARTESIAN_POINT ( 'NONE',  ( 15.36147648729999915, -101.1716782170000073, 3.403622381159999932 ) ) ;
#12695 = CIRCLE ( 'NONE', #6196, 3.000000000000002665 ) ;
#12696 = CARTESIAN_POINT ( 'NONE',  ( -7.879410208250000380, -99.92967571559999840, 15.46934584979999983 ) ) ;
#12697 = EDGE_CURVE ( 'NONE', #15179, #21477, #10430, .T. ) ;
#12698 = CARTESIAN_POINT ( 'NONE',  ( -39.80580048936597137, -65.72850285331089992, -2.193980430793042391 ) ) ;
#12699 = CARTESIAN_POINT ( 'NONE',  ( 21.40257419309999776, -18.50000000000000000, 0.9664833869290000434 ) ) ;
#12700 = LINE ( 'NONE', #15165, #24660 ) ;
#12701 = VERTEX_POINT ( 'NONE', #23719 ) ;
#12702 = TOROIDAL_SURFACE ( 'NONE', #16915, 5.500000000000000000, 0.5000000000000000000 ) ;
#12703 = CARTESIAN_POINT ( 'NONE',  ( 4.742489832159999530, -92.98926436760000058, -27.98920360839999688 ) ) ;
#12704 = EDGE_CURVE ( 'NONE', #19645, #12804, #21127, .T. ) ;
#12705 = DIRECTION ( 'NONE',  ( 0.000000000000000000, 1.000000000000000000, 0.000000000000000000 ) ) ;
#12706 = CARTESIAN_POINT ( 'NONE',  ( -6.768220873529999793, -101.4254868729999970, 14.46370517449999937 ) ) ;
#12707 = VERTEX_POINT ( 'NONE', #10023 ) ;
#12708 = FACE_OUTER_BOUND ( 'NONE', #2108, .T. ) ;
#12709 = CARTESIAN_POINT ( 'NONE',  ( -12.56985916528515190, -100.9570234915280338, -10.74835527338169427 ) ) ;
#12710 = ORIENTED_EDGE ( 'NONE', *, *, #4298, .T. ) ;
#12711 = EDGE_CURVE ( 'NONE', #21689, #21931, #18936, .T. ) ;
#12712 = ADVANCED_FACE ( 'NONE', ( #28224, #23305 ), #27819, .T. ) ;
#12713 = CARTESIAN_POINT ( 'NONE',  ( 0.000000000000000000, -39.50000000000000000, 0.000000000000000000 ) ) ;
#12714 = AXIS2_PLACEMENT_3D ( 'NONE', #17330, #12790, #10588 ) ;
#12715 = DIRECTION ( 'NONE',  ( 0.4794255386042033384, 0.000000000000000000, 0.8775825618903726477 ) ) ;
#12716 = VECTOR ( 'NONE', #19611, 1000.000000000000000 ) ;
#12717 = CARTESIAN_POINT ( 'NONE',  ( -13.18688177930000016, -93.32822605769999313, -23.58441486170000090 ) ) ;
#12718 = DIRECTION ( 'NONE',  ( 0.000000000000000000, -1.000000000000000000, 0.000000000000000000 ) ) ;
#12719 = CARTESIAN_POINT ( 'NONE',  ( 16.34567793506732869, -94.63270597576601517, 17.22370556663485175 ) ) ;
#12720 = CARTESIAN_POINT ( 'NONE',  ( -22.19764394599999946, -69.10489204579999978, 16.61088088690000220 ) ) ;
#12721 = CARTESIAN_POINT ( 'NONE',  ( -31.00000000000000000, -11.00000000000000000, 4.500000000000000000 ) ) ;
#12722 = CARTESIAN_POINT ( 'NONE',  ( -19.55651890851374475, -19.49660179764862633, 14.34605571524100043 ) ) ;
#12723 = CIRCLE ( 'NONE', #4856, 11.00000000000000000 ) ;
#12724 = CARTESIAN_POINT ( 'NONE',  ( 7.120076906740000489, -35.74888742009999731, -21.45961752960000268 ) ) ;
#12725 = CARTESIAN_POINT ( 'NONE',  ( -26.69293917519999937, -34.10310889129999623, -48.86109741659999628 ) ) ;
#12726 = ORIENTED_EDGE ( 'NONE', *, *, #20297, .F. ) ;
#12727 = VERTEX_POINT ( 'NONE', #1311 ) ;
#12728 = CARTESIAN_POINT ( 'NONE',  ( -38.55000000000000426, -63.07912966450000880, 2.857883832489999776 ) ) ;
#12729 = VERTEX_POINT ( 'NONE', #8133 ) ;
#12730 = CARTESIAN_POINT ( 'NONE',  ( -0.8504652179830000103, -58.79428935229999098, -23.42987164899999897 ) ) ;
#12731 = AXIS2_PLACEMENT_3D ( 'NONE', #15658, #20643, #20190 ) ;
#12732 = CARTESIAN_POINT ( 'NONE',  ( 9.393614097370001303, -37.99999999279999230, -22.97877291159999658 ) ) ;
#12733 = CARTESIAN_POINT ( 'NONE',  ( -29.38881566890000130, -92.76004107139999633, 4.720288864379999616 ) ) ;
#12734 = DIRECTION ( 'NONE',  ( 0.4794255386042041156, 0.000000000000000000, 0.8775825618903720926 ) ) ;
#12735 = CARTESIAN_POINT ( 'NONE',  ( -19.54048411320001222, -52.63055504210016267, 12.61913916920000034 ) ) ;
#12736 = EDGE_CURVE ( 'NONE', #21778, #6019, #18151, .T. ) ;
#12737 = EDGE_LOOP ( 'NONE', ( #2670, #24778, #23696, #26638, #17979, #7519, #27415 ) ) ;
#12738 = CARTESIAN_POINT ( 'NONE',  ( -18.87800995732253995, -96.89152198193129095, -9.790682212865581491 ) ) ;
#12739 = CARTESIAN_POINT ( 'NONE',  ( 10.20110288159999890, -82.25000000000000000, -41.00000000000000000 ) ) ;
#12740 = ORIENTED_EDGE ( 'NONE', *, *, #15889, .T. ) ;
#12741 = CIRCLE ( 'NONE', #1182, 0.5000000000000009992 ) ;
#12742 = DIRECTION ( 'NONE',  ( 1.000000000000000000, 0.000000000000000000, 0.000000000000000000 ) ) ;
#12743 = EDGE_CURVE ( 'NONE', #1488, #28309, #8724, .T. ) ;
#12744 = EDGE_LOOP ( 'NONE', ( #3533, #23499, #4000, #22488 ) ) ;
#12745 = CIRCLE ( 'NONE', #10882, 0.5000000000000012212 ) ;
#12746 = CARTESIAN_POINT ( 'NONE',  ( -17.93028678539999987, -18.50000000000000000, 10.99759328500000066 ) ) ;
#12747 = CARTESIAN_POINT ( 'NONE',  ( -15.32098868920000001, -101.1716782350000017, 3.581867792729999778 ) ) ;
#12748 = DIRECTION ( 'NONE',  ( 1.000000000000000000, 0.000000000000000000, 0.000000000000000000 ) ) ;
#12749 = CARTESIAN_POINT ( 'NONE',  ( 11.12836528380000090, -101.0356131030000029, -10.75380786670000077 ) ) ;
#12750 = ORIENTED_EDGE ( 'NONE', *, *, #7964, .F. ) ;
#12751 = CIRCLE ( 'NONE', #13240, 55.67692378859999991 ) ;
#12752 = CARTESIAN_POINT ( 'NONE',  ( -12.55296505889999992, -100.8088109309999965, -10.78431163630000000 ) ) ;
#12753 = CARTESIAN_POINT ( 'NONE',  ( -5.679770007689999289, -79.50000000000000000, 47.25000000000000000 ) ) ;
#12754 = DIRECTION ( 'NONE',  ( 0.8775825618903722036, 0.000000000000000000, -0.4794255386042041156 ) ) ;
#12755 = EDGE_LOOP ( 'NONE', ( #14455, #6202, #26036, #16275 ) ) ;
#12756 = CARTESIAN_POINT ( 'NONE',  ( -0.9692006007005103951, -101.5902664364219277, -16.01432838750588061 ) ) ;
#12757 = CARTESIAN_POINT ( 'NONE',  ( -32.63753603780000390, -74.26163306789999297, -22.10337284230000066 ) ) ;
#12758 = CARTESIAN_POINT ( 'NONE',  ( 36.29172732829999859, -79.00000000000000000, -14.94947765220000058 ) ) ;
#12759 = ORIENTED_EDGE ( 'NONE', *, *, #1960, .F. ) ;
#12760 = AXIS2_PLACEMENT_3D ( 'NONE', #25302, #16823, #7799 ) ;
#12761 = EDGE_CURVE ( 'NONE', #25949, #87, #8397, .T. ) ;
#12762 = CARTESIAN_POINT ( 'NONE',  ( 6.667714868184677179, -101.2021794473701988, 14.92458339438100801 ) ) ;
#12763 = CARTESIAN_POINT ( 'NONE',  ( -0.8970218170808564873, -79.84013848330904750, 47.19429349399515417 ) ) ;
#12764 = ORIENTED_EDGE ( 'NONE', *, *, #23078, .F. ) ;
#12765 = EDGE_CURVE ( 'NONE', #22592, #20540, #423, .T. ) ;
#12766 = CARTESIAN_POINT ( 'NONE',  ( -12.22902281399961844, -69.69726684069728151, -24.77074626774463084 ) ) ;
#12767 = DIRECTION ( 'NONE',  ( 0.000000000000000000, -1.000000000000000000, 0.000000000000000000 ) ) ;
#12768 = ORIENTED_EDGE ( 'NONE', *, *, #18470, .F. ) ;
#12769 = AXIS2_PLACEMENT_3D ( 'NONE', #13680, #18055, #5088 ) ;
#12770 = CARTESIAN_POINT ( 'NONE',  ( 22.81627243510000014, -54.99674360790000094, 10.21013232080000144 ) ) ;
#12771 = CARTESIAN_POINT ( 'NONE',  ( -38.25764126207506877, -63.06523941402393518, 2.751386478887667408 ) ) ;
#12772 = CARTESIAN_POINT ( 'NONE',  ( -7.367397733560000717, -74.05254684259999465, -39.49475000900000765 ) ) ;
#12773 = EDGE_LOOP ( 'NONE', ( #17103, #1874, #21903, #24235 ) ) ;
#12774 = CARTESIAN_POINT ( 'NONE',  ( -3.371331056789452774, -97.34036579176134296, -20.41252770651184179 ) ) ;
#12775 = DIRECTION ( 'NONE',  ( 1.000000000000000000, 0.000000000000000000, 0.000000000000000000 ) ) ;
#12776 = EDGE_CURVE ( 'NONE', #10585, #8240, #11146, .T. ) ;
#12777 = VERTEX_POINT ( 'NONE', #15091 ) ;
#12778 = CARTESIAN_POINT ( 'NONE',  ( 9.136262649109999856, -36.24018116499999564, -21.32348944479999986 ) ) ;
#12779 = CARTESIAN_POINT ( 'NONE',  ( -22.02936738240000025, -92.83702889919999279, -20.06351774230000373 ) ) ;
#12780 = CARTESIAN_POINT ( 'NONE',  ( -3.638844514300000110, -18.50000000000000000, -24.22839726010000305 ) ) ;
#12781 = EDGE_LOOP ( 'NONE', ( #14819, #2659, #25720, #21355 ) ) ;
#12782 = CARTESIAN_POINT ( 'NONE',  ( -13.27621816679999966, -99.83167544280000527, -11.12918164819999944 ) ) ;
#12783 = CARTESIAN_POINT ( 'NONE',  ( 12.16870387880000060, -101.1030539030000028, -9.499108720959998919 ) ) ;
#12784 = DIRECTION ( 'NONE',  ( 0.000000000000000000, -1.000000000000000000, 0.000000000000000000 ) ) ;
#12785 = CARTESIAN_POINT ( 'NONE',  ( 23.81109335309999864, -94.64125147549999895, -7.489946264089999417 ) ) ;
#12786 = CARTESIAN_POINT ( 'NONE',  ( -0.8454043835150000241, -53.84414347720000649, -23.22093481959999650 ) ) ;
#12787 = CARTESIAN_POINT ( 'NONE',  ( 29.84209778924876844, -92.58608763743339409, 6.300736884733585619 ) ) ;
#12788 = CARTESIAN_POINT ( 'NONE',  ( -38.25000000000000000, -65.14977478849999670, -2.684678751729999480 ) ) ;
#12789 = ORIENTED_EDGE ( 'NONE', *, *, #20503, .F. ) ;
#12790 = DIRECTION ( 'NONE',  ( 0.000000000000000000, 1.000000000000000000, 0.000000000000000000 ) ) ;
#12791 = DIRECTION ( 'NONE',  ( -0.8775825618903722036, 0.000000000000000000, 0.4794255386042041156 ) ) ;
#12792 = CARTESIAN_POINT ( 'NONE',  ( 6.153525452890544756, -92.86910576385621141, 28.82527858285896016 ) ) ;
#12793 = CARTESIAN_POINT ( 'NONE',  ( 20.58776654729999933, -18.50000000000000000, 8.497741595429999961 ) ) ;
#12794 = CARTESIAN_POINT ( 'NONE',  ( 0.1199839491673418412, -92.96960399592218494, -30.49976399678630301 ) ) ;
#12795 = CARTESIAN_POINT ( 'NONE',  ( 36.70830950850000107, -75.00000000000000000, -14.75000000000000000 ) ) ;
#12796 = ORIENTED_EDGE ( 'NONE', *, *, #16712, .F. ) ;
#12797 = ADVANCED_FACE ( 'NONE', ( #24001 ), #17452, .F. ) ;
#12798 = DIRECTION ( 'NONE',  ( 0.000000000000000000, -1.000000000000000000, 0.000000000000000000 ) ) ;
#12799 = DIRECTION ( 'NONE',  ( 1.000000000000000000, 0.000000000000000000, 0.000000000000000000 ) ) ;
#12800 = EDGE_LOOP ( 'NONE', ( #19278, #27959, #11361, #18929 ) ) ;
#12801 = ADVANCED_FACE ( 'NONE', ( #13349 ), #8709, .T. ) ;
#12802 = CARTESIAN_POINT ( 'NONE',  ( 21.02097499579999962, -36.24640870310000196, -8.676716518870000172 ) ) ;
#12803 = CARTESIAN_POINT ( 'NONE',  ( 6.850353625200000351, -36.56979901409999911, -21.56931447779999900 ) ) ;
#12804 = VERTEX_POINT ( 'NONE', #13054 ) ;
#12805 = EDGE_CURVE ( 'NONE', #4037, #19516, #3897, .T. ) ;
#12806 = CARTESIAN_POINT ( 'NONE',  ( -12.99806807920000118, -101.2995922080000071, -9.195720578049998650 ) ) ;
#12807 = CARTESIAN_POINT ( 'NONE',  ( -13.16778098350000015, -93.19477590270000178, -23.58326777899999982 ) ) ;
#12808 = CARTESIAN_POINT ( 'NONE',  ( -7.983017350639999954, -99.94751438429999268, 15.18573513309999790 ) ) ;
#12809 = CARTESIAN_POINT ( 'NONE',  ( -3.055530165179999980, -94.70873790529999781, 23.49572270359999848 ) ) ;
#12810 = CARTESIAN_POINT ( 'NONE',  ( 19.43643804750000115, -34.66800313659999944, -8.988996126470000902 ) ) ;
#12811 = CARTESIAN_POINT ( 'NONE',  ( -10.77422065139999852, -19.15825174789999963, -19.39513388339999622 ) ) ;
#12812 = CARTESIAN_POINT ( 'NONE',  ( -26.69293917519999937, -33.49689110869999809, -48.86109741659999628 ) ) ;
#12813 = ORIENTED_EDGE ( 'NONE', *, *, #19207, .T. ) ;
#12814 = CARTESIAN_POINT ( 'NONE',  ( 13.63841234616398879, -100.4010812937911510, -10.11563007918305601 ) ) ;
#12815 = CARTESIAN_POINT ( 'NONE',  ( 25.32712246539999867, -57.40875703270000230, 1.379782582989999895 ) ) ;
#12816 = CARTESIAN_POINT ( 'NONE',  ( 24.30013770089999880, -66.02175891730000501, 10.80690825860000004 ) ) ;
#12817 = DIRECTION ( 'NONE',  ( 1.000000000000000000, 0.000000000000000000, 1.836909530729999990E-16 ) ) ;
#12818 = ORIENTED_EDGE ( 'NONE', *, *, #12658, .F. ) ;
#12819 = DIRECTION ( 'NONE',  ( 0.000000000000000000, 1.000000000000000000, 0.000000000000000000 ) ) ;
#12820 = CYLINDRICAL_SURFACE ( 'NONE', #8529, 0.5000000000000012212 ) ;
#12821 = CARTESIAN_POINT ( 'NONE',  ( -41.74235873792772367, -63.06523941402236488, -2.751386478892827281 ) ) ;
#12822 = DIRECTION ( 'NONE',  ( 0.000000000000000000, -1.000000000000000000, 0.000000000000000000 ) ) ;
#12823 = VERTEX_POINT ( 'NONE', #21818 ) ;
#12824 = CARTESIAN_POINT ( 'NONE',  ( 28.63360536809999957, -72.82938840390001189, 1.697633657649999961 ) ) ;
#12825 = ADVANCED_FACE ( 'NONE', ( #28648 ), #18504, .T. ) ;
#12826 = CARTESIAN_POINT ( 'NONE',  ( 9.038647564319999717, -35.72724395809999720, -19.55068592700000352 ) ) ;
#12827 = FACE_OUTER_BOUND ( 'NONE', #13178, .T. ) ;
#12828 = FACE_OUTER_BOUND ( 'NONE', #11726, .T. ) ;
#12829 = CARTESIAN_POINT ( 'NONE',  ( 22.43070387670000088, -60.15167146970000545, 10.24377596799999957 ) ) ;
#12830 = CARTESIAN_POINT ( 'NONE',  ( -36.83844719860000083, -65.17124718639999514, 0.1954025812279999996 ) ) ;
#12831 = ORIENTED_EDGE ( 'NONE', *, *, #24680, .F. ) ;
#12832 = CARTESIAN_POINT ( 'NONE',  ( 6.775066376809999902, -101.3878691800000098, 14.60824414760000067 ) ) ;
#12833 = CARTESIAN_POINT ( 'NONE',  ( 14.96872597019999951, -101.0403179300000005, 3.906879788429999500 ) ) ;
#12834 = EDGE_CURVE ( 'NONE', #22453, #842, #12553, .T. ) ;
#12835 = CARTESIAN_POINT ( 'NONE',  ( -32.70331798974049775, -74.50000000070001249, -22.03951504806313011 ) ) ;
#12836 = CARTESIAN_POINT ( 'NONE',  ( 24.22382764319999993, -64.24504439390000243, 10.76339940740000145 ) ) ;
#12837 = DIRECTION ( 'NONE',  ( 0.2414462220490755373, 0.000000000000000000, 0.9704142011833032377 ) ) ;
#12838 = ORIENTED_EDGE ( 'NONE', *, *, #23477, .F. ) ;
#12839 = CARTESIAN_POINT ( 'NONE',  ( 8.467196410959999753, -93.92589062430000979, -23.69480735049999964 ) ) ;
#12840 = B_SPLINE_SURFACE_WITH_KNOTS ( 'NONE', 5, 5, ( 
 ( #2475, #22870, #4797, #6988, #26946, #9295 ),
 ( #22429, #15700, #20684, #20087, #25046, #15852 ),
 ( #20376, #6692, #151, #5079, #15554, #13369 ),
 ( #22722, #2760, #11773, #22579, #305, #24458 ),
 ( #13816, #22273, #17911, #26804, #27092, #11471 ),
 ( #8849, #17762, #9144, #26648, #6836, #20529 ),
 ( #4494, #18049, #11618, #445, #24606, #24761 ),
 ( #2911, #13674, #2622, #18197, #7133, #598 ),
 ( #16001, #24905, #4935, #9442, #18350, #27237 ) ),
 .UNSPECIFIED., .F., .F., .F.,
 ( 6, 3, 6 ),
 ( 6, 6 ),
 ( 0.2311830627119999815, 0.9730373362299999940, 1.893943578530000060 ),
 ( 0.000000000000000000, 0.5000000000000000000 ),
 .UNSPECIFIED. ) ;
#12841 = FACE_OUTER_BOUND ( 'NONE', #5444, .T. ) ;
#12842 = DIRECTION ( 'NONE',  ( 1.000000000000000000, 0.000000000000000000, 0.000000000000000000 ) ) ;
#12843 = EDGE_LOOP ( 'NONE', ( #16546, #21439, #23035, #28682 ) ) ;
#12844 = CARTESIAN_POINT ( 'NONE',  ( -12.83467265744653929, -100.4872618010412992, -11.01232127950116890 ) ) ;
#12845 = ORIENTED_EDGE ( 'NONE', *, *, #25573, .F. ) ;
#12846 = CARTESIAN_POINT ( 'NONE',  ( 26.24918299980000214, -92.87437365140000622, -7.909057152789999989 ) ) ;
#12847 = ORIENTED_EDGE ( 'NONE', *, *, #7974, .F. ) ;
#12848 = CARTESIAN_POINT ( 'NONE',  ( 12.82422237299999956, -94.98812477769999418, -19.93894812050000098 ) ) ;
#12849 = CARTESIAN_POINT ( 'NONE',  ( 21.82773932530000138, -18.50000000000000000, 1.697762045069999948 ) ) ;
#12850 = CARTESIAN_POINT ( 'NONE',  ( -24.63993737860000266, -72.00000000000000000, 17.98210258840000009 ) ) ;
#12851 = CARTESIAN_POINT ( 'NONE',  ( -19.78043542534729227, -92.52498922770500656, -23.21615846764749236 ) ) ;
#12852 = ORIENTED_EDGE ( 'NONE', *, *, #7160, .F. ) ;
#12853 = CARTESIAN_POINT ( 'NONE',  ( -6.439729480049999566, -101.2530993010000060, 13.76171823350000167 ) ) ;
#12854 = CARTESIAN_POINT ( 'NONE',  ( 4.500000000000000000, -15.00000000000000000, -31.00000000000000000 ) ) ;
#12855 = EDGE_CURVE ( 'NONE', #24745, #23918, #6040, .T. ) ;
#12856 = CARTESIAN_POINT ( 'NONE',  ( 13.75485398520459057, -100.1406256088168760, -10.30979386037251189 ) ) ;
#12857 = CARTESIAN_POINT ( 'NONE',  ( -18.51066704717978695, -19.46987374639787305, 12.90209632547328944 ) ) ;
#12858 = CARTESIAN_POINT ( 'NONE',  ( 7.355131038309999703, -34.88462684899999999, -21.34291130700000139 ) ) ;
#12859 = LINE ( 'NONE', #10526, #28105 ) ;
#12860 = EDGE_LOOP ( 'NONE', ( #21519, #23167, #5608, #20995 ) ) ;
#12861 = CARTESIAN_POINT ( 'NONE',  ( 7.383548971359999769, -18.50000000000000000, -19.69582298410000121 ) ) ;
#12862 = CARTESIAN_POINT ( 'NONE',  ( 22.92823879609999693, -37.07368284070000186, -9.571688886919998751 ) ) ;
#12863 = EDGE_CURVE ( 'NONE', #27211, #5075, #7963, .T. ) ;
#12864 = AXIS2_PLACEMENT_3D ( 'NONE', #18044, #22717, #11168 ) ;
#12865 = CARTESIAN_POINT ( 'NONE',  ( 7.151043167926666833, -36.56947960410957421, -21.49478374055488317 ) ) ;
#12866 = CARTESIAN_POINT ( 'NONE',  ( -27.68682485439999752, -20.89999999999999858, -50.68039294919999804 ) ) ;
#12867 = CARTESIAN_POINT ( 'NONE',  ( -20.51033946140000097, -54.98594849529999351, 14.82152834640000094 ) ) ;
#12868 = DIRECTION ( 'NONE',  ( 0.9952295494196654602, 0.000000000000000000, -0.09756097560976770278 ) ) ;
#12869 = DIRECTION ( 'NONE',  ( 0.4794255386042040601, 0.000000000000000000, 0.8775825618903722036 ) ) ;
#12870 = EDGE_LOOP ( 'NONE', ( #19709, #951, #16894, #354 ) ) ;
#12871 = CARTESIAN_POINT ( 'NONE',  ( -15.02595431881585242, -98.99956644457965638, -10.95841658774190108 ) ) ;
#12872 = AXIS2_PLACEMENT_3D ( 'NONE', #25554, #3415, #21737 ) ;
#12873 = DIRECTION ( 'NONE',  ( 0.000000000000000000, -1.000000000000000000, 0.000000000000000000 ) ) ;
#12874 = ORIENTED_EDGE ( 'NONE', *, *, #6069, .F. ) ;
#12875 = DIRECTION ( 'NONE',  ( 0.4794255386042036160, 0.000000000000000000, 0.8775825618903723147 ) ) ;
#12876 = EDGE_LOOP ( 'NONE', ( #6389, #11646, #15953, #18969 ) ) ;
#12877 = LINE ( 'NONE', #6203, #19734 ) ;
#12878 = CARTESIAN_POINT ( 'NONE',  ( 20.70007164369999941, -19.44981017030000103, 9.428305666440000010 ) ) ;
#12879 = CARTESIAN_POINT ( 'NONE',  ( -22.21882404873914396, -74.32470999146529778, -32.79282312874325100 ) ) ;
#12880 = AXIS2_PLACEMENT_3D ( 'NONE', #14925, #12183, #1562 ) ;
#12881 = CARTESIAN_POINT ( 'NONE',  ( 21.64091288609999708, -18.86472494550000079, 9.360502753589999614 ) ) ;
#12882 = CARTESIAN_POINT ( 'NONE',  ( -32.70912902188079130, -74.24831373276512636, -22.19863839555747020 ) ) ;
#12883 = DIRECTION ( 'NONE',  ( 0.000000000000000000, -1.000000000000000000, 0.000000000000000000 ) ) ;
#12884 = ORIENTED_EDGE ( 'NONE', *, *, #21421, .T. ) ;
#12885 = DIRECTION ( 'NONE',  ( 0.9704142011833032377, 0.000000000000000000, 0.2414462220490753985 ) ) ;
#12886 = CARTESIAN_POINT ( 'NONE',  ( -11.89877799829999994, -101.0147083550000104, -10.00853575740000068 ) ) ;
#12887 = EDGE_CURVE ( 'NONE', #18987, #11754, #27372, .T. ) ;
#12888 = CARTESIAN_POINT ( 'NONE',  ( -7.208022861691824268, -73.58162913641194791, 39.21655428041565727 ) ) ;
#12889 = CARTESIAN_POINT ( 'NONE',  ( -7.860694240047618742, -100.5550990450661573, 14.91249917024564198 ) ) ;
#12890 = ORIENTED_EDGE ( 'NONE', *, *, #18902, .T. ) ;
#12891 = EDGE_CURVE ( 'NONE', #9393, #14188, #16854, .T. ) ;
#12892 = DIRECTION ( 'NONE',  ( -1.000000000000000000, 0.000000000000000000, 6.217248937900000596E-16 ) ) ;
#12893 = CONICAL_SURFACE ( 'NONE', #2716, 57.74999999999999289, 1.224257462359999549 ) ;
#12894 = CARTESIAN_POINT ( 'NONE',  ( -22.47178550313523360, -79.93075540391261313, -32.73115669477952849 ) ) ;
#12895 = ORIENTED_EDGE ( 'NONE', *, *, #10688, .F. ) ;
#12896 = EDGE_CURVE ( 'NONE', #17152, #2628, #11525, .T. ) ;
#12897 = EDGE_CURVE ( 'NONE', #19426, #27931, #7365, .T. ) ;
#12898 = B_SPLINE_SURFACE_WITH_KNOTS ( 'NONE', 5, 5, ( 
 ( #12171, #7394, #9983, #5620, #9564, #16692 ),
 ( #27207, #27778, #9698, #7246, #712, #11888 ),
 ( #12311, #25454, #20941, #16411, #25318, #7693 ),
 ( #5201, #14084, #18463, #27349, #18612, #14236 ),
 ( #23404, #23264, #3306, #3170, #1000, #5047 ),
 ( #16258, #14373, #25168, #3036, #13936, #854 ) ),
 .UNSPECIFIED., .F., .F., .F.,
 ( 6, 6 ),
 ( 6, 6 ),
 ( 12.34870487170000075, 33.81329059570000339 ),
 ( 0.000000000000000000, 2.000000000000000000 ),
 .UNSPECIFIED. ) ;
#12899 = CARTESIAN_POINT ( 'NONE',  ( 19.55285847160000046, -35.83289739509999805, -9.107180759300000261 ) ) ;
#12900 = CARTESIAN_POINT ( 'NONE',  ( 12.02686724500000004, -92.54157628459999785, 27.32173438410000088 ) ) ;
#12901 = ORIENTED_EDGE ( 'NONE', *, *, #22380, .F. ) ;
#12902 = CIRCLE ( 'NONE', #11025, 0.5000000000000004441 ) ;
#12903 = CARTESIAN_POINT ( 'NONE',  ( -15.11912402641494424, -93.86130746169172312, -21.61442877420574149 ) ) ;
#12904 = AXIS2_PLACEMENT_3D ( 'NONE', #4354, #15108, #26065 ) ;
#12905 = ORIENTED_EDGE ( 'NONE', *, *, #10520, .F. ) ;
#12906 = CARTESIAN_POINT ( 'NONE',  ( 20.42111665379999863, -55.05574748869999979, 11.17031783180000026 ) ) ;
#12907 = CARTESIAN_POINT ( 'NONE',  ( 45.99664575370000108, -73.93831497249999529, -4.396813293179999249 ) ) ;
#12908 = ORIENTED_EDGE ( 'NONE', *, *, #4859, .F. ) ;
#12909 = DIRECTION ( 'NONE',  ( 1.000000000000000000, 0.000000000000000000, 6.123031769109999188E-17 ) ) ;
#12910 = CARTESIAN_POINT ( 'NONE',  ( 47.19280574540000117, -74.66665734379999719, -1.149945984370000174 ) ) ;
#12911 = ORIENTED_EDGE ( 'NONE', *, *, #2888, .T. ) ;
#12912 = AXIS2_PLACEMENT_3D ( 'NONE', #26513, #9018, #15416 ) ;
#12913 = CARTESIAN_POINT ( 'NONE',  ( -12.07243358760000085, -45.73899999920000425, -24.77970463289999969 ) ) ;
#12914 = CARTESIAN_POINT ( 'NONE',  ( -18.88944331899999796, -93.00000000000000000, -23.13319212550000259 ) ) ;
#12915 = CARTESIAN_POINT ( 'NONE',  ( -21.97175844099999864, -92.62399497440000573, -19.94807775750000189 ) ) ;
#12916 = CARTESIAN_POINT ( 'NONE',  ( -39.50000000000000000, -63.30468293320000583, 2.309401076760000393 ) ) ;
#12917 = VERTEX_POINT ( 'NONE', #3587 ) ;
#12918 = CARTESIAN_POINT ( 'NONE',  ( -15.09406086359999932, -98.83667233820000320, -10.95640931279999997 ) ) ;
#12919 = CARTESIAN_POINT ( 'NONE',  ( 12.62715338020000111, -101.2063419769999939, -9.804727914620000817 ) ) ;
#12920 = DIRECTION ( 'NONE',  ( 1.000000000000000000, 0.000000000000000000, 0.000000000000000000 ) ) ;
#12921 = CARTESIAN_POINT ( 'NONE',  ( -2.363861431270000146, -52.59522851940000265, -24.20187825489999867 ) ) ;
#12922 = CARTESIAN_POINT ( 'NONE',  ( 29.85855671192240379, -92.56772982766284485, 6.222565568561500449 ) ) ;
#12923 = CARTESIAN_POINT ( 'NONE',  ( -19.68803165839999991, -18.87168151170000030, 14.53288016459999987 ) ) ;
#12924 = ORIENTED_EDGE ( 'NONE', *, *, #16848, .F. ) ;
#12925 = ADVANCED_FACE ( 'NONE', ( #14657 ), #20368, .F. ) ;
#12926 = AXIS2_PLACEMENT_3D ( 'NONE', #9731, #18643, #7982 ) ;
#12927 = FACE_OUTER_BOUND ( 'NONE', #25349, .T. ) ;
#12928 = VECTOR ( 'NONE', #5431, 1000.000000000000000 ) ;
#12929 = CARTESIAN_POINT ( 'NONE',  ( 12.04737265770000043, -101.6484611540000031, -10.52904611289999970 ) ) ;
#12930 = CYLINDRICAL_SURFACE ( 'NONE', #3608, 3.749999999999996447 ) ;
#12931 = CARTESIAN_POINT ( 'NONE',  ( -38.25000000000000000, -65.63577453799999262, 1.587713240270000048 ) ) ;
#12932 = DIRECTION ( 'NONE',  ( 1.000000000000000000, 0.000000000000000000, 0.000000000000000000 ) ) ;
#12933 = ADVANCED_FACE ( 'NONE', ( #25463 ), #1012, .T. ) ;
#12934 = DIRECTION ( 'NONE',  ( 0.000000000000000000, 0.000000000000000000, 1.000000000000000000 ) ) ;
#12935 = DIRECTION ( 'NONE',  ( 0.4794255386042041156, 0.000000000000000000, 0.8775825618903722036 ) ) ;
#12936 = DIRECTION ( 'NONE',  ( 1.000000000000000000, 0.000000000000000000, 0.000000000000000000 ) ) ;
#12937 = CARTESIAN_POINT ( 'NONE',  ( -11.90992159600000200, -57.47815920179999694, -20.09952900869999937 ) ) ;
#12938 = ORIENTED_EDGE ( 'NONE', *, *, #28312, .T. ) ;
#12939 = FACE_OUTER_BOUND ( 'NONE', #13072, .T. ) ;
#12940 = CARTESIAN_POINT ( 'NONE',  ( -3.355978770230000130, -90.50000000000000000, -6.143077933229999843 ) ) ;
#12942 = ORIENTED_EDGE ( 'NONE', *, *, #13339, .T. ) ;
#12941 = CIRCLE ( 'NONE', #17661, 7.250000000000000000 ) ;
#12943 = CARTESIAN_POINT ( 'NONE',  ( 19.87955124240000160, -35.87174558430000104, -9.133536657829999683 ) ) ;
#12944 = CARTESIAN_POINT ( 'NONE',  ( 9.476764215410000247, -82.25000000000000000, -38.08875739639999836 ) ) ;
#12945 = VERTEX_POINT ( 'NONE', #14517 ) ;
#12946 = CARTESIAN_POINT ( 'NONE',  ( -12.61650973899999961, -101.1516803200000112, -8.702315162139999671 ) ) ;
#12947 = AXIS2_PLACEMENT_3D ( 'NONE', #16976, #10387, #8086 ) ;
#12948 = VECTOR ( 'NONE', #14773, 1000.000000000000000 ) ;
#12949 = CARTESIAN_POINT ( 'NONE',  ( -3.369214011477492665, -68.11464510236007186, -27.57567578509392803 ) ) ;
#12950 = CARTESIAN_POINT ( 'NONE',  ( -0.5853762890571154731, -19.20927481204733311, -22.01698796243409717 ) ) ;
#12951 = CARTESIAN_POINT ( 'NONE',  ( 9.024081099289999131, -19.49999992740000110, -18.94592230980000380 ) ) ;
#12952 = LINE ( 'NONE', #27769, #12200 ) ;
#12953 = DIRECTION ( 'NONE',  ( 0.09756097560976997873, 0.000000000000000000, 0.9952295494196653491 ) ) ;
#12954 = CARTESIAN_POINT ( 'NONE',  ( -10.06158909070000007, -18.61865660339999806, -19.91781936479999970 ) ) ;
#12955 = LINE ( 'NONE', #8731, #20913 ) ;
#12956 = ORIENTED_EDGE ( 'NONE', *, *, #15304, .T. ) ;
#12957 = CARTESIAN_POINT ( 'NONE',  ( 13.48463565429420896, -100.6644468680852924, -9.970219641038934100 ) ) ;
#12958 = CARTESIAN_POINT ( 'NONE',  ( 22.82317425849999992, -42.27249569770000193, -0.5642684588070000506 ) ) ;
#12959 = CARTESIAN_POINT ( 'NONE',  ( 25.04292896270000313, -70.80052042889998631, 11.98325363630000062 ) ) ;
#12960 = CARTESIAN_POINT ( 'NONE',  ( -16.79027416539999962, -100.2529091920000042, 3.234199557169999739 ) ) ;
#12961 = ORIENTED_EDGE ( 'NONE', *, *, #19207, .F. ) ;
#12962 = EDGE_CURVE ( 'NONE', #13629, #9669, #8260, .T. ) ;
#12963 = CARTESIAN_POINT ( 'NONE',  ( -2.453167969115414238, -64.58097188162675195, -25.72104633702097942 ) ) ;
#12964 = CARTESIAN_POINT ( 'NONE',  ( -17.60151059589999889, -93.41955571290000648, 19.34924659089999821 ) ) ;
#12965 = CARTESIAN_POINT ( 'NONE',  ( 25.14694229440000228, -65.07443093669999712, -0.3759436444569999591 ) ) ;
#12966 = EDGE_LOOP ( 'NONE', ( #17929, #25248, #28702, #17585 ) ) ;
#12967 = EDGE_CURVE ( 'NONE', #15667, #27517, #16187, .T. ) ;
#12968 = CARTESIAN_POINT ( 'NONE',  ( 36.82697890865670587, -80.36910032511354984, -13.57704402516810305 ) ) ;
#12969 = B_SPLINE_CURVE_WITH_KNOTS ( 'NONE', 3,
 ( #1516, #25172, #10360, #7249, #569, #25703 ),
 .UNSPECIFIED., .F., .F.,
 ( 4, 2, 4 ),
 ( 0.000000000000000000, 0.5000000000000000000, 1.000000000000000000 ),
 .UNSPECIFIED. ) ;
#12970 = AXIS2_PLACEMENT_3D ( 'NONE', #9335, #11661, #24945 ) ;
#12971 = CARTESIAN_POINT ( 'NONE',  ( 0.2107703687019999994, -101.2927714249999980, -16.05360085099999878 ) ) ;
#12972 = CARTESIAN_POINT ( 'NONE',  ( 7.733063023050000595, -63.62941396979999809, -23.24181039339999799 ) ) ;
#12973 = CARTESIAN_POINT ( 'NONE',  ( 15.28252213929999925, -101.1292389529999980, 2.628739817060000039 ) ) ;
#12974 = EDGE_CURVE ( 'NONE', #12631, #27292, #1156, .T. ) ;
#12975 = CARTESIAN_POINT ( 'NONE',  ( 21.83262230589999930, -60.24417646120000569, 10.33011226949999894 ) ) ;
#12976 = CARTESIAN_POINT ( 'NONE',  ( 24.08167113289999861, -63.05444450430000813, -9.753780024779999280 ) ) ;
#12977 = ORIENTED_EDGE ( 'NONE', *, *, #24434, .T. ) ;
#12978 = AXIS2_PLACEMENT_3D ( 'NONE', #3699, #12558, #14350 ) ;
#12979 = CARTESIAN_POINT ( 'NONE',  ( 6.601639229639999940, -100.7430069139999915, 15.11370351929999956 ) ) ;
#12980 = CARTESIAN_POINT ( 'NONE',  ( 14.80905440220000102, -101.2358105800000061, 3.500992360309999718 ) ) ;
#12981 = CARTESIAN_POINT ( 'NONE',  ( -5.892551212131841076, -97.41291607174348144, 19.73490353248802265 ) ) ;
#12982 = EDGE_LOOP ( 'NONE', ( #24520, #17142, #17236, #23583 ) ) ;
#12983 = CARTESIAN_POINT ( 'NONE',  ( -13.30284256589999892, -92.50000025620001054, 26.72171909750000296 ) ) ;
#12984 = CARTESIAN_POINT ( 'NONE',  ( 5.191020918613762802, -92.62800705126865353, -30.05509293616334787 ) ) ;
#12985 = B_SPLINE_CURVE_WITH_KNOTS ( 'NONE', 3,
 ( #3833, #6151, #26272, #15303, #4110, #3695, #8069, #3974, #16959, #26123, #12981, #10784, #8201, #28586, #26409, #17088, #12696 ),
 .UNSPECIFIED., .F., .F.,
 ( 4, 2, 2, 1, 1, 1, 1, 1, 2, 2, 4 ),
 ( 0.000000000000000000, 0.2500000000001315059, 0.3750000000001976752, 0.4375000000002307043, 0.4687500000002471912, 0.4843750000002554623, 0.4921875000002595701, 0.4960937500002607914, 0.4980468750002605693, 0.5000000000002603473, 1.000000000000000000 ),
 .UNSPECIFIED. ) ;
#12986 = CARTESIAN_POINT ( 'NONE',  ( -41.91080735079999897, -65.74290444429999525, -1.043878813350000101 ) ) ;
#12987 = ORIENTED_EDGE ( 'NONE', *, *, #23023, .T. ) ;
#12988 = CARTESIAN_POINT ( 'NONE',  ( 6.586633760479999822, -93.48569568790000517, -26.38833621560000253 ) ) ;
#12989 = ADVANCED_FACE ( 'NONE', ( #3455 ), #16408, .T. ) ;
#12990 = DIRECTION ( 'NONE',  ( 0.000000000000000000, 1.000000000000000000, 0.000000000000000000 ) ) ;
#12991 = DIRECTION ( 'NONE',  ( 1.000000000000000000, 0.000000000000000000, 0.000000000000000000 ) ) ;
#12992 = ORIENTED_EDGE ( 'NONE', *, *, #7024, .T. ) ;
#12993 = CARTESIAN_POINT ( 'NONE',  ( 3.768036230260000150E-15, -69.00000000000000000, 40.00000000000000000 ) ) ;
#12994 = CARTESIAN_POINT ( 'NONE',  ( -12.95358181834116351, -100.3266728694473073, -11.07102962069259000 ) ) ;
#12995 = ORIENTED_EDGE ( 'NONE', *, *, #25510, .F. ) ;
#12996 = CARTESIAN_POINT ( 'NONE',  ( 25.26718046270000073, -45.73899999920000425, 6.129403842640000377 ) ) ;
#12997 = CARTESIAN_POINT ( 'NONE',  ( 27.07127711109999879, -92.49999846069999876, -10.05443248829999980 ) ) ;
#12998 = ORIENTED_EDGE ( 'NONE', *, *, #17670, .F. ) ;
#12999 = AXIS2_PLACEMENT_3D ( 'NONE', #20036, #6083, #18002 ) ;
#13000 = TOROIDAL_SURFACE ( 'NONE', #23710, 43.34897771020000334, 20.00000000000000000 ) ;
#13001 = FACE_OUTER_BOUND ( 'NONE', #25290, .T. ) ;
#13002 = CARTESIAN_POINT ( 'NONE',  ( 21.88953683090000268, -18.85523522049999912, -0.4607248773119999585 ) ) ;
#13003 = CARTESIAN_POINT ( 'NONE',  ( -38.65106240728522380, -73.99999920929936081, -7.498734568567304137 ) ) ;
#13004 = CARTESIAN_POINT ( 'NONE',  ( 23.52622212079999997, -57.40875702419999982, -9.564509902230000193 ) ) ;
#13005 = VERTEX_POINT ( 'NONE', #19594 ) ;
#13006 = CARTESIAN_POINT ( 'NONE',  ( -14.73065703810000038, -101.1848546039999945, 4.068069544640000146 ) ) ;
#13007 = CARTESIAN_POINT ( 'NONE',  ( 16.31233561804996057, -94.64857743460261474, 17.22706169121702047 ) ) ;
#13008 = EDGE_CURVE ( 'NONE', #1224, #418, #26416, .T. ) ;
#13009 = CARTESIAN_POINT ( 'NONE',  ( 26.51307495810083381, -92.55389105864081500, 13.35502057535796894 ) ) ;
#13010 = CYLINDRICAL_SURFACE ( 'NONE', #4055, 5.000000000000001776 ) ;
#13011 = CARTESIAN_POINT ( 'NONE',  ( 0.000000000000000000, -37.57799544290000426, 0.000000000000000000 ) ) ;
#13012 = CARTESIAN_POINT ( 'NONE',  ( 7.548681495209999426, -35.51902686380000063, -21.37164025960000302 ) ) ;
#13013 = CARTESIAN_POINT ( 'NONE',  ( 19.35265720810000190, -32.04884292379999522, -8.993109114790000191 ) ) ;
#13014 = VERTEX_POINT ( 'NONE', #17854 ) ;
#13015 = ADVANCED_FACE ( 'NONE', ( #13173 ), #13864, .T. ) ;
#13016 = CARTESIAN_POINT ( 'NONE',  ( 8.201027188560001235, -18.50000000000000000, -19.45829122079999962 ) ) ;
#13017 = CIRCLE ( 'NONE', #22840, 3.750000000000000000 ) ;
#13018 = AXIS2_PLACEMENT_3D ( 'NONE', #28139, #17059, #25953 ) ;
#13019 = VERTEX_POINT ( 'NONE', #15197 ) ;
#13020 = CARTESIAN_POINT ( 'NONE',  ( -1.970171503600000040, -60.24417646110000391, -24.07266168299999975 ) ) ;
#13021 = CARTESIAN_POINT ( 'NONE',  ( -25.12376022900000194, -94.06807348059999185, -3.039477672979999934 ) ) ;
#13022 = CARTESIAN_POINT ( 'NONE',  ( -20.30439858460000124, -57.41946977150000464, 14.68516942459999974 ) ) ;
#13023 = DIRECTION ( 'NONE',  ( 0.000000000000000000, 1.000000000000000000, 0.000000000000000000 ) ) ;
#13024 = EDGE_CURVE ( 'NONE', #5884, #19001, #1313, .T. ) ;
#13025 = ORIENTED_EDGE ( 'NONE', *, *, #4275, .F. ) ;
#13026 = CARTESIAN_POINT ( 'NONE',  ( 21.21808932789999957, -34.59820509829999935, -7.670972970100000232 ) ) ;
#13027 = CARTESIAN_POINT ( 'NONE',  ( 7.253641904899999382, -74.31847293630001161, -40.32207487370000365 ) ) ;
#13028 = ORIENTED_EDGE ( 'NONE', *, *, #5573, .F. ) ;
#13029 = FACE_OUTER_BOUND ( 'NONE', #13792, .T. ) ;
#13030 = ORIENTED_EDGE ( 'NONE', *, *, #16045, .T. ) ;
#13031 = CARTESIAN_POINT ( 'NONE',  ( -14.19188836390000041, -80.00000061209999558, 37.13021406550000592 ) ) ;
#13032 = B_SPLINE_CURVE_WITH_KNOTS ( 'NONE', 3,
 ( #2176, #4496, #22431, #19929, #3, #26805, #13370, #4202, #19642, #22274, #2322, #11174, #17471, #9004, #20235, #306, #9145 ),
 .UNSPECIFIED., .F., .F.,
 ( 4, 2, 2, 1, 1, 1, 1, 1, 2, 2, 4 ),
 ( 0.000000000000000000, 0.2500000000000727751, 0.3750000000001091349, 0.4375000000001275646, 0.4687500000001377787, 0.4843750000001418865, 0.4921875000001446621, 0.4960937500001461054, 0.4980468750001466050, 0.5000000000001471046, 1.000000000000000000 ),
 .UNSPECIFIED. ) ;
#13033 = CARTESIAN_POINT ( 'NONE',  ( -9.483174519389997670, -18.50000000000000000, -21.05226109790000066 ) ) ;
#13034 = EDGE_CURVE ( 'NONE', #19989, #24375, #25035, .T. ) ;
#13035 = AXIS2_PLACEMENT_3D ( 'NONE', #6317, #28316, #21913 ) ;
#13036 = CARTESIAN_POINT ( 'NONE',  ( 32.39999999999999858, -86.00000000000000000, 3.967724586379999025E-15 ) ) ;
#13037 = CIRCLE ( 'NONE', #6553, 0.3500000000000003664 ) ;
#13038 = CIRCLE ( 'NONE', #16796, 10.00000000000000000 ) ;
#13039 = CARTESIAN_POINT ( 'NONE',  ( 22.63564271879999978, -18.50000000000000000, 8.833840388520000531 ) ) ;
#13040 = CARTESIAN_POINT ( 'NONE',  ( 19.97576656849999921, -74.00000000000000000, -19.97576656849999921 ) ) ;
#13041 = CARTESIAN_POINT ( 'NONE',  ( -13.46646228700000059, -101.3150700380000018, -9.098096927170001180 ) ) ;
#13042 = ORIENTED_EDGE ( 'NONE', *, *, #15583, .F. ) ;
#13043 = B_SPLINE_CURVE_WITH_KNOTS ( 'NONE', 3,
 ( #28158, #27747, #23641, #10491, #14472, #21317, #18994, #19406, #28287, #19132, #8318, #7785, #27874, #16805, #26112, #14334, #12133, #21050, #25840 ),
 .UNSPECIFIED., .F., .F.,
 ( 4, 2, 2, 2, 1, 1, 1, 2, 2, 2, 4 ),
 ( 0.000000000000000000, 0.2499999999999667488, 0.3749999999999501510, 0.4374999999999416578, 0.4687499999999342193, 0.4843749999999327760, 0.4921874999999295563, 0.4960937499999287792, 0.4999999999999280575, 0.7499999999999641398, 1.000000000000000000 ),
 .UNSPECIFIED. ) ;
#13044 = CARTESIAN_POINT ( 'NONE',  ( 0.000000000000000000, -84.75000000000000000, 0.000000000000000000 ) ) ;
#13045 = CARTESIAN_POINT ( 'NONE',  ( -12.28682837150000040, -101.1417990620000040, -9.866547330559999551 ) ) ;
#13046 = FILL_AREA_STYLE ('',( #24282 ) ) ;
#13047 = CARTESIAN_POINT ( 'NONE',  ( -7.647449374585493231, -101.0147714268888848, 14.61310169654407254 ) ) ;
#13048 = EDGE_LOOP ( 'NONE', ( #2946, #18081, #16889, #11906, #5704 ) ) ;
#13049 = DIRECTION ( 'NONE',  ( 1.000000000000000000, 0.000000000000000000, 0.000000000000000000 ) ) ;
#13050 = CARTESIAN_POINT ( 'NONE',  ( -32.19107628040000435, -74.02008960720000630, -22.07235371499999843 ) ) ;
#13051 = ORIENTED_EDGE ( 'NONE', *, *, #2625, .T. ) ;
#13052 = CARTESIAN_POINT ( 'NONE',  ( 24.90033419343626875, -40.03422670538211747, 1.393580993394984757 ) ) ;
#13053 = CIRCLE ( 'NONE', #11206, 9.999999999999996447 ) ;
#13054 = CARTESIAN_POINT ( 'NONE',  ( -4.500000000000000000, -15.00000000000000000, -31.00000000000000000 ) ) ;
#13055 = CIRCLE ( 'NONE', #12600, 38.75000000000000000 ) ;
#13056 = EDGE_LOOP ( 'NONE', ( #18467, #285, #23703, #18045, #27639, #23913, #14763, #7286, #28799, #10880, #9455, #23946, #7774, #4131, #4350, #13060 ) ) ;
#13057 = CIRCLE ( 'NONE', #26101, 3.749999999999996447 ) ;
#13058 = DIRECTION ( 'NONE',  ( 1.000000000000000000, 0.000000000000000000, 0.000000000000000000 ) ) ;
#13059 = CARTESIAN_POINT ( 'NONE',  ( -20.43932202180000246, -94.59276292389999696, 12.18704577789999988 ) ) ;
#13060 = ORIENTED_EDGE ( 'NONE', *, *, #20433, .T. ) ;
#13061 = CARTESIAN_POINT ( 'NONE',  ( 24.22266071560000000, -93.30149109789999784, 12.29404703189999815 ) ) ;
#13062 = CARTESIAN_POINT ( 'NONE',  ( 0.000000000000000000, -15.00000000000000000, 0.000000000000000000 ) ) ;
#13063 = VERTEX_POINT ( 'NONE', #19874 ) ;
#13064 = CARTESIAN_POINT ( 'NONE',  ( 45.84677419350000349, -80.50000000000000000, -4.286925650119999709 ) ) ;
#13065 = CARTESIAN_POINT ( 'NONE',  ( -22.22906621679999972, -79.65851410119999798, -32.83566840089999772 ) ) ;
#13066 = EDGE_CURVE ( 'NONE', #623, #9249, #28199, .T. ) ;
#13067 = ORIENTED_EDGE ( 'NONE', *, *, #24061, .F. ) ;
#13068 = CARTESIAN_POINT ( 'NONE',  ( -29.47185689770189398, -92.86910576385491822, -0.4149841894467364845 ) ) ;
#13069 = EDGE_CURVE ( 'NONE', #14954, #2162, #19892, .T. ) ;
#13070 = CARTESIAN_POINT ( 'NONE',  ( 0.000000000000000000, -57.47855601759999900, 0.000000000000000000 ) ) ;
#13071 = CARTESIAN_POINT ( 'NONE',  ( -0.7584661595949999668, -18.50000000000000000, -21.02157855700000155 ) ) ;
#13072 = EDGE_LOOP ( 'NONE', ( #5365, #10655, #15349, #19298 ) ) ;
#13073 = EDGE_CURVE ( 'NONE', #5555, #25224, #14779, .T. ) ;
#13074 = CARTESIAN_POINT ( 'NONE',  ( -41.74999999998716760, -63.32273534313992513, -1.487446372639924963 ) ) ;
#13075 = CARTESIAN_POINT ( 'NONE',  ( 12.69294339169999830, -100.9137139110000021, -9.125620792290000338 ) ) ;
#13076 = LINE ( 'NONE', #8697, #5505 ) ;
#13077 = CARTESIAN_POINT ( 'NONE',  ( -1.156066514279999957, -56.26441942339999969, -23.35759358749999848 ) ) ;
#13078 = DIRECTION ( 'NONE',  ( 0.3422283636740854340, -0.7003189540771749266, 0.6264448177271558782 ) ) ;
#13079 = CIRCLE ( 'NONE', #1943, 1.000000000000000888 ) ;
#13080 = CARTESIAN_POINT ( 'NONE',  ( 11.21116711998534576, -72.35538559737412356, -26.93475422593673230 ) ) ;
#13081 = CARTESIAN_POINT ( 'NONE',  ( -40.00000000000000000, -69.00000000000000000, 3.236300116779999679E-15 ) ) ;
#13082 = ORIENTED_EDGE ( 'NONE', *, *, #3508, .F. ) ;
#13083 = CIRCLE ( 'NONE', #28002, 10.00000000000000000 ) ;
#13084 = CARTESIAN_POINT ( 'NONE',  ( -29.91144828099999842, -92.50000000000000000, -0.6532076026720000650 ) ) ;
#13085 = CARTESIAN_POINT ( 'NONE',  ( -29.08514934200000113, -10.00000000000000000, -53.24000875469999983 ) ) ;
#13086 = CARTESIAN_POINT ( 'NONE',  ( -14.42556421679999978, -101.1889999979999999, -2.978755036369999942 ) ) ;
#13087 = CARTESIAN_POINT ( 'NONE',  ( 20.38105827579999740, -18.50000000000000000, 8.542818265839999370 ) ) ;
#13088 = CARTESIAN_POINT ( 'NONE',  ( 19.91489911684789504, -97.53591929688253970, 2.489632866012725820 ) ) ;
#13089 = B_SPLINE_SURFACE_WITH_KNOTS ( 'NONE', 5, 5, ( 
 ( #20220, #9133, #10716, #12907, #2164, #26934 ),
 ( #6369, #15096, #19631, #11000, #15236, #24297 ),
 ( #8684, #17602, #4341, #8833, #15542, #24448 ),
 ( #2307, #11157, #20075, #24748, #16274, #13953 ),
 ( #4783, #18626, #7264, #13802, #25030, #5364 ),
 ( #15837, #22707, #434, #25188, #27079, #9282 ),
 ( #22568, #9578, #18182, #18480, #9428, #7121 ),
 ( #20670, #11605, #15985, #730, #20513, #22856 ),
 ( #18334, #24891, #4924, #13662, #2899, #2608 ) ),
 .UNSPECIFIED., .F., .F., .F.,
 ( 6, 3, 6 ),
 ( 6, 6 ),
 ( 4.259926120710000319, 7.604735995929999604, 9.437975975800000583 ),
 ( 0.000000000000000000, 0.5000000000000000000 ),
 .UNSPECIFIED. ) ;
#13090 = DIRECTION ( 'NONE',  ( 0.000000000000000000, 0.000000000000000000, 1.000000000000000000 ) ) ;
#13091 = DIRECTION ( 'NONE',  ( 0.000000000000000000, 1.000000000000000000, 0.000000000000000000 ) ) ;
#13092 = ORIENTED_EDGE ( 'NONE', *, *, #13137, .T. ) ;
#13093 = CARTESIAN_POINT ( 'NONE',  ( 22.33318586679999740, -95.76596938049999608, -4.313430884220000650 ) ) ;
#13094 = ORIENTED_EDGE ( 'NONE', *, *, #15036, .T. ) ;
#13095 = CARTESIAN_POINT ( 'NONE',  ( 28.66034821447630065, -72.31232981782518721, 2.687344020524678356 ) ) ;
#13096 = CARTESIAN_POINT ( 'NONE',  ( 0.000000000000000000, -34.10310889129999623, 0.000000000000000000 ) ) ;
#13097 = ORIENTED_EDGE ( 'NONE', *, *, #7224, .T. ) ;
#13098 = CIRCLE ( 'NONE', #17786, 9.000000000000000000 ) ;
#13099 = DIRECTION ( 'NONE',  ( 1.000000000000000000, 0.000000000000000000, 0.000000000000000000 ) ) ;
#13100 = ADVANCED_FACE ( 'NONE', ( #20780 ), #4553, .T. ) ;
#13101 = CARTESIAN_POINT ( 'NONE',  ( 0.000000000000000000, -13.50000000000000000, 14.25000000000000000 ) ) ;
#13102 = CARTESIAN_POINT ( 'NONE',  ( -26.33972759919999973, -74.00000000000000000, -36.23922253580000330 ) ) ;
#13103 = ORIENTED_EDGE ( 'NONE', *, *, #14473, .F. ) ;
#13104 = CARTESIAN_POINT ( 'NONE',  ( -4.535184989290000246, -98.41760973750001540, -18.76514591000000109 ) ) ;
#13105 = CARTESIAN_POINT ( 'NONE',  ( -29.21843812340000213, -92.50000000000000000, 6.434616699369999360 ) ) ;
#13106 = CARTESIAN_POINT ( 'NONE',  ( -20.22328760799999969, -94.79579754960001026, 12.30739653150000024 ) ) ;
#13107 = CARTESIAN_POINT ( 'NONE',  ( -29.74292299291512620, -92.82709422631626239, 6.753409419028412408 ) ) ;
#13108 = CARTESIAN_POINT ( 'NONE',  ( 11.92827614917728418, -99.33527508908198911, -14.57398112561237191 ) ) ;
#13109 = ORIENTED_EDGE ( 'NONE', *, *, #22877, .T. ) ;
#13110 = EDGE_CURVE ( 'NONE', #5390, #7572, #16400, .T. ) ;
#13111 = CARTESIAN_POINT ( 'NONE',  ( -38.25000000000000000, -63.30468293320000583, 1.587713240270000048 ) ) ;
#13112 = CARTESIAN_POINT ( 'NONE',  ( 24.71478468710000342, -57.43018267659999765, 1.313252578800000014 ) ) ;
#13113 = CARTESIAN_POINT ( 'NONE',  ( -27.40038777100000189, -77.00000000000000000, -36.59277592640000165 ) ) ;
#13114 = CARTESIAN_POINT ( 'NONE',  ( 39.27497438177074685, -73.60295742109256878, 7.213678002735273154 ) ) ;
#13115 = VERTEX_POINT ( 'NONE', #24706 ) ;
#13116 = CARTESIAN_POINT ( 'NONE',  ( -38.25000000000000000, -63.24880261863425090, -1.898084215915099460 ) ) ;
#13117 = CARTESIAN_POINT ( 'NONE',  ( -18.02343650629999772, -94.04288410259999864, 18.38798360810000077 ) ) ;
#13118 = CARTESIAN_POINT ( 'NONE',  ( 41.00000000000000000, -74.00000000000000000, -10.20110288159999890 ) ) ;
#13119 = ORIENTED_EDGE ( 'NONE', *, *, #8694, .T. ) ;
#13120 = CARTESIAN_POINT ( 'NONE',  ( 28.25592597320000010, -71.94685997979999570, 1.272191253259999932 ) ) ;
#13121 = CIRCLE ( 'NONE', #10797, 0.7499999999999997780 ) ;
#13122 = CARTESIAN_POINT ( 'NONE',  ( 0.4502802160170000234, -100.9678331089999972, -16.17514339299999904 ) ) ;
#13123 = DIRECTION ( 'NONE',  ( 1.000000000000000000, 0.000000000000000000, -1.734723475976805517E-15 ) ) ;
#13124 = DIRECTION ( 'NONE',  ( 1.000000000000000000, 0.000000000000000000, 0.000000000000000000 ) ) ;
#13125 = CARTESIAN_POINT ( 'NONE',  ( 20.87785960109999905, -60.34598855900000558, 11.06351907140000002 ) ) ;
#13126 = AXIS2_PLACEMENT_3D ( 'NONE', #21825, #1321, #12775 ) ;
#13127 = ORIENTED_EDGE ( 'NONE', *, *, #17200, .F. ) ;
#13128 = CARTESIAN_POINT ( 'NONE',  ( -50.00000000000000000, -15.00000000000000000, -4.500000000000000000 ) ) ;
#13129 = VERTEX_POINT ( 'NONE', #13466 ) ;
#13130 = CARTESIAN_POINT ( 'NONE',  ( -2.619606055569999814, -19.50000000000000000, -24.29997775220000023 ) ) ;
#13131 = CARTESIAN_POINT ( 'NONE',  ( 3.787197165510000296, -93.00000000000000000, -30.26395773239999798 ) ) ;
#13132 = ADVANCED_FACE ( 'NONE', ( #9677 ), #17119, .F. ) ;
#13133 = CARTESIAN_POINT ( 'NONE',  ( -4.400377801179999437, -95.75647260670000094, 22.05748086060000190 ) ) ;
#13134 = ORIENTED_EDGE ( 'NONE', *, *, #8119, .T. ) ;
#13135 = CARTESIAN_POINT ( 'NONE',  ( 9.397448849349999023, -94.89419905519999077, -22.59845534099999753 ) ) ;
#13136 = CARTESIAN_POINT ( 'NONE',  ( -6.665307709260000379, -111.0000000000000000, -13.13558364449999871 ) ) ;
#13137 = EDGE_CURVE ( 'NONE', #4936, #7956, #3190, .T. ) ;
#13138 = CARTESIAN_POINT ( 'NONE',  ( 20.63024960799999974, -19.43020100670000261, -7.734540904970000241 ) ) ;
#13139 = CARTESIAN_POINT ( 'NONE',  ( -7.135467526410000261, -73.65707963269998970, -38.71641004229999794 ) ) ;
#13140 = CARTESIAN_POINT ( 'NONE',  ( 0.000000000000000000, -111.0000000000000000, 0.000000000000000000 ) ) ;
#13141 = ORIENTED_EDGE ( 'NONE', *, *, #26655, .F. ) ;
#13142 = CARTESIAN_POINT ( 'NONE',  ( -3.653527372796985695, -80.06168500522677789, 46.47637749218215220 ) ) ;
#13143 = EDGE_CURVE ( 'NONE', #11541, #22767, #27399, .T. ) ;
#13144 = CIRCLE ( 'NONE', #14985, 13.13304743849999845 ) ;
#13145 = CARTESIAN_POINT ( 'NONE',  ( -12.58496709408010972, -100.9229461901620937, -10.77194485367771826 ) ) ;
#13146 = ORIENTED_EDGE ( 'NONE', *, *, #12465, .T. ) ;
#13147 = FACE_OUTER_BOUND ( 'NONE', #24412, .T. ) ;
#13148 = AXIS2_PLACEMENT_3D ( 'NONE', #15136, #1769, #19254 ) ;
#13149 = DIRECTION ( 'NONE',  ( 0.09756097560976716154, 0.000000000000000000, 0.9952295494196655712 ) ) ;
#13150 = EDGE_CURVE ( 'NONE', #7636, #19075, #27481, .T. ) ;
#13151 = CARTESIAN_POINT ( 'NONE',  ( -1.241004412070000118, -101.0848057460000007, -15.36253221559999993 ) ) ;
#13152 = CARTESIAN_POINT ( 'NONE',  ( 22.98887299579999777, -18.62004679909999894, 1.721454723069999915 ) ) ;
#13153 = CARTESIAN_POINT ( 'NONE',  ( 0.000000000000000000, -84.75000000000000000, 0.000000000000000000 ) ) ;
#13154 = VERTEX_POINT ( 'NONE', #4740 ) ;
#13155 = CARTESIAN_POINT ( 'NONE',  ( -14.89765609740000052, -101.1045759049999901, 4.404014004990000508 ) ) ;
#13156 = CARTESIAN_POINT ( 'NONE',  ( -26.77683864449999973, -23.00000000000000000, -49.01467436490000296 ) ) ;
#13157 = CARTESIAN_POINT ( 'NONE',  ( 16.24020105036429484, -94.68293928641202228, 17.23415085847014083 ) ) ;
#13158 = DIRECTION ( 'NONE',  ( 0.000000000000000000, 1.000000000000000000, 0.000000000000000000 ) ) ;
#13159 = PRODUCT ( 'Housing Torx Attachment Screw', 'Housing Torx Attachment Screw', '', ( #22888 ) ) ;
#13160 = CONICAL_SURFACE ( 'NONE', #24342, 55.67692378859999280, 1.047197551199999799 ) ;
#13161 = B_SPLINE_CURVE_WITH_KNOTS ( 'NONE', 3,
 ( #4013, #19739, #17564, #26315, #3736, #12738, #19328, #15065, #23976, #24265, #28070, #12595, #21787, #25884, #26024, #12871, #6491 ),
 .UNSPECIFIED., .F., .F.,
 ( 4, 2, 2, 1, 1, 1, 1, 1, 2, 2, 4 ),
 ( 0.000000000000000000, 0.2499999999999857336, 0.3749999999999782396, 0.4374999999999752420, 0.4687499999999737987, 0.4843749999999718558, 0.4921874999999703570, 0.4960937499999696909, 0.4980468749999701905, 0.4999999999999706901, 1.000000000000000000 ),
 .UNSPECIFIED. ) ;
#13162 = CARTESIAN_POINT ( 'NONE',  ( 0.000000000000000000, -65.07443093669999712, 0.000000000000000000 ) ) ;
#13163 = FACE_OUTER_BOUND ( 'NONE', #22244, .T. ) ;
#13164 = DIRECTION ( 'NONE',  ( -0.1988145312159089739, -0.9099612708765829616, -0.3639275582888334415 ) ) ;
#13165 = DIRECTION ( 'NONE',  ( 0.000000000000000000, -1.000000000000000000, 0.000000000000000000 ) ) ;
#13166 = CARTESIAN_POINT ( 'NONE',  ( 24.95011738624632613, -93.41743724467393406, 11.71896984693396604 ) ) ;
#13167 = EDGE_LOOP ( 'NONE', ( #10009, #16315, #6906, #19191 ) ) ;
#13168 = DIRECTION ( 'NONE',  ( -0.000000000000000000, 1.000000000000000000, 0.000000000000000000 ) ) ;
#13169 = CARTESIAN_POINT ( 'NONE',  ( 22.97877291159999658, -37.99999999279999230, -9.393614097370001303 ) ) ;
#13170 = AXIS2_PLACEMENT_3D ( 'NONE', #3093, #16611, #18381 ) ;
#13171 = CARTESIAN_POINT ( 'NONE',  ( -13.13212274099999988, -63.41261178559999223, 21.16710223579999806 ) ) ;
#13172 = CARTESIAN_POINT ( 'NONE',  ( -23.85439607509999860, -94.57749572790000059, -4.067360661330000404 ) ) ;
#13173 = FACE_OUTER_BOUND ( 'NONE', #7019, .T. ) ;
#13174 = CARTESIAN_POINT ( 'NONE',  ( -19.77751067240000182, -52.59522851940014476, 14.14810317790000838 ) ) ;
#13175 = EDGE_CURVE ( 'NONE', #18448, #17829, #22526, .T. ) ;
#13176 = EDGE_CURVE ( 'NONE', #19773, #15453, #900, .T. ) ;
#13177 = CARTESIAN_POINT ( 'NONE',  ( 16.20958609349999691, -100.4071172650000108, 4.379827211240000295 ) ) ;
#13178 = EDGE_LOOP ( 'NONE', ( #14507, #1894, #14082, #14024 ) ) ;
#13179 = AXIS2_PLACEMENT_3D ( 'NONE', #18421, #18123, #15924 ) ;
#13180 = CARTESIAN_POINT ( 'NONE',  ( 21.44183145790000111, -35.25283582229999979, -7.100559644140000515 ) ) ;
#13181 = CARTESIAN_POINT ( 'NONE',  ( 11.70455088819999823, -93.00000000000000000, 8.942783294160001617 ) ) ;
#13182 = ORIENTED_EDGE ( 'NONE', *, *, #5597, .T. ) ;
#13183 = ADVANCED_FACE ( 'NONE', ( #20180 ), #18015, .F. ) ;
#13184 = FACE_OUTER_BOUND ( 'NONE', #28068, .T. ) ;
#13185 = CARTESIAN_POINT ( 'NONE',  ( 0.6601778629024529499, -99.57060688035245732, -17.35471282991112574 ) ) ;
#13186 = CARTESIAN_POINT ( 'NONE',  ( -9.525302004199998507, -18.50000000000000000, -21.25953894639999930 ) ) ;
#13187 = CIRCLE ( 'NONE', #26691, 3.499999999999999556 ) ;
#13188 = CARTESIAN_POINT ( 'NONE',  ( -15.53338745080000116, -83.75000000000000000, -28.43367500519999780 ) ) ;
#13189 = CARTESIAN_POINT ( 'NONE',  ( 20.91081638819999711, -19.16559685929999901, 9.386484010540000256 ) ) ;
#13190 = CARTESIAN_POINT ( 'NONE',  ( 10.31091299859999921, -69.35841635670000471, -25.71411929689999809 ) ) ;
#13191 = CARTESIAN_POINT ( 'NONE',  ( -17.05590440810569675, -97.60610394651996558, 10.26113453133471154 ) ) ;
#13192 = ORIENTED_EDGE ( 'NONE', *, *, #5714, .T. ) ;
#13193 = CARTESIAN_POINT ( 'NONE',  ( -12.84659744679999882, -72.82938648530000592, -25.64625568420000334 ) ) ;
#13194 = CARTESIAN_POINT ( 'NONE',  ( 26.72438235069999735, -72.61900956739999913, -10.64645804510000104 ) ) ;
#13195 = CARTESIAN_POINT ( 'NONE',  ( -11.91096112960000042, -101.1700440390000040, -9.606277335259999717 ) ) ;
#13196 = CARTESIAN_POINT ( 'NONE',  ( 22.82359378984540399, -61.65624515446846488, -7.265242739030600916 ) ) ;
#13197 = ORIENTED_EDGE ( 'NONE', *, *, #27129, .F. ) ;
#13198 = TOROIDAL_SURFACE ( 'NONE', #7655, 3.750000000000000000, 1.000000000000000000 ) ;
#13199 = B_SPLINE_CURVE_WITH_KNOTS ( 'NONE', 3,
 ( #6703, #12794, #9016, #21995, #19651, #21702, #1751, #10593, #1899, #19511, #19939, #15258, #24179, #28395, #2043, #10886, #26227, #17335, #8431, #15117, #12, #19796, #28675, #6254, #8708, #24029, #4064, #8859, #28543, #17625, #26511, #4365, #22883 ),
 .UNSPECIFIED., .F., .F.,
 ( 4, 2, 1, 1, 2, 2, 1, 1, 1, 2, 2, 2, 1, 1, 2, 2, 1, 1, 2, 2, 4 ),
 ( 0.000000000000000000, 0.06250000000002318978, 0.09375000000002295386, 0.1093750000000323352, 0.1171875000000370259, 0.1250000000000417166, 0.1875000000000381362, 0.2187500000000363598, 0.2343750000000414946, 0.2421875000000440759, 0.2500000000000466294, 0.3750000000000206501, 0.4375000000000118794, 0.4687500000000074385, 0.4843750000000081601, 0.5000000000000087708, 0.6250000000000012212, 0.6874999999999975575, 0.7187499999999973355, 0.7499999999999971134, 1.000000000000000000 ),
 .UNSPECIFIED. ) ;
#13200 = EDGE_CURVE ( 'NONE', #18713, #19738, #22432, .T. ) ;
#13201 = CIRCLE ( 'NONE', #9949, 9.500000000000001776 ) ;
#13202 = DIRECTION ( 'NONE',  ( 1.000000000000000000, 0.000000000000000000, 0.000000000000000000 ) ) ;
#13203 = VERTEX_POINT ( 'NONE', #4 ) ;
#13204 = DIRECTION ( 'NONE',  ( 0.000000000000000000, 1.000000000000000000, 0.000000000000000000 ) ) ;
#13205 = CARTESIAN_POINT ( 'NONE',  ( -40.65853658540000026, -84.50000000000000000, 6.717799458580000049 ) ) ;
#13206 = DIRECTION ( 'NONE',  ( -0.7320471826101231372, 0.000000000000000000, 0.6812539338841141490 ) ) ;
#13207 = MECHANICAL_DESIGN_GEOMETRIC_PRESENTATION_REPRESENTATION (  '', ( #23473 ), #21152 ) ;
#13208 = CARTESIAN_POINT ( 'NONE',  ( 12.03625741000000104, -92.92010097569999516, 27.59856934729999978 ) ) ;
#13209 = VERTEX_POINT ( 'NONE', #21987 ) ;
#13210 = ADVANCED_FACE ( 'NONE', ( #2477 ), #6416, .T. ) ;
#13211 = DIRECTION ( 'NONE',  ( 1.000000000000000000, 0.000000000000000000, 0.000000000000000000 ) ) ;
#13212 = TOROIDAL_SURFACE ( 'NONE', #3486, 15.50000000000000000, 0.5000000000000000000 ) ;
#13213 = ORIENTED_EDGE ( 'NONE', *, *, #3589, .T. ) ;
#13214 = CARTESIAN_POINT ( 'NONE',  ( 24.09844107120000345, -93.07154584180000256, 12.17654209520000030 ) ) ;
#13215 = CARTESIAN_POINT ( 'NONE',  ( -15.21246488650000117, -100.9405327639999967, 4.776672761669999545 ) ) ;
#13216 = ORIENTED_EDGE ( 'NONE', *, *, #2625, .F. ) ;
#13217 = DIRECTION ( 'NONE',  ( -0.000000000000000000, 1.000000000000000000, 0.000000000000000000 ) ) ;
#13218 = CARTESIAN_POINT ( 'NONE',  ( 19.43643804750000115, -34.66800313659999944, -8.988996126470000902 ) ) ;
#13219 = AXIS2_PLACEMENT_3D ( 'NONE', #18152, #701, #2722 ) ;
#13220 = CARTESIAN_POINT ( 'NONE',  ( 12.39757656149999931, -101.6484611540000031, -10.11435096289999969 ) ) ;
#13221 = CARTESIAN_POINT ( 'NONE',  ( -11.53802887301132607, -59.75213514187333175, -22.74397602207726266 ) ) ;
#13222 = FACE_OUTER_BOUND ( 'NONE', #9317, .T. ) ;
#13223 = EDGE_LOOP ( 'NONE', ( #4836, #19018, #6654, #21111 ) ) ;
#13224 = CARTESIAN_POINT ( 'NONE',  ( 36.31506118079999368, -74.00004962420000254, -14.00376701259999912 ) ) ;
#13225 = CARTESIAN_POINT ( 'NONE',  ( 12.97071070920000047, -101.3090757639999993, -9.810351643989998038 ) ) ;
#13226 = LINE ( 'NONE', #19928, #22739 ) ;
#13227 = CARTESIAN_POINT ( 'NONE',  ( 0.000000000000000000, -23.00000000000000000, 0.000000000000000000 ) ) ;
#13228 = CARTESIAN_POINT ( 'NONE',  ( 9.720255118479999012, -72.82938648530000592, -26.98670296669999757 ) ) ;
#13229 = CARTESIAN_POINT ( 'NONE',  ( 21.47791241899999903, -36.56811125080000835, -7.356933755090000027 ) ) ;
#13230 = ORIENTED_EDGE ( 'NONE', *, *, #25925, .T. ) ;
#13231 = CARTESIAN_POINT ( 'NONE',  ( -6.296318341739999269, -102.8486084350000027, -11.52533341650000054 ) ) ;
#13232 = EDGE_CURVE ( 'NONE', #26990, #12325, #8851, .T. ) ;
#13233 = AXIS2_PLACEMENT_3D ( 'NONE', #22631, #25109, #2671 ) ;
#13234 = DIRECTION ( 'NONE',  ( 0.000000000000000000, -1.000000000000000000, 0.000000000000000000 ) ) ;
#13235 = CARTESIAN_POINT ( 'NONE',  ( 1.723886190540000030, -92.49999926799999628, -29.27157131740000295 ) ) ;
#13236 = CARTESIAN_POINT ( 'NONE',  ( 21.42899162430000359, -18.50000000000000000, 8.464585110160001591 ) ) ;
#13237 = DIRECTION ( 'NONE',  ( 0.000000000000000000, 1.000000000000000000, 0.000000000000000000 ) ) ;
#13238 = EDGE_CURVE ( 'NONE', #11594, #20314, #20391, .T. ) ;
#13239 = UNCERTAINTY_MEASURE_WITH_UNIT (LENGTH_MEASURE( 1.000000000000000082E-05 ), #11280, 'distance_accuracy_value', 'NONE');
#13240 = AXIS2_PLACEMENT_3D ( 'NONE', #3680, #18862, #17077 ) ;
#13241 = ADVANCED_FACE ( 'NONE', ( #6541 ), #22736, .F. ) ;
#13242 = FACE_OUTER_BOUND ( 'NONE', #16968, .T. ) ;
#13243 = ORIENTED_EDGE ( 'NONE', *, *, #3255, .T. ) ;
#13244 = CARTESIAN_POINT ( 'NONE',  ( 19.14326094509999976, -98.26007807750001177, -0.6345988924250000052 ) ) ;
#13246 = EDGE_LOOP ( 'NONE', ( #13608, #11996, #4989, #435 ) ) ;
#13245 = B_SPLINE_CURVE_WITH_KNOTS ( 'NONE', 3,
 ( #2408, #11264, #11411, #11557, #20466, #9088 ),
 .UNSPECIFIED., .F., .F.,
 ( 4, 2, 4 ),
 ( 0.000000000000000000, 0.5000000000000000000, 1.000000000000000000 ),
 .UNSPECIFIED. ) ;
#13247 = LINE ( 'NONE', #20255, #27508 ) ;
#13248 = CARTESIAN_POINT ( 'NONE',  ( -42.56117883860000006, -65.49083508809999898, -0.5420286502529999551 ) ) ;
#13249 = EDGE_LOOP ( 'NONE', ( #8079, #8564, #987, #6454 ) ) ;
#13250 = CARTESIAN_POINT ( 'NONE',  ( 30.91973185770000043, -72.00365067099998839, -22.05221014440000005 ) ) ;
#13251 = ORIENTED_EDGE ( 'NONE', *, *, #9843, .T. ) ;
#13252 = DIRECTION ( 'NONE',  ( 0.000000000000000000, -1.000000000000000000, 0.000000000000000000 ) ) ;
#13253 = CARTESIAN_POINT ( 'NONE',  ( 9.885503723209998483, -36.00000000000000000, -20.33566493420000043 ) ) ;
#13254 = DIRECTION ( 'NONE',  ( 0.000000000000000000, 1.000000000000000000, 0.000000000000000000 ) ) ;
#13255 = CARTESIAN_POINT ( 'NONE',  ( -9.949002106569999171, -18.50000000000000000, -18.82416880939999970 ) ) ;
#13256 = CARTESIAN_POINT ( 'NONE',  ( 47.20252187080182438, -79.30480005358090523, -1.049247932104649506 ) ) ;
#13257 = ORIENTED_EDGE ( 'NONE', *, *, #2860, .F. ) ;
#13258 = CARTESIAN_POINT ( 'NONE',  ( 10.49047732170000025, -92.65509162889999573, -25.64082967920000300 ) ) ;
#13259 = CARTESIAN_POINT ( 'NONE',  ( 24.24555580839999891, -27.00851495059999863, 1.474038313269999900 ) ) ;
#13260 = LINE ( 'NONE', #13113, #8781 ) ;
#13261 = CARTESIAN_POINT ( 'NONE',  ( -32.77174708219999388, -74.50000000000000000, -21.60034937629999874 ) ) ;
#13262 = ORIENTED_EDGE ( 'NONE', *, *, #9903, .T. ) ;
#13263 = CARTESIAN_POINT ( 'NONE',  ( -1.084624312358362319, -65.04696244768176427, -25.11520602852569439 ) ) ;
#13264 = CARTESIAN_POINT ( 'NONE',  ( -17.96353918029999974, -93.86098520749999352, 18.31830939139999970 ) ) ;
#13265 = CARTESIAN_POINT ( 'NONE',  ( 7.138278311610000593, -60.29602444460000044, -22.47789715730000282 ) ) ;
#13266 = ORIENTED_EDGE ( 'NONE', *, *, #11083, .T. ) ;
#13267 = CARTESIAN_POINT ( 'NONE',  ( 25.14694229440000228, -65.07443093669999712, -0.3759436444569999591 ) ) ;
#13268 = CARTESIAN_POINT ( 'NONE',  ( 0.7855938671740000379, -100.2511768809999921, -16.66646386170000227 ) ) ;
#13269 = CARTESIAN_POINT ( 'NONE',  ( 24.83705061268925007, -74.21720588690770626, -30.28267051683909372 ) ) ;
#13270 = CARTESIAN_POINT ( 'NONE',  ( -12.19593855029999929, -68.24200910160000433, -24.12327046570000277 ) ) ;
#13271 = EDGE_CURVE ( 'NONE', #22982, #10474, #22138, .T. ) ;
#13272 = CARTESIAN_POINT ( 'NONE',  ( -11.53652411959999924, -49.87340317219999974, -20.08903528430000307 ) ) ;
#13273 = EDGE_CURVE ( 'NONE', #139, #23006, #7836, .T. ) ;
#13274 = LINE ( 'NONE', #24365, #12448 ) ;
#13275 = AXIS2_PLACEMENT_3D ( 'NONE', #26832, #15728, #24641 ) ;
#13276 = EDGE_CURVE ( 'NONE', #15187, #23314, #8284, .T. ) ;
#13277 = EDGE_CURVE ( 'NONE', #14660, #5636, #15231, .T. ) ;
#13278 = ORIENTED_EDGE ( 'NONE', *, *, #17232, .F. ) ;
#13279 = B_SPLINE_CURVE_WITH_KNOTS ( 'NONE', 5,
 ( #10168, #14828, #19087, #21143, #21549, #27973 ),
 .UNSPECIFIED., .F., .F.,
 ( 6, 6 ),
 ( -46.92787229070000166, 0.000000000000000000 ),
 .UNSPECIFIED. ) ;
#13280 = CARTESIAN_POINT ( 'NONE',  ( 28.25594642106975130, -92.69183043804710564, 11.48302245628102192 ) ) ;
#13281 = CARTESIAN_POINT ( 'NONE',  ( -42.25000000000000000, -65.63577453799999262, 0.7216878364880000563 ) ) ;
#13282 = CARTESIAN_POINT ( 'NONE',  ( -41.99796191249483712, -65.72812594248435403, -0.9281908455079398435 ) ) ;
#13283 = ORIENTED_EDGE ( 'NONE', *, *, #21706, .F. ) ;
#13284 = AXIS2_PLACEMENT_3D ( 'NONE', #21018, #25394, #20735 ) ;
#13285 = PLANE ( 'NONE',  #8943 ) ;
#13286 = CARTESIAN_POINT ( 'NONE',  ( 20.31493464609999933, -22.48307172219999828, -8.521724737190000454 ) ) ;
#13287 = CARTESIAN_POINT ( 'NONE',  ( 22.20081257617079018, -19.46558063074879996, 0.3071883854471966213 ) ) ;
#13288 = ORIENTED_EDGE ( 'NONE', *, *, #10404, .T. ) ;
#13289 = DIRECTION ( 'NONE',  ( 1.000000000000000000, 0.000000000000000000, 0.000000000000000000 ) ) ;
#13290 = CARTESIAN_POINT ( 'NONE',  ( -13.12737311083959568, -100.1240332945601779, -11.11848609902146201 ) ) ;
#13291 = ORIENTED_EDGE ( 'NONE', *, *, #21202, .F. ) ;
#13292 = CARTESIAN_POINT ( 'NONE',  ( 9.275138546780000937, -35.95833528409999502, -19.65753135889999825 ) ) ;
#13293 = CARTESIAN_POINT ( 'NONE',  ( 26.79489351000000141, -92.68584525839999344, -12.41053404230000190 ) ) ;
#13294 = CARTESIAN_POINT ( 'NONE',  ( 8.708727887559998493, -98.58239820560001476, 16.48836518959999964 ) ) ;
#13295 = CARTESIAN_POINT ( 'NONE',  ( 21.89545778420000133, -18.85485920039999996, -0.1610960871889999813 ) ) ;
#13296 = CARTESIAN_POINT ( 'NONE',  ( -0.5455003419149999644, -98.53908914310000000, -18.73905742539999864 ) ) ;
#13297 = CARTESIAN_POINT ( 'NONE',  ( 14.28478035945855140, -92.50000000000000000, 26.94835746195996862 ) ) ;
#13298 = ORIENTED_EDGE ( 'NONE', *, *, #5286, .F. ) ;
#13299 = CARTESIAN_POINT ( 'NONE',  ( 11.45697295529999948, -101.0535396030000044, -10.57669106610000220 ) ) ;
#13300 = CARTESIAN_POINT ( 'NONE',  ( -13.08672874900000060, -19.48537664570000061, 19.65389566680000044 ) ) ;
#13301 = DIRECTION ( 'NONE',  ( 1.000000000000000000, 0.000000000000000000, 0.000000000000000000 ) ) ;
#13302 = CARTESIAN_POINT ( 'NONE',  ( -13.66168260340000096, -72.00000000000000000, -27.27344781959999764 ) ) ;
#13303 = LINE ( 'NONE', #24250, #8752 ) ;
#13304 = CARTESIAN_POINT ( 'NONE',  ( -12.31890027530000076, -66.79872818030000303, -23.02601073709999824 ) ) ;
#13305 = DIRECTION ( 'NONE',  ( 0.000000000000000000, -1.000000000000000000, 0.000000000000000000 ) ) ;
#13306 = CARTESIAN_POINT ( 'NONE',  ( 27.32142465356705330, -93.09721478964854668, 9.756329643219576297 ) ) ;
#13307 = ORIENTED_EDGE ( 'NONE', *, *, #16973, .F. ) ;
#13308 = ADVANCED_FACE ( 'NONE', ( #2323 ), #18051, .T. ) ;
#13309 = LINE ( 'NONE', #24401, #942 ) ;
#13311 = CARTESIAN_POINT ( 'NONE',  ( 7.889779489369998622, -101.3196660750000149, 13.95717439989999953 ) ) ;
#13310 =( REPRESENTATION_RELATIONSHIP ('NONE','NONE', #26008, #10908 ) REPRESENTATION_RELATIONSHIP_WITH_TRANSFORMATION ( #20547 )SHAPE_REPRESENTATION_RELATIONSHIP( ) );
#13312 = EDGE_CURVE ( 'NONE', #13903, #640, #21791, .T. ) ;
#13313 = VERTEX_POINT ( 'NONE', #153 ) ;
#13314 = CARTESIAN_POINT ( 'NONE',  ( -12.24789267649999935, -65.07443092999999124, 21.96586367309999943 ) ) ;
#13315 = CARTESIAN_POINT ( 'NONE',  ( -1.878699226219999963, -64.89165510060000486, -25.21178815420000063 ) ) ;
#13316 = CARTESIAN_POINT ( 'NONE',  ( -24.00581540240000322, -94.71481161159999829, -4.132755290490000455 ) ) ;
#13317 = CARTESIAN_POINT ( 'NONE',  ( -19.68721726160000074, -53.84414347720000649, 12.34260908240000099 ) ) ;
#13318 = CARTESIAN_POINT ( 'NONE',  ( -10.93437413680000070, -19.50000027030000282, -21.85842452360000010 ) ) ;
#13319 = VERTEX_POINT ( 'NONE', #9006 ) ;
#13320 = CARTESIAN_POINT ( 'NONE',  ( -6.285925807789999986, -101.6484611540000031, 14.71350185169999847 ) ) ;
#13321 = CARTESIAN_POINT ( 'NONE',  ( 28.11272953839543121, -74.46129532805292683, -27.39515278475305493 ) ) ;
#13322 = CARTESIAN_POINT ( 'NONE',  ( 7.135466578850000019, -73.50000064450000536, -38.71640869449999656 ) ) ;
#13323 = ORIENTED_EDGE ( 'NONE', *, *, #13548, .F. ) ;
#13324 = CARTESIAN_POINT ( 'NONE',  ( -35.88566914520000495, -77.00000000000000000, -26.69328098980000163 ) ) ;
#13325 = CARTESIAN_POINT ( 'NONE',  ( -40.65853658540000026, -84.50000000000000000, -6.717799458580000049 ) ) ;
#13326 = CARTESIAN_POINT ( 'NONE',  ( 22.61819354930000259, -45.94038128989999592, 10.08865270770000144 ) ) ;
#13327 = CARTESIAN_POINT ( 'NONE',  ( 4.500000000000000000, -12.50000000000000000, 40.50000000000000000 ) ) ;
#13328 = CARTESIAN_POINT ( 'NONE',  ( 24.20411630889999799, -92.55031878719999838, -15.29912012159999968 ) ) ;
#13329 = CARTESIAN_POINT ( 'NONE',  ( 20.51027266010000005, -57.91805314620000189, 11.21560917149999881 ) ) ;
#13330 = CARTESIAN_POINT ( 'NONE',  ( 17.60755106127235692, -95.57586274903817980, 14.14554066879750671 ) ) ;
#13331 = CARTESIAN_POINT ( 'NONE',  ( 14.08191940870000103, -97.83383802260000550, -14.15749693589999758 ) ) ;
#13332 = VERTEX_POINT ( 'NONE', #15703 ) ;
#13333 = FACE_OUTER_BOUND ( 'NONE', #10973, .T. ) ;
#13334 = CARTESIAN_POINT ( 'NONE',  ( -43.94912152850000098, -63.50000000000000000, -2.157414923720000210 ) ) ;
#13335 = CARTESIAN_POINT ( 'NONE',  ( -12.00964495180000036, -100.4731125450000064, -10.87550195419999888 ) ) ;
#13336 = CARTESIAN_POINT ( 'NONE',  ( 0.000000000000000000, -92.50000000000000000, 0.000000000000000000 ) ) ;
#13337 = CARTESIAN_POINT ( 'NONE',  ( 22.77210041255538187, -61.43103207892549023, -7.246012015154788877 ) ) ;
#13338 = ORIENTED_EDGE ( 'NONE', *, *, #15956, .T. ) ;
#13339 = EDGE_CURVE ( 'NONE', #12657, #1944, #24763, .T. ) ;
#13340 = ADVANCED_FACE ( 'NONE', ( #4799 ), #25534, .F. ) ;
#13341 = B_SPLINE_CURVE_WITH_KNOTS ( 'NONE', 5,
 ( #25982, #6298, #15163, #23800, #3835, #12699, #21613, #1666, #19418, #28299, #26708, #15308, #2531, #24225, #15908, #4853, #4410, #4698 ),
 .UNSPECIFIED., .F., .F.,
 ( 6, 3, 3, 3, 3, 6 ),
 ( 0.000000000000000000, 1.123597682109999996, 2.251105814029999763, 3.378920982540000395, 4.507089344450000645, 5.576980695509999642 ),
 .UNSPECIFIED. ) ;
#13342 = PLANE ( 'NONE',  #4214 ) ;
#13343 = CARTESIAN_POINT ( 'NONE',  ( -32.18652848360000007, -74.02659082439998883, -22.03329363239999950 ) ) ;
#13344 = ORIENTED_EDGE ( 'NONE', *, *, #13819, .F. ) ;
#13345 = CIRCLE ( 'NONE', #25021, 0.4999999999999991118 ) ;
#13346 = DIRECTION ( 'NONE',  ( 0.000000000000000000, 1.000000000000000000, 0.000000000000000000 ) ) ;
#13347 = TOROIDAL_SURFACE ( 'NONE', #15205, 21.14285714289999873, 0.5000000000000000000 ) ;
#13348 = DIRECTION ( 'NONE',  ( 0.000000000000000000, 1.000000000000000000, 0.000000000000000000 ) ) ;
#13349 = FACE_OUTER_BOUND ( 'NONE', #19882, .T. ) ;
#13350 = ORIENTED_EDGE ( 'NONE', *, *, #2125, .T. ) ;
#13351 = DIRECTION ( 'NONE',  ( 0.000000000000000000, 1.000000000000000000, 0.000000000000000000 ) ) ;
#13352 = CARTESIAN_POINT ( 'NONE',  ( 0.000000000000000000, -6.000000000000000000, 0.000000000000000000 ) ) ;
#13353 = ORIENTED_EDGE ( 'NONE', *, *, #24715, .F. ) ;
#13354 = FACE_OUTER_BOUND ( 'NONE', #10697, .T. ) ;
#13355 = CARTESIAN_POINT ( 'NONE',  ( 21.86954465750000054, -93.60791045439999891, 13.04854595950000018 ) ) ;
#13356 = DIRECTION ( 'NONE',  ( 1.000000000000000000, 0.000000000000000000, 0.000000000000000000 ) ) ;
#13357 = VERTEX_POINT ( 'NONE', #24609 ) ;
#13358 = CARTESIAN_POINT ( 'NONE',  ( 16.58537890990000108, -94.98812477769999418, 16.93952572510000110 ) ) ;
#13359 = CARTESIAN_POINT ( 'NONE',  ( 22.56940788859976266, -57.43018266628944701, 10.15711811299984646 ) ) ;
#13360 = AXIS2_PLACEMENT_3D ( 'NONE', #26138, #28596, #26284 ) ;
#13361 = EDGE_CURVE ( 'NONE', #11126, #258, #23652, .T. ) ;
#13362 = CARTESIAN_POINT ( 'NONE',  ( 9.165580138570000202, -36.00000000019999646, -20.59810116059999885 ) ) ;
#13363 = CARTESIAN_POINT ( 'NONE',  ( -18.79536340909999836, -92.66001714109999909, -20.78146695779999931 ) ) ;
#13364 = FACE_OUTER_BOUND ( 'NONE', #23017, .T. ) ;
#13365 = VERTEX_POINT ( 'NONE', #22581 ) ;
#13366 = CARTESIAN_POINT ( 'NONE',  ( -1.228311966399999955, -101.1461874320000049, -16.11255545180000226 ) ) ;
#13367 = CARTESIAN_POINT ( 'NONE',  ( -4.439198032609999743E-16, -77.00000000000000000, 47.25000000000000000 ) ) ;
#13368 = CARTESIAN_POINT ( 'NONE',  ( -39.23650411529999360, -73.50070240710000746, 7.229383731089999543 ) ) ;
#13369 = CARTESIAN_POINT ( 'NONE',  ( -21.62384810780000066, -74.29049705580000307, -32.72083640759999668 ) ) ;
#13370 = CARTESIAN_POINT ( 'NONE',  ( -5.069308693793000309, -98.61679376083424131, -19.10643818412435024 ) ) ;
#13371 = CIRCLE ( 'NONE', #22724, 7.750000000000000000 ) ;
#13372 = CARTESIAN_POINT ( 'NONE',  ( -43.75000000000000000, -79.00000000000000000, 0.000000000000000000 ) ) ;
#13373 = CARTESIAN_POINT ( 'NONE',  ( -7.627568735119999666, -74.00000000000000000, 38.62788659690000515 ) ) ;
#13374 = CARTESIAN_POINT ( 'NONE',  ( -18.19213461030000190, -18.50000000000000000, 11.15819842919999871 ) ) ;
#13375 = ORIENTED_EDGE ( 'NONE', *, *, #12420, .F. ) ;
#13377 = EDGE_CURVE ( 'NONE', #12777, #5069, #3206, .T. ) ;
#13376 = DIRECTION ( 'NONE',  ( 0.000000000000000000, 1.000000000000000000, 0.000000000000000000 ) ) ;
#13378 = CARTESIAN_POINT ( 'NONE',  ( 9.307782790770433579, -57.43039233035062097, -22.95932714880148851 ) ) ;
#13379 = CARTESIAN_POINT ( 'NONE',  ( -23.81726931088821786, -92.83865970263468625, -19.05223594286923117 ) ) ;
#13380 = CARTESIAN_POINT ( 'NONE',  ( 16.13266937400000245, -83.75000000000000000, 29.53065320760000034 ) ) ;
#13381 = CARTESIAN_POINT ( 'NONE',  ( 22.60879290213893711, -95.55433702443635013, -0.3969505341440314194 ) ) ;
#13382 = EDGE_CURVE ( 'NONE', #28507, #9115, #2624, .T. ) ;
#13383 = AXIS2_PLACEMENT_3D ( 'NONE', #17274, #6485, #4149 ) ;
#13384 = SHAPE_DEFINITION_REPRESENTATION ( #3858, #19699 ) ;
#13385 = CIRCLE ( 'NONE', #11536, 0.5000000000000004441 ) ;
#13386 = DIRECTION ( 'NONE',  ( -0.8775825618903722036, 0.000000000000000000, 0.4794255386042041156 ) ) ;
#13387 = ORIENTED_EDGE ( 'NONE', *, *, #25925, .F. ) ;
#13388 = CARTESIAN_POINT ( 'NONE',  ( 15.50925568500000118, -100.9197081840000010, 1.894556133100000039 ) ) ;
#13389 = ORIENTED_EDGE ( 'NONE', *, *, #23278, .T. ) ;
#13390 = AXIS2_PLACEMENT_3D ( 'NONE', #3518, #12374, #21282 ) ;
#13391 = CARTESIAN_POINT ( 'NONE',  ( -13.85849061559999917, -57.40875702409999803, 21.24403769210000092 ) ) ;
#13392 = CARTESIAN_POINT ( 'NONE',  ( 5.258016244619999627E-13, -84.50000000000000000, -5.364597654989999396E-13 ) ) ;
#13393 = VERTEX_POINT ( 'NONE', #18199 ) ;
#13394 = CARTESIAN_POINT ( 'NONE',  ( 13.43278536909999943, -96.09419472199999745, 17.29930431160000026 ) ) ;
#13395 = PRODUCT_DEFINITION_SHAPE ( 'NONE', 'NONE',  #28803 ) ;
#13396 = EDGE_CURVE ( 'NONE', #3543, #21689, #10130, .T. ) ;
#13397 = CARTESIAN_POINT ( 'NONE',  ( -13.82310862920000005, -74.00000000000000000, 36.20061004769999613 ) ) ;
#13398 = CARTESIAN_POINT ( 'NONE',  ( 9.374849361280000792, -94.98812477599999227, -22.63660904189999812 ) ) ;
#13399 = CARTESIAN_POINT ( 'NONE',  ( -7.325370793560000315, -72.00000000000000000, -24.94672208400000102 ) ) ;
#13400 = CARTESIAN_POINT ( 'NONE',  ( -16.97872427700000131, -99.83167715590001023, 3.440838554449999531 ) ) ;
#13401 = CARTESIAN_POINT ( 'NONE',  ( -29.74393970790053388, -92.83160374581187568, 6.748930471038662837 ) ) ;
#13402 = CARTESIAN_POINT ( 'NONE',  ( 47.25000000000000000, -79.00000000000000000, -7.709388683000000122E-13 ) ) ;
#13403 = ORIENTED_EDGE ( 'NONE', *, *, #21286, .F. ) ;
#13404 = VECTOR ( 'NONE', #17473, 1000.000000000000000 ) ;
#13405 = DIRECTION ( 'NONE',  ( 0.000000000000000000, -1.000000000000000000, 0.000000000000000000 ) ) ;
#13406 = CARTESIAN_POINT ( 'NONE',  ( -20.38196585287909457, -61.35680953179207364, 12.44223151297076058 ) ) ;
#13407 = AXIS2_PLACEMENT_3D ( 'NONE', #19713, #15037, #17537 ) ;
#13408 = CARTESIAN_POINT ( 'NONE',  ( -12.80006882320263450, -92.59055325462904307, 27.68408069405598226 ) ) ;
#13409 = VERTEX_POINT ( 'NONE', #9593 ) ;
#13410 = EDGE_CURVE ( 'NONE', #8136, #15352, #28157, .T. ) ;
#13411 = DIRECTION ( 'NONE',  ( 1.000000000000000000, 0.000000000000000000, 0.000000000000000000 ) ) ;
#13412 = FACE_OUTER_BOUND ( 'NONE', #18168, .T. ) ;
#13413 = CARTESIAN_POINT ( 'NONE',  ( -22.65530694619999963, -72.00000000000000000, 18.22957389299999775 ) ) ;
#13414 = ORIENTED_EDGE ( 'NONE', *, *, #13776, .T. ) ;
#13415 = CARTESIAN_POINT ( 'NONE',  ( 27.46886385830000066, -68.58900653949999082, 1.888124754229999924 ) ) ;
#13416 = CARTESIAN_POINT ( 'NONE',  ( -23.32456840009999866, -92.51542729400000553, -18.96923773310000172 ) ) ;
#13417 = CARTESIAN_POINT ( 'NONE',  ( 0.6800711189380000965, -100.1459902240000019, -16.94139632559999953 ) ) ;
#13418 = CARTESIAN_POINT ( 'NONE',  ( 28.97576656849999566, -38.00000000000000000, -19.97576656850000987 ) ) ;
#13419 = FACE_OUTER_BOUND ( 'NONE', #2375, .T. ) ;
#13420 = CARTESIAN_POINT ( 'NONE',  ( 23.64759572430000034, -63.25393901619999326, -9.386700920010000004 ) ) ;
#13421 = CARTESIAN_POINT ( 'NONE',  ( 0.000000000000000000, -82.25000000000000000, 40.00000000000000000 ) ) ;
#13422 = DIRECTION ( 'NONE',  ( 0.09756097560976997873, 0.000000000000000000, -0.9952295494196653491 ) ) ;
#13423 = CIRCLE ( 'NONE', #16706, 3.000000000000000000 ) ;
#13424 = ORIENTED_EDGE ( 'NONE', *, *, #5792, .T. ) ;
#13425 = CIRCLE ( 'NONE', #23235, 55.67692378859999991 ) ;
#13426 = CARTESIAN_POINT ( 'NONE',  ( -2.619606461630943350, -19.18584080450747464, -24.29997790279570680 ) ) ;
#13427 = CARTESIAN_POINT ( 'NONE',  ( -43.08431406180000067, -65.21397798589998729, 0.2399963883289999989 ) ) ;
#13428 = AXIS2_PLACEMENT_3D ( 'NONE', #1464, #6534, #15391 ) ;
#13429 = CARTESIAN_POINT ( 'NONE',  ( 30.45033996220000105, -74.00000000000000000, 1.805359716810000181 ) ) ;
#13430 = ORIENTED_EDGE ( 'NONE', *, *, #15898, .F. ) ;
#13431 = CARTESIAN_POINT ( 'NONE',  ( 23.27561534246691011, -92.52048598158071968, -19.71030172176314821 ) ) ;
#13432 = DIRECTION ( 'NONE',  ( -0.5000000000001900702, 0.000000000000000000, 0.8660254037843290176 ) ) ;
#13433 = CARTESIAN_POINT ( 'NONE',  ( 22.62855517031298547, -19.47102808830224419, 0.9225138090183480077 ) ) ;
#13434 = CARTESIAN_POINT ( 'NONE',  ( -6.842114547430000471, -101.1030539030000028, 13.83820396960000032 ) ) ;
#13435 = ORIENTED_EDGE ( 'NONE', *, *, #4032, .F. ) ;
#13436 = FACE_OUTER_BOUND ( 'NONE', #8037, .T. ) ;
#13437 = CARTESIAN_POINT ( 'NONE',  ( 8.295955541540001477, -37.60239178479999822, -21.68561411610000178 ) ) ;
#13438 = CARTESIAN_POINT ( 'NONE',  ( 21.37812247595803328, -35.07876462143099161, -7.265514940539457456 ) ) ;
#13439 = EDGE_CURVE ( 'NONE', #2729, #9504, #5525, .T. ) ;
#13440 = CARTESIAN_POINT ( 'NONE',  ( 6.944463756510000252, -99.57787269160000676, 15.90826982280000124 ) ) ;
#13441 = DIRECTION ( 'NONE',  ( 1.000000000000000000, 0.000000000000000000, 0.000000000000000000 ) ) ;
#13442 = CARTESIAN_POINT ( 'NONE',  ( -7.441474119920000518, -94.70873613630000420, -22.49466058249999989 ) ) ;
#13443 = AXIS2_PLACEMENT_3D ( 'NONE', #6824, #15687, #13356 ) ;
#13444 = CARTESIAN_POINT ( 'NONE',  ( -20.00661640924422713, -92.56492639285779944, -23.02161043673221030 ) ) ;
#13445 = ORIENTED_EDGE ( 'NONE', *, *, #23090, .F. ) ;
#13446 = ADVANCED_FACE ( 'NONE', ( #16145 ), #16203, .T. ) ;
#13447 = CARTESIAN_POINT ( 'NONE',  ( -14.86197080470000209, -100.8869818489999943, 4.957595453540000641 ) ) ;
#13448 = CARTESIAN_POINT ( 'NONE',  ( -14.19924994259999984, -18.50000000000000000, 19.48093193789999944 ) ) ;
#13449 = CARTESIAN_POINT ( 'NONE',  ( -13.46646228700000059, -101.3150700380000018, -9.098096927170001180 ) ) ;
#13450 = EDGE_CURVE ( 'NONE', #15112, #1700, #26445, .T. ) ;
#13451 = AXIS2_PLACEMENT_3D ( 'NONE', #7824, #10115, #5352 ) ;
#13452 = CIRCLE ( 'NONE', #944, 1.000000000000000888 ) ;
#13453 = DIRECTION ( 'NONE',  ( 0.9952295494196653491, 0.000000000000000000, 0.09756097560976997873 ) ) ;
#13454 = CARTESIAN_POINT ( 'NONE',  ( -11.35954001540000036, -79.50000000000000000, 45.25000000000000000 ) ) ;
#13455 = CARTESIAN_POINT ( 'NONE',  ( -9.476764215410000247, -84.00000000000000000, -38.08875739639999836 ) ) ;
#13456 = CARTESIAN_POINT ( 'NONE',  ( 0.000000000000000000, -39.32601556110000018, 0.000000000000000000 ) ) ;
#13457 = CARTESIAN_POINT ( 'NONE',  ( 24.33166760675546314, -93.00000237470422348, -17.52085307207648412 ) ) ;
#13458 = CARTESIAN_POINT ( 'NONE',  ( 28.86890114233755966, -93.00000237470419506, 8.099190551483227196 ) ) ;
#13459 = EDGE_LOOP ( 'NONE', ( #1363, #3020 ) ) ;
#13460 = CARTESIAN_POINT ( 'NONE',  ( 36.30177426670000074, -74.72020149879999451, -14.92507557220000081 ) ) ;
#13461 = VERTEX_POINT ( 'NONE', #20531 ) ;
#13462 = CARTESIAN_POINT ( 'NONE',  ( -13.22200285019999910, -64.89165763220000827, 21.54860465570000017 ) ) ;
#13463 = DIRECTION ( 'NONE',  ( 0.000000000000000000, -1.000000000000000000, 0.000000000000000000 ) ) ;
#13464 = CARTESIAN_POINT ( 'NONE',  ( 7.243395527602854322, -74.19510049697379372, 40.30949744634092013 ) ) ;
#13465 = CARTESIAN_POINT ( 'NONE',  ( -23.50862730440000092, -94.59276292120000562, -3.692480652049999978 ) ) ;
#13466 = CARTESIAN_POINT ( 'NONE',  ( 38.71640881029999548, -73.50000064450000536, 7.135467304789999687 ) ) ;
#13467 = CIRCLE ( 'NONE', #8346, 0.5000000000000004441 ) ;
#13468 = AXIS2_PLACEMENT_3D ( 'NONE', #16582, #20970, #27534 ) ;
#13469 = CARTESIAN_POINT ( 'NONE',  ( -11.18016241693830182, -57.44036992075809422, -21.74842387285283962 ) ) ;
#13470 = ORIENTED_EDGE ( 'NONE', *, *, #14230, .T. ) ;
#13471 = CARTESIAN_POINT ( 'NONE',  ( -7.472970580910000216, -74.00000000000000000, -38.65569705749999940 ) ) ;
#13472 = CARTESIAN_POINT ( 'NONE',  ( 21.47791250119999873, -36.56811126780000620, -7.356933704980000321 ) ) ;
#13473 = CARTESIAN_POINT ( 'NONE',  ( 7.562806955129999231, -74.00032110550000652, -39.03038279139999389 ) ) ;
#13474 = ORIENTED_EDGE ( 'NONE', *, *, #21482, .T. ) ;
#13475 = CARTESIAN_POINT ( 'NONE',  ( 8.182334915651470197, -92.59033770621367410, 29.38229076648032034 ) ) ;
#13476 = EDGE_CURVE ( 'NONE', #5258, #26105, #10078, .T. ) ;
#13477 = CARTESIAN_POINT ( 'NONE',  ( -6.831813925109999630, -11.50000000000000000, -12.50555150689999984 ) ) ;
#13478 = CARTESIAN_POINT ( 'NONE',  ( 20.75931401429999923, -45.99312545570000310, 10.28958141490000067 ) ) ;
#13479 = DIRECTION ( 'NONE',  ( 1.000000000000000000, 0.000000000000000000, 0.000000000000000000 ) ) ;
#13480 = CARTESIAN_POINT ( 'NONE',  ( -21.60034937969999902, -74.50000000000000000, -32.77174707999999725 ) ) ;
#13481 = EDGE_CURVE ( 'NONE', #8693, #28264, #19459, .T. ) ;
#13482 = CARTESIAN_POINT ( 'NONE',  ( 20.53475900819999822, -58.35721757130000498, 11.22800283159999957 ) ) ;
#13483 = CARTESIAN_POINT ( 'NONE',  ( 8.188637977920000921, -100.9197082849999987, 13.30686163390000054 ) ) ;
#13484 = CARTESIAN_POINT ( 'NONE',  ( -16.10081869210645422, -99.27453212434828345, 7.470651185126897076 ) ) ;
#13485 = ORIENTED_EDGE ( 'NONE', *, *, #12967, .T. ) ;
#13486 = DIRECTION ( 'NONE',  ( -0.04481497625361005599, -0.9975499440283644992, -0.05371896380604832683 ) ) ;
#13487 = CARTESIAN_POINT ( 'NONE',  ( -5.873418876839999747, -101.3150700380000018, 15.15334698740000086 ) ) ;
#13488 = CARTESIAN_POINT ( 'NONE',  ( -12.94893854829999924, -100.3063911739999980, -11.10051843049999931 ) ) ;
#13489 = CARTESIAN_POINT ( 'NONE',  ( 20.42887670810370437, -19.46987374644096391, 9.579659739538350038 ) ) ;
#13490 = AXIS2_PLACEMENT_3D ( 'NONE', #22891, #18658, #16018 ) ;
#13491 = CARTESIAN_POINT ( 'NONE',  ( 10.65740927894239753, -97.98442063578340822, 16.78772980300869833 ) ) ;
#13492 = ORIENTED_EDGE ( 'NONE', *, *, #18563, .F. ) ;
#13493 = CIRCLE ( 'NONE', #20001, 3.000000000000002665 ) ;
#13494 = DIRECTION ( 'NONE',  ( -0.8775825618903722036, 0.000000000000000000, 0.4794255386042041156 ) ) ;
#13495 = ORIENTED_EDGE ( 'NONE', *, *, #1537, .F. ) ;
#13496 = DIRECTION ( 'NONE',  ( -0.3687499999999814260, 0.000000000000000000, 0.9295286103719527793 ) ) ;
#13497 = CARTESIAN_POINT ( 'NONE',  ( 25.24946330670458394, -54.25046843273178609, 1.378801988918380239 ) ) ;
#13498 = CARTESIAN_POINT ( 'NONE',  ( -18.05296197569739647, -94.57749224628196316, 16.11416072503950048 ) ) ;
#13499 = EDGE_LOOP ( 'NONE', ( #24340, #14890, #23267, #12510 ) ) ;
#13500 = ORIENTED_EDGE ( 'NONE', *, *, #18904, .T. ) ;
#13501 = CARTESIAN_POINT ( 'NONE',  ( -22.91248086744062107, -71.02126462269738738, 15.84901304865810800 ) ) ;
#13502 = CARTESIAN_POINT ( 'NONE',  ( 21.75610509370000045, -93.65023659739999573, 12.77706960399999936 ) ) ;
#13503 = CARTESIAN_POINT ( 'NONE',  ( -15.03194159329999913, -100.8816813800000034, 4.847769557329999479 ) ) ;
#13504 = EDGE_LOOP ( 'NONE', ( #26782, #9710, #17916, #24371 ) ) ;
#13505 = AXIS2_PLACEMENT_3D ( 'NONE', #26813, #4653, #22440 ) ;
#13506 = CARTESIAN_POINT ( 'NONE',  ( 16.42966103859999905, -94.59276292389999696, 17.21499949629999904 ) ) ;
#13507 = CARTESIAN_POINT ( 'NONE',  ( -22.56855420249999966, -80.00000000000000000, -32.68889834139999806 ) ) ;
#13508 = TOROIDAL_SURFACE ( 'NONE', #537, 38.75000000000000000, 0.5000000000000000000 ) ;
#13509 = EDGE_CURVE ( 'NONE', #16619, #8693, #11047, .T. ) ;
#13510 = TOROIDAL_SURFACE ( 'NONE', #4687, 6.750000000000000000, 0.5000000000000000000 ) ;
#13511 = CARTESIAN_POINT ( 'NONE',  ( 0.000000000000000000, -101.6484611540000031, 0.000000000000000000 ) ) ;
#13512 = ADVANCED_FACE ( 'NONE', ( #7428 ), #20974, .F. ) ;
#13513 = CARTESIAN_POINT ( 'NONE',  ( -14.04043131989999971, -93.59856727309998803, -21.14276827349999976 ) ) ;
#13514 = CARTESIAN_POINT ( 'NONE',  ( -23.55554542814485686, -94.54719627017709627, -3.773182801408312415 ) ) ;
#13515 = B_SPLINE_CURVE_WITH_KNOTS ( 'NONE', 5,
 ( #2229, #20145, #4551, #20441, #22636, #214 ),
 .UNSPECIFIED., .F., .F.,
 ( 6, 6 ),
 ( 0.000000000000000000, 1.000000000000000000 ),
 .UNSPECIFIED. ) ;
#13516 = ORIENTED_EDGE ( 'NONE', *, *, #20815, .F. ) ;
#13517 = EDGE_CURVE ( 'NONE', #18513, #11029, #11534, .T. ) ;
#13518 = CARTESIAN_POINT ( 'NONE',  ( -5.963907253145354304, -101.5019029710834673, 14.96613752057661806 ) ) ;
#13519 = CARTESIAN_POINT ( 'NONE',  ( -40.37845838710000379, -74.24284936579999794, 7.248115120149999591 ) ) ;
#13520 = DIRECTION ( 'NONE',  ( 0.4794255386042000078, 0.000000000000000000, 0.8775825618903743131 ) ) ;
#13521 = DIRECTION ( 'NONE',  ( 0.000000000000000000, 1.000000000000000000, 0.000000000000000000 ) ) ;
#13522 = DIRECTION ( 'NONE',  ( 0.3186522097941134612, 0.000000000000000000, 0.9478717050283378409 ) ) ;
#13523 = CARTESIAN_POINT ( 'NONE',  ( -7.588683564822256145, -74.00000000115923626, 38.71475194765147165 ) ) ;
#13524 = CARTESIAN_POINT ( 'NONE',  ( 40.65508461000000295, -80.00000000000000000, -13.75000000000000000 ) ) ;
#13525 = ORIENTED_EDGE ( 'NONE', *, *, #7861, .T. ) ;
#13526 = CARTESIAN_POINT ( 'NONE',  ( -7.441474466189999859, -94.70873790539999959, -22.49465953780000049 ) ) ;
#13527 = CARTESIAN_POINT ( 'NONE',  ( 0.000000000000000000, -33.79999999999999716, 0.000000000000000000 ) ) ;
#13528 = CARTESIAN_POINT ( 'NONE',  ( -24.14169972247601237, -92.59055325465111252, -18.63943186536354091 ) ) ;
#13529 = DIRECTION ( 'NONE',  ( 0.4794255386042040046, 0.000000000000000000, 0.8775825618903722036 ) ) ;
#13530 = CARTESIAN_POINT ( 'NONE',  ( 47.11548663039999951, -79.82827424500000291, -1.752954514250000040 ) ) ;
#13531 = AXIS2_PLACEMENT_3D ( 'NONE', #19432, #3852, #1678 ) ;
#13532 = CARTESIAN_POINT ( 'NONE',  ( -14.59972664311643697, -101.2126522312630925, 4.393265484499556450 ) ) ;
#13533 = AXIS2_PLACEMENT_3D ( 'NONE', #26081, #25942, #14719 ) ;
#13534 = AXIS2_PLACEMENT_3D ( 'NONE', #10312, #7878, #14295 ) ;
#13535 = ADVANCED_FACE ( 'NONE', ( #14120 ), #407, .F. ) ;
#13536 = DIRECTION ( 'NONE',  ( 1.000000000000000000, 0.000000000000000000, 0.000000000000000000 ) ) ;
#13537 = CARTESIAN_POINT ( 'NONE',  ( 23.36166352360000076, -57.47815920179999694, -0.2645301549009999587 ) ) ;
#13538 = CIRCLE ( 'NONE', #21020, 55.67692378859999991 ) ;
#13539 = CARTESIAN_POINT ( 'NONE',  ( -22.22906645670000003, -79.25000000000000000, -32.83566817450000030 ) ) ;
#13540 = EDGE_LOOP ( 'NONE', ( #23630, #1676, #21926, #24645 ) ) ;
#13541 = FACE_OUTER_BOUND ( 'NONE', #23558, .T. ) ;
#13542 = ORIENTED_EDGE ( 'NONE', *, *, #27055, .T. ) ;
#13543 = CARTESIAN_POINT ( 'NONE',  ( -13.76297350900000005, -49.80571413040000550, 21.08331308489999856 ) ) ;
#13544 = CYLINDRICAL_SURFACE ( 'NONE', #17, 0.7999999999999997113 ) ;
#13545 = ORIENTED_EDGE ( 'NONE', *, *, #8641, .F. ) ;
#13546 = CARTESIAN_POINT ( 'NONE',  ( 16.46460143819999900, -94.70873611929999925, 17.03825138000000194 ) ) ;
#13547 = FACE_OUTER_BOUND ( 'NONE', #5805, .T. ) ;
#13548 = EDGE_CURVE ( 'NONE', #17502, #20283, #27841, .T. ) ;
#13549 = CARTESIAN_POINT ( 'NONE',  ( 5.341700292228932057, -93.31462968041127226, -27.40505522819004369 ) ) ;
#13550 = DIRECTION ( 'NONE',  ( 0.000000000000000000, 1.000000000000000000, 0.000000000000000000 ) ) ;
#13551 = CARTESIAN_POINT ( 'NONE',  ( -41.75000000000000000, -63.30468293320000583, 1.587713240270000048 ) ) ;
#13552 = DIRECTION ( 'NONE',  ( -0.7436828042389490578, 0.000000000000000000, 0.6685326369589542628 ) ) ;
#13553 = CIRCLE ( 'NONE', #21925, 3.500000000000003109 ) ;
#13554 = CARTESIAN_POINT ( 'NONE',  ( 21.70902145223586288, -37.93282145858484000, -8.317949937562373108 ) ) ;
#13555 = EDGE_LOOP ( 'NONE', ( #12029, #3324, #394, #18777, #22569, #5639 ) ) ;
#13556 = TOROIDAL_SURFACE ( 'NONE', #7074, 18.14285714289999873, 0.5000000000000000000 ) ;
#13557 = FACE_OUTER_BOUND ( 'NONE', #22556, .T. ) ;
#13558 = AXIS2_PLACEMENT_3D ( 'NONE', #17629, #13386, #12075 ) ;
#13559 = CARTESIAN_POINT ( 'NONE',  ( -38.25000000000000000, -65.63577453799999262, -1.587713240270000048 ) ) ;
#13560 = CARTESIAN_POINT ( 'NONE',  ( 39.83391879089067800, -73.87273571681690498, 7.248098695790405444 ) ) ;
#13561 = EDGE_LOOP ( 'NONE', ( #9803, #14938, #8952, #8483 ) ) ;
#13562 = DIRECTION ( 'NONE',  ( -0.2162432783070589171, 0.000000000000000000, -0.9763395129702657771 ) ) ;
#13563 = CARTESIAN_POINT ( 'NONE',  ( -16.50487832609999828, -92.86540159979999487, 21.47928501360000197 ) ) ;
#13564 = FACE_OUTER_BOUND ( 'NONE', #3283, .T. ) ;
#13565 = ORIENTED_EDGE ( 'NONE', *, *, #1633, .T. ) ;
#13566 = CARTESIAN_POINT ( 'NONE',  ( -3.215510237749999778, -94.59276292389999696, 23.57860181210000405 ) ) ;
#13567 = CARTESIAN_POINT ( 'NONE',  ( 0.6844652716010000137, -99.85455315880000171, -17.12311058819999943 ) ) ;
#13568 = CARTESIAN_POINT ( 'NONE',  ( 21.45986210613797596, -74.01270519314725505, -32.43345270094494737 ) ) ;
#13569 = DIRECTION ( 'NONE',  ( 0.8775825618903724257, 0.000000000000000000, 0.4794255386042036160 ) ) ;
#13570 = CARTESIAN_POINT ( 'NONE',  ( -11.37720190070000115, -49.80573906490000269, -22.46074069029999976 ) ) ;
#13571 = AXIS2_PLACEMENT_3D ( 'NONE', #1704, #25887, #16575 ) ;
#13572 = EDGE_CURVE ( 'NONE', #1013, #17518, #16688, .T. ) ;
#13573 = CARTESIAN_POINT ( 'NONE',  ( 40.70731707320000226, -77.00000000000000000, 7.215414233289999757 ) ) ;
#13574 = CARTESIAN_POINT ( 'NONE',  ( -10.13149969890000079, -18.50000000000000000, 18.43352821810000108 ) ) ;
#13575 = AXIS2_PLACEMENT_3D ( 'NONE', #15313, #2100, #25989 ) ;
#13576 = VECTOR ( 'NONE', #22921, 1000.000000000000000 ) ;
#13577 = EDGE_LOOP ( 'NONE', ( #16992, #3340, #13638, #16698, #3846, #921 ) ) ;
#13578 = CARTESIAN_POINT ( 'NONE',  ( 27.75131065520946905, -92.50000000000000000, 12.65403630604174445 ) ) ;
#13579 = CARTESIAN_POINT ( 'NONE',  ( 27.05591625959999647, -111.0000000000000000, 12.64646362319999895 ) ) ;
#13580 = CARTESIAN_POINT ( 'NONE',  ( 14.78884388380000026, -96.96081173790000207, 14.87954162810000014 ) ) ;
#13581 = ORIENTED_EDGE ( 'NONE', *, *, #25839, .F. ) ;
#13582 = CARTESIAN_POINT ( 'NONE',  ( 23.42046525251764422, -92.54938211474758702, -19.53815701032223728 ) ) ;
#13583 = CARTESIAN_POINT ( 'NONE',  ( 20.51721167730000062, -93.01584738759999027, 16.65400869639999826 ) ) ;
#13584 = B_SPLINE_SURFACE_WITH_KNOTS ( 'NONE', 5, 5, ( 
 ( #6412, #15277, #4231, #13106, #22018, #25826 ),
 ( #10904, #8729, #11502, #9032, #16031, #17938 ),
 ( #22753, #19959, #15882, #24936, #7165, #9324 ),
 ( #22608, #7016, #17791, #9174, #2651, #4965 ),
 ( #629, #18079, #4522, #2351, #20410, #13850 ),
 ( #6721, #18228, #26528, #15432, #13400, #2796 ) ),
 .UNSPECIFIED., .F., .F., .F.,
 ( 6, 6 ),
 ( 6, 6 ),
 ( 21.64530111450000049, 36.61382091400000149 ),
 ( 0.000000000000000000, 0.5000000000000000000 ),
 .UNSPECIFIED. ) ;
#13585 = CARTESIAN_POINT ( 'NONE',  ( 22.55098976337314909, -19.46994031921913049, 0.8437242863546875471 ) ) ;
#13586 = CARTESIAN_POINT ( 'NONE',  ( -7.197000385329999972, -101.3878691800000098, 14.40505143829999923 ) ) ;
#13587 = VERTEX_POINT ( 'NONE', #18353 ) ;
#13588 = CARTESIAN_POINT ( 'NONE',  ( 26.84105869354614526, -72.49728541232093448, -10.88571253161128105 ) ) ;
#13589 = DIRECTION ( 'NONE',  ( 0.000000000000000000, 1.000000000000000000, 0.000000000000000000 ) ) ;
#13590 = CARTESIAN_POINT ( 'NONE',  ( 8.520390455640001193, -37.01762350529999424, -21.57375892880000023 ) ) ;
#13591 = CARTESIAN_POINT ( 'NONE',  ( 45.89652019322726062, -73.81415926414906892, -4.323399998322560833 ) ) ;
#13592 = ORIENTED_EDGE ( 'NONE', *, *, #17008, .T. ) ;
#13593 = CARTESIAN_POINT ( 'NONE',  ( -0.6930209439279999550, -101.1411470200000053, -15.37361599470000151 ) ) ;
#13594 = CIRCLE ( 'NONE', #17315, 3.499999999999999556 ) ;
#13595 = CARTESIAN_POINT ( 'NONE',  ( 9.476764215410000247, -74.50000000000000000, -38.08875739639999836 ) ) ;
#13596 = CARTESIAN_POINT ( 'NONE',  ( 21.49478374063930630, -36.56947960183979518, -7.151043167494730568 ) ) ;
#13597 = CARTESIAN_POINT ( 'NONE',  ( 25.26718046270000073, -18.50000000000000000, 6.129403842640000377 ) ) ;
#13598 = B_SPLINE_CURVE_WITH_KNOTS ( 'NONE', 5,
 ( #2076, #40, #21877, #10915, #19823, #3959 ),
 .UNSPECIFIED., .F., .F.,
 ( 6, 6 ),
 ( 0.000000000000000000, 1.000000000000000000 ),
 .UNSPECIFIED. ) ;
#13599 = ORIENTED_EDGE ( 'NONE', *, *, #5122, .T. ) ;
#13600 = CARTESIAN_POINT ( 'NONE',  ( -21.30003612899999865, -93.00000000000000000, -21.83021898440000186 ) ) ;
#13601 = CARTESIAN_POINT ( 'NONE',  ( 12.74020478277715185, -96.39729796470680867, 17.27646218270080425 ) ) ;
#13602 = DIRECTION ( 'NONE',  ( 0.000000000000000000, 1.000000000000000000, 0.000000000000000000 ) ) ;
#13603 = B_SPLINE_CURVE_WITH_KNOTS ( 'NONE', 5,
 ( #7798, #23383, #7672, #3425, #8204, #6010, #12290, #14889, #21199 ),
 .UNSPECIFIED., .F., .F.,
 ( 6, 3, 6 ),
 ( 0.000000000000000000, 0.5000000000000000000, 1.000000000000000000 ),
 .UNSPECIFIED. ) ;
#13604 = CARTESIAN_POINT ( 'NONE',  ( 25.32712259480000228, -57.40875702469999453, 1.379782074460000230 ) ) ;
#13605 = DIRECTION ( 'NONE',  ( 1.000000000000000000, 0.000000000000000000, 0.000000000000000000 ) ) ;
#13606 = CARTESIAN_POINT ( 'NONE',  ( -36.59277592640000165, -77.00000000000000000, -25.98617420859999783 ) ) ;
#13607 = CARTESIAN_POINT ( 'NONE',  ( 24.76102720923304901, -93.45279863481047755, 11.84977757016969591 ) ) ;
#13608 = ORIENTED_EDGE ( 'NONE', *, *, #19452, .T. ) ;
#13609 = CARTESIAN_POINT ( 'NONE',  ( -29.75227628095127841, -92.87422005961224158, 6.712099127441182311 ) ) ;
#13610 = EDGE_CURVE ( 'NONE', #24058, #10217, #888, .T. ) ;
#13611 = ORIENTED_EDGE ( 'NONE', *, *, #1381, .T. ) ;
#13612 = CARTESIAN_POINT ( 'NONE',  ( -14.87113501819999861, -65.53648121479999133, 22.45123099050000093 ) ) ;
#13613 = CARTESIAN_POINT ( 'NONE',  ( -14.25684790429999893, -62.95263723189999183, 21.84526217519999847 ) ) ;
#13614 = DIRECTION ( 'NONE',  ( 0.000000000000000000, 1.000000000000000000, 0.000000000000000000 ) ) ;
#13615 = VECTOR ( 'NONE', #11721, 1000.000000000000000 ) ;
#13616 = EDGE_CURVE ( 'NONE', #25860, #11169, #9228, .T. ) ;
#13617 = CARTESIAN_POINT ( 'NONE',  ( 20.16453947749999998, -36.00000000000000000, -9.644867042430000481 ) ) ;
#13618 = CIRCLE ( 'NONE', #6637, 30.50381168839999901 ) ;
#13619 = CARTESIAN_POINT ( 'NONE',  ( 14.28941763439999946, -92.50000000000000000, -3.575252188409999921 ) ) ;
#13620 = ADVANCED_FACE ( 'NONE', ( #8385 ), #28213, .T. ) ;
#13621 = CARTESIAN_POINT ( 'NONE',  ( 16.76553128029999939, -99.61736775859999682, 4.445700604479999818 ) ) ;
#13622 = ORIENTED_EDGE ( 'NONE', *, *, #28400, .T. ) ;
#13623 = B_SPLINE_CURVE_WITH_KNOTS ( 'NONE', 3,
 ( #15883, #20411, #25506, #12635, #7872, #25790 ),
 .UNSPECIFIED., .F., .F.,
 ( 4, 2, 4 ),
 ( 0.000000000000000000, 0.5000000000000000000, 1.000000000000000000 ),
 .UNSPECIFIED. ) ;
#13624 = CARTESIAN_POINT ( 'NONE',  ( -7.215414233289999757, -74.50000000000000000, -40.70731707320000226 ) ) ;
#13625 = CARTESIAN_POINT ( 'NONE',  ( 28.91153913726728675, -74.37196457031747343, -26.52194363930463794 ) ) ;
#13626 = CARTESIAN_POINT ( 'NONE',  ( -17.86977837739999941, -98.51736893809999174, -8.245718314579999486 ) ) ;
#13627 = ORIENTED_EDGE ( 'NONE', *, *, #27357, .F. ) ;
#13628 = CARTESIAN_POINT ( 'NONE',  ( 23.07334373890000023, -54.17834560379999687, 10.34261593159999926 ) ) ;
#13629 = VERTEX_POINT ( 'NONE', #10283 ) ;
#13630 = CARTESIAN_POINT ( 'NONE',  ( 12.03978574509999966, -15.50000000000000000, 22.03867997850000293 ) ) ;
#13631 = VECTOR ( 'NONE', #5560, 1000.000000000000000 ) ;
#13632 = DIRECTION ( 'NONE',  ( 0.000000000000000000, -1.000000000000000000, 0.000000000000000000 ) ) ;
#13633 = DIRECTION ( 'NONE',  ( -0.000000000000000000, 1.000000000000000000, 0.000000000000000000 ) ) ;
#13634 = CARTESIAN_POINT ( 'NONE',  ( -40.50000000000000000, -11.00000000000000000, -4.500000000000000000 ) ) ;
#13635 = CARTESIAN_POINT ( 'NONE',  ( 22.15526589779999966, -65.02054951249999704, 11.85001090629999965 ) ) ;
#13636 = CARTESIAN_POINT ( 'NONE',  ( -41.59490899353561133, -65.09473114940422533, 2.889727902555501160 ) ) ;
#13637 = CARTESIAN_POINT ( 'NONE',  ( -17.53021419299614081, -96.09436528054369830, 13.05496988638304146 ) ) ;
#13638 = ORIENTED_EDGE ( 'NONE', *, *, #20675, .F. ) ;
#13639 = CARTESIAN_POINT ( 'NONE',  ( -12.78246122589999878, -70.56976055389999658, -24.52593635099999858 ) ) ;
#13640 = CARTESIAN_POINT ( 'NONE',  ( -3.132411190821024149, -98.07566646228944762, 20.23086237361857442 ) ) ;
#13641 = CARTESIAN_POINT ( 'NONE',  ( -12.87349974830000043, -99.74726900420000675, -11.33951603419999898 ) ) ;
#13642 = CIRCLE ( 'NONE', #1124, 1.000000000000000888 ) ;
#13643 = DIRECTION ( 'NONE',  ( 0.000000000000000000, 1.000000000000000000, 0.000000000000000000 ) ) ;
#13644 = CARTESIAN_POINT ( 'NONE',  ( 23.81686956487109086, -64.79566076651281037, -7.674173441228443693 ) ) ;
#13645 = ORIENTED_EDGE ( 'NONE', *, *, #23898, .F. ) ;
#13646 = CARTESIAN_POINT ( 'NONE',  ( 26.66370566908554096, -92.65976904079786891, -14.80868499793449722 ) ) ;
#13647 = EDGE_LOOP ( 'NONE', ( #4185, #3549, #13353, #19820 ) ) ;
#13648 = EDGE_CURVE ( 'NONE', #26062, #19169, #23317, .T. ) ;
#13649 = CARTESIAN_POINT ( 'NONE',  ( 3.355978770230000130, -90.50000000000000000, 6.143077933229999843 ) ) ;
#13650 = CIRCLE ( 'NONE', #1137, 2.500000000000000444 ) ;
#13651 = CARTESIAN_POINT ( 'NONE',  ( 6.962669195700001090, -93.00000450890000536, -28.64060852350000275 ) ) ;
#13652 = EDGE_CURVE ( 'NONE', #14525, #17829, #1337, .T. ) ;
#13653 = CARTESIAN_POINT ( 'NONE',  ( -0.5784133371710000748, -95.70830610519999482, 22.47961678780000128 ) ) ;
#13654 = CARTESIAN_POINT ( 'NONE',  ( 11.26661192880000151, -92.54721911629999909, 27.31814187710000041 ) ) ;
#13655 = EDGE_CURVE ( 'NONE', #8384, #3189, #21328, .T. ) ;
#13656 = ORIENTED_EDGE ( 'NONE', *, *, #24509, .T. ) ;
#13657 = B_SPLINE_CURVE_WITH_KNOTS ( 'NONE', 5,
 ( #5427, #23207, #650, #27294, #18405, #7331 ),
 .UNSPECIFIED., .F., .F.,
 ( 6, 6 ),
 ( 0.000000000000000000, 1.000000000000000000 ),
 .UNSPECIFIED. ) ;
#13658 = DIRECTION ( 'NONE',  ( 0.000000000000000000, 1.000000000000000000, 0.000000000000000000 ) ) ;
#13659 = VERTEX_POINT ( 'NONE', #25895 ) ;
#13660 = CARTESIAN_POINT ( 'NONE',  ( -22.62019343126265625, -69.58561462934873987, 15.11541909148706075 ) ) ;
#13661 = CARTESIAN_POINT ( 'NONE',  ( 20.37436807119999926, -94.16701182180001695, 13.61303751910000059 ) ) ;
#13662 = CARTESIAN_POINT ( 'NONE',  ( 47.17354595309999610, -74.60192833800000756, -1.119582300150000043 ) ) ;
#13663 = EDGE_LOOP ( 'NONE', ( #9306, #6075, #9592, #22971, #5901, #21069, #10140, #13990, #18267, #12977, #23292, #21280, #4667, #5183, #13323, #366 ) ) ;
#13664 = AXIS2_PLACEMENT_3D ( 'NONE', #8460, #28428, #6423 ) ;
#13665 = CARTESIAN_POINT ( 'NONE',  ( -10.05832918090000128, -74.00000000000000000, 34.34024345419999946 ) ) ;
#13666 = CARTESIAN_POINT ( 'NONE',  ( -22.71848792900000191, -80.00000000000000000, -32.61798286559999838 ) ) ;
#13667 = CARTESIAN_POINT ( 'NONE',  ( 12.41906884210000150, -101.3138676899999950, -9.951096275919999457 ) ) ;
#13668 = CARTESIAN_POINT ( 'NONE',  ( -13.31557542770000069, -94.15497152580000773, -21.58932584709999958 ) ) ;
#13669 = DIRECTION ( 'NONE',  ( 1.000000000000000000, 0.000000000000000000, 0.000000000000000000 ) ) ;
#13670 = ORIENTED_EDGE ( 'NONE', *, *, #5733, .F. ) ;
#13671 = CARTESIAN_POINT ( 'NONE',  ( -41.91080743279999865, -63.35440207070000440, -1.043878858150000033 ) ) ;
#13672 = CARTESIAN_POINT ( 'NONE',  ( -16.77203540500000045, -99.85754733859999988, 2.755720534169999958 ) ) ;
#13673 = CARTESIAN_POINT ( 'NONE',  ( -39.12193274490000050, -73.75841684550000821, 7.250133233359999707 ) ) ;
#13674 = CARTESIAN_POINT ( 'NONE',  ( -22.01433816329999971, -74.00000000000000000, -32.02416862469999614 ) ) ;
#13675 = CARTESIAN_POINT ( 'NONE',  ( 0.000000000000000000, -28.10000000000000142, 0.000000000000000000 ) ) ;
#13676 = DIRECTION ( 'NONE',  ( 1.000000000000000000, 0.000000000000000000, 0.000000000000000000 ) ) ;
#13677 = CARTESIAN_POINT ( 'NONE',  ( -7.485351522714842609, -73.99989166819224806, 38.96151920400748025 ) ) ;
#13678 = CARTESIAN_POINT ( 'NONE',  ( 21.42681242760168914, -35.72549454987603212, -7.289241608393363769 ) ) ;
#13679 = ORIENTED_EDGE ( 'NONE', *, *, #5241, .T. ) ;
#13680 = CARTESIAN_POINT ( 'NONE',  ( 0.000000000000000000, -86.00000000000000000, 0.000000000000000000 ) ) ;
#13681 = DIRECTION ( 'NONE',  ( 0.4151946956541399669, 0.5000000000001689759, 0.7600087925152558821 ) ) ;
#13682 = CARTESIAN_POINT ( 'NONE',  ( 8.113043114279999912, -34.60505749659999708, -21.05852214609999962 ) ) ;
#13683 = CARTESIAN_POINT ( 'NONE',  ( 16.26822356142537629, -100.5798851022435940, 4.341841719661410970 ) ) ;
#13684 = EDGE_CURVE ( 'NONE', #14853, #18925, #12458, .T. ) ;
#13685 = CARTESIAN_POINT ( 'NONE',  ( -11.07305194678827043, -18.50000000000000000, -24.81486620154639411 ) ) ;
#13686 = ORIENTED_EDGE ( 'NONE', *, *, #19776, .T. ) ;
#13687 = CARTESIAN_POINT ( 'NONE',  ( 21.50956136780000350, -52.61368720120000120, 10.11639787090000020 ) ) ;
#13688 = VECTOR ( 'NONE', #23125, 999.9999999999998863 ) ;
#13689 = CARTESIAN_POINT ( 'NONE',  ( -14.63416202187712933, -101.1297513861017450, 4.643748334617020745 ) ) ;
#13690 = EDGE_CURVE ( 'NONE', #16909, #12644, #8301, .T. ) ;
#13691 = CARTESIAN_POINT ( 'NONE',  ( -12.66643311790000048, -65.04696659260000047, -21.71432957020000032 ) ) ;
#13692 = CARTESIAN_POINT ( 'NONE',  ( 25.02058483049999538, -57.41946977210000114, 1.375913446200000001 ) ) ;
#13693 = DIRECTION ( 'NONE',  ( 0.000000000000000000, 1.000000000000000000, 0.000000000000000000 ) ) ;
#13694 = CARTESIAN_POINT ( 'NONE',  ( 12.80450217360000131, -93.00000000000000000, 27.55316291459999789 ) ) ;
#13695 = VERTEX_POINT ( 'NONE', #12339 ) ;
#13696 = DIRECTION ( 'NONE',  ( 0.000000000000000000, -1.000000000000000000, 0.000000000000000000 ) ) ;
#13697 = CARTESIAN_POINT ( 'NONE',  ( 46.76737938683341156, -73.86778755184377587, -2.601362616105526993 ) ) ;
#13698 = ORIENTED_EDGE ( 'NONE', *, *, #21796, .T. ) ;
#13699 = AXIS2_PLACEMENT_3D ( 'NONE', #9252, #25000, #4599 ) ;
#13700 = CARTESIAN_POINT ( 'NONE',  ( -11.18242929300000021, -57.47855601759999900, 20.51090108450000216 ) ) ;
#13701 = DIRECTION ( 'NONE',  ( 0.000000000000000000, -1.000000000000000000, 0.000000000000000000 ) ) ;
#13702 = ORIENTED_EDGE ( 'NONE', *, *, #27873, .T. ) ;
#13703 = CARTESIAN_POINT ( 'NONE',  ( 16.42966247209999864, -94.59276292389999696, 17.21499781270000184 ) ) ;
#13704 = CARTESIAN_POINT ( 'NONE',  ( 3.432129155885089489, -93.09721478922745064, -28.80740708133247452 ) ) ;
#13705 = CARTESIAN_POINT ( 'NONE',  ( -41.00000000000000000, -84.00000000000000000, -10.20110288159999890 ) ) ;
#13706 = CARTESIAN_POINT ( 'NONE',  ( 26.50442268124868050, -71.53529804145092896, -9.316922704210117701 ) ) ;
#13707 = AXIS2_PLACEMENT_3D ( 'NONE', #15932, #9224, #22514 ) ;
#13708 = LINE ( 'NONE', #9477, #24634 ) ;
#13709 = FACE_OUTER_BOUND ( 'NONE', #25502, .T. ) ;
#13710 = ORIENTED_EDGE ( 'NONE', *, *, #20397, .F. ) ;
#13711 = CARTESIAN_POINT ( 'NONE',  ( 10.18254802899999945, -92.87437365140000622, -25.45365413509999897 ) ) ;
#13712 = CARTESIAN_POINT ( 'NONE',  ( -38.16136311219324284, -65.74402559148357739, -1.166215138813985419 ) ) ;
#13713 = CARTESIAN_POINT ( 'NONE',  ( -12.28514971879595663, -92.50630337894784816, 27.91669684123871775 ) ) ;
#13714 = ORIENTED_EDGE ( 'NONE', *, *, #12030, .F. ) ;
#13715 = VECTOR ( 'NONE', #13204, 1000.000000000000000 ) ;
#13716 = CARTESIAN_POINT ( 'NONE',  ( 0.000000000000000000, -36.20000000000000284, 0.000000000000000000 ) ) ;
#13717 = DIRECTION ( 'NONE',  ( 0.000000000000000000, 1.000000000000000000, 0.000000000000000000 ) ) ;
#13718 = CARTESIAN_POINT ( 'NONE',  ( -21.43329341219999762, -64.24504445130001784, 15.59675287610000005 ) ) ;
#13719 = EDGE_LOOP ( 'NONE', ( #27937, #3631, #14736, #3569 ) ) ;
#13720 = CARTESIAN_POINT ( 'NONE',  ( -17.69156363009999922, -96.95584349610000174, 11.12533346610000073 ) ) ;
#13721 = CIRCLE ( 'NONE', #28150, 0.7500000000000006661 ) ;
#13722 = CARTESIAN_POINT ( 'NONE',  ( -18.72487404859999671, -26.08233090750000116, 13.26742744989999956 ) ) ;
#13723 = CARTESIAN_POINT ( 'NONE',  ( 27.03609113194391256, -74.42256117523155012, -28.47179119120458424 ) ) ;
#13724 = CARTESIAN_POINT ( 'NONE',  ( 32.34203265880000089, -73.93832878009999376, -20.34158615750000010 ) ) ;
#13725 = CARTESIAN_POINT ( 'NONE',  ( -14.76920872520722128, -74.23817965565569921, 36.28536762717221364 ) ) ;
#13726 = ADVANCED_FACE ( 'NONE', ( #27804 ), #17144, .F. ) ;
#13727 = DIRECTION ( 'NONE',  ( 0.000000000000000000, 1.000000000000000000, 0.000000000000000000 ) ) ;
#13728 = EDGE_CURVE ( 'NONE', #5438, #20928, #10604, .T. ) ;
#13729 = ORIENTED_EDGE ( 'NONE', *, *, #806, .T. ) ;
#13730 = CARTESIAN_POINT ( 'NONE',  ( -39.06010443616429484, -73.53996501803551666, -7.188997797805019907 ) ) ;
#13731 = DIRECTION ( 'NONE',  ( 1.000000000000000000, 0.000000000000000000, 0.000000000000000000 ) ) ;
#13732 = AXIS2_PLACEMENT_3D ( 'NONE', #9924, #14310, #3256 ) ;
#13733 = B_SPLINE_CURVE_WITH_KNOTS ( 'NONE', 3,
 ( #5631, #14095, #9571, #5491, #3451, #1280 ),
 .UNSPECIFIED., .F., .F.,
 ( 4, 2, 4 ),
 ( 0.000000000000000000, 0.5000000000000000000, 1.000000000000000000 ),
 .UNSPECIFIED. ) ;
#13734 = DIRECTION ( 'NONE',  ( 0.000000000000000000, 1.000000000000000000, 0.000000000000000000 ) ) ;
#13735 = ORIENTED_EDGE ( 'NONE', *, *, #15543, .T. ) ;
#13736 = CARTESIAN_POINT ( 'NONE',  ( 23.76344434241608283, -92.71346081468576017, -19.11932852845460573 ) ) ;
#13737 = CARTESIAN_POINT ( 'NONE',  ( 22.54710945800000133, -93.01085527750001347, 15.53951536520000154 ) ) ;
#13738 = CARTESIAN_POINT ( 'NONE',  ( 23.17742085089960113, -19.47933631450631253, 1.304785058156784361 ) ) ;
#13739 = CARTESIAN_POINT ( 'NONE',  ( -7.338479256380000315, -100.8772072149999985, 13.99320739510000067 ) ) ;
#13740 = CARTESIAN_POINT ( 'NONE',  ( 26.85156072424344131, -72.47607639700331106, -10.93820933281734042 ) ) ;
#13741 = CARTESIAN_POINT ( 'NONE',  ( -12.48888858376851907, -101.5829753080983977, -10.08195492097721058 ) ) ;
#13742 = CARTESIAN_POINT ( 'NONE',  ( 7.971459325760000603, -37.27103823680000261, -21.55676125340000127 ) ) ;
#13743 = CARTESIAN_POINT ( 'NONE',  ( 8.594185256147103047, -19.47869450728761720, -20.00856785065116838 ) ) ;
#13744 = ORIENTED_EDGE ( 'NONE', *, *, #22310, .T. ) ;
#13745 = CARTESIAN_POINT ( 'NONE',  ( 7.437117725900000309, -99.39747163819998832, 16.00091516599999864 ) ) ;
#13746 = ADVANCED_FACE ( 'NONE', ( #10549 ), #18577, .F. ) ;
#13747 = CARTESIAN_POINT ( 'NONE',  ( 24.39713797690000163, -19.18584095090000119, 1.459766401380000023 ) ) ;
#13748 = FACE_OUTER_BOUND ( 'NONE', #19962, .T. ) ;
#13749 = CARTESIAN_POINT ( 'NONE',  ( -2.135291575822543475, -19.47314420526490863, -22.69925340028805039 ) ) ;
#13750 = CARTESIAN_POINT ( 'NONE',  ( 11.63343413870000020, -100.9405348700000076, -10.90407401050000047 ) ) ;
#13751 = CARTESIAN_POINT ( 'NONE',  ( -0.8452062098759999254, -52.63280639819999607, -23.17863372589999926 ) ) ;
#13752 = DIRECTION ( 'NONE',  ( 0.000000000000000000, 1.000000000000000000, 0.000000000000000000 ) ) ;
#13753 = CARTESIAN_POINT ( 'NONE',  ( -38.25000000000000000, -63.07912966450000880, -2.684678751729999480 ) ) ;
#13754 = B_SPLINE_CURVE_WITH_KNOTS ( 'NONE', 3,
 ( #15931, #378, #11100, #24835, #2402, #8783, #26581, #24691, #9222, #24251, #20013, #20166, #13604 ),
 .UNSPECIFIED., .F., .F.,
 ( 4, 2, 2, 1, 2, 2, 4 ),
 ( 0.000000000000000000, 0.2499999999999875655, 0.3749999999999815703, 0.4374999999999798495, 0.4687499999999790168, 0.4999999999999781286, 1.000000000000000000 ),
 .UNSPECIFIED. ) ;
#13755 = DIRECTION ( 'NONE',  ( 0.8775825618903723147, 0.000000000000000000, 0.4794255386042037825 ) ) ;
#13756 = CARTESIAN_POINT ( 'NONE',  ( 37.60355029590000697, -84.50000000000000000, -9.356041104380000917 ) ) ;
#13757 = CARTESIAN_POINT ( 'NONE',  ( 6.867289776849999861, -93.00000000000000000, 29.52484619129999643 ) ) ;
#13758 = CYLINDRICAL_SURFACE ( 'NONE', #12238, 16.00000000000000000 ) ;
#13759 = ORIENTED_EDGE ( 'NONE', *, *, #8307, .F. ) ;
#13760 = LINE ( 'NONE', #15789, #24146 ) ;
#13761 = EDGE_CURVE ( 'NONE', #23006, #19757, #20414, .T. ) ;
#13762 = CARTESIAN_POINT ( 'NONE',  ( -14.55867152370000106, -64.24504444460001196, 22.15151623919999935 ) ) ;
#13763 = CARTESIAN_POINT ( 'NONE',  ( -13.44405735660000012, -68.28990366489999531, 22.97003097380000014 ) ) ;
#13764 = FACE_OUTER_BOUND ( 'NONE', #15150, .T. ) ;
#13765 = CARTESIAN_POINT ( 'NONE',  ( -18.75664408842720121, -92.68584073461859418, 22.80736226812994261 ) ) ;
#13766 = CARTESIAN_POINT ( 'NONE',  ( 21.02256860540000005, -93.91547409650000588, 13.07290323880000038 ) ) ;
#13767 = CARTESIAN_POINT ( 'NONE',  ( -3.666223272120000027E-16, -84.50000000000000000, -40.00000000000000000 ) ) ;
#13768 = CARTESIAN_POINT ( 'NONE',  ( -11.25973246350476487, -41.21911678045049854, -22.28515149975225285 ) ) ;
#13769 = ORIENTED_EDGE ( 'NONE', *, *, #27863, .T. ) ;
#13770 = DIRECTION ( 'NONE',  ( 1.000000000000000000, 0.000000000000000000, 0.000000000000000000 ) ) ;
#13771 = CARTESIAN_POINT ( 'NONE',  ( -15.33123009060000008, -99.55619081909999579, -8.401006626490000073 ) ) ;
#13772 = ORIENTED_EDGE ( 'NONE', *, *, #7257, .F. ) ;
#13773 = CARTESIAN_POINT ( 'NONE',  ( 9.134356845928596869, -92.82529299096876230, 29.10006078398899021 ) ) ;
#13774 = ORIENTED_EDGE ( 'NONE', *, *, #17596, .F. ) ;
#13775 = DIRECTION ( 'NONE',  ( 1.000000000000000000, 0.000000000000000000, 0.000000000000000000 ) ) ;
#13776 = EDGE_CURVE ( 'NONE', #22228, #18774, #16346, .T. ) ;
#13777 = CARTESIAN_POINT ( 'NONE',  ( -38.25000000001283951, -63.32273534313050334, 1.487446372692276864 ) ) ;
#13778 = DIRECTION ( 'NONE',  ( 1.000000000000000000, 0.000000000000000000, 0.000000000000000000 ) ) ;
#13779 = CARTESIAN_POINT ( 'NONE',  ( -7.248542667678731455, -73.88534697526095840, -39.85457864233587344 ) ) ;
#13780 = CARTESIAN_POINT ( 'NONE',  ( 20.05190523629999788, -18.61827554290000108, 9.243272875029999724 ) ) ;
#13781 = CARTESIAN_POINT ( 'NONE',  ( -20.91226881559999740, -64.69849613010001121, 14.77252284299999907 ) ) ;
#13782 = CARTESIAN_POINT ( 'NONE',  ( 13.81099964959999937, -99.92967428129999519, -10.51862844640000105 ) ) ;
#13783 = ORIENTED_EDGE ( 'NONE', *, *, #2237, .F. ) ;
#13784 = CARTESIAN_POINT ( 'NONE',  ( -12.17507554820000060, -71.31774462289999406, -25.53716782429999910 ) ) ;
#13785 = CARTESIAN_POINT ( 'NONE',  ( -3.463941484895344480, -98.37417905842463028, 19.78189371439013300 ) ) ;
#13786 = CARTESIAN_POINT ( 'NONE',  ( 7.724131721144110507, -101.6290295230935499, 14.02868979977465358 ) ) ;
#13787 = ADVANCED_FACE ( 'NONE', ( #6060 ), #23989, .F. ) ;
#13788 = CARTESIAN_POINT ( 'NONE',  ( 20.16789755236859705, -19.46756325250261455, 9.702623992525639451 ) ) ;
#13789 = CARTESIAN_POINT ( 'NONE',  ( -38.65569830309999588, -74.00000023179998720, -7.472969336320000266 ) ) ;
#13790 = ORIENTED_EDGE ( 'NONE', *, *, #10305, .F. ) ;
#13791 = CARTESIAN_POINT ( 'NONE',  ( 26.82487458483781850, -92.59033770622828285, -14.51536147898519857 ) ) ;
#13792 = EDGE_LOOP ( 'NONE', ( #12961, #6528, #2494, #2122 ) ) ;
#13793 = CARTESIAN_POINT ( 'NONE',  ( 28.07036528529999941, -39.50000000000000000, 51.38245899869999533 ) ) ;
#13794 = DIRECTION ( 'NONE',  ( -0.7529607911047507818, 0.000000000000000000, 0.6580653820547832655 ) ) ;
#13795 = AXIS2_PLACEMENT_3D ( 'NONE', #7627, #6252, #12513 ) ;
#13796 = CARTESIAN_POINT ( 'NONE',  ( 11.27094287870000144, -92.51078253369999516, 27.07599673740000057 ) ) ;
#13797 = ORIENTED_EDGE ( 'NONE', *, *, #22100, .F. ) ;
#13798 = CARTESIAN_POINT ( 'NONE',  ( -19.88709748648987485, -26.11257320932467252, 14.48079129993961978 ) ) ;
#13799 = ORIENTED_EDGE ( 'NONE', *, *, #14850, .T. ) ;
#13800 = CARTESIAN_POINT ( 'NONE',  ( -22.67424940895870478, -69.82955780735299811, 15.23442037431579976 ) ) ;
#13801 = CARTESIAN_POINT ( 'NONE',  ( -17.85148316769999965, -92.81180222680001179, -20.73234325470000172 ) ) ;
#13802 = CARTESIAN_POINT ( 'NONE',  ( 46.87568470190000625, -74.15546349729999065, -2.521714412790000193 ) ) ;
#13803 = VERTEX_POINT ( 'NONE', #15081 ) ;
#13804 = CARTESIAN_POINT ( 'NONE',  ( 7.217717631489795060, -73.61799623139430082, -39.31656870534071402 ) ) ;
#13805 = CARTESIAN_POINT ( 'NONE',  ( -11.32307664120000013, -101.1889999979999999, 9.421136869679999748 ) ) ;
#13806 = ORIENTED_EDGE ( 'NONE', *, *, #16851, .F. ) ;
#13807 = CARTESIAN_POINT ( 'NONE',  ( 7.412091288878791318, -101.1586403914945151, 13.76842333336193924 ) ) ;
#13808 = CARTESIAN_POINT ( 'NONE',  ( -2.555683107399999709, -71.82672919469999329, -28.11473569369999836 ) ) ;
#13809 = EDGE_CURVE ( 'NONE', #11515, #11754, #8535, .T. ) ;
#13810 = CARTESIAN_POINT ( 'NONE',  ( -11.71096586250000016, -94.52293239719999463, -20.87032883819999896 ) ) ;
#13811 = FACE_OUTER_BOUND ( 'NONE', #8984, .T. ) ;
#13812 = ORIENTED_EDGE ( 'NONE', *, *, #15649, .F. ) ;
#13813 = ADVANCED_FACE ( 'NONE', ( #20201 ), #4167, .F. ) ;
#13814 = CARTESIAN_POINT ( 'NONE',  ( -10.50000000000000000, -89.50000000000000000, 4.573100142190000219E-16 ) ) ;
#13815 = CARTESIAN_POINT ( 'NONE',  ( 13.77380425289999977, -99.99711545080000974, -10.25584394120000020 ) ) ;
#13816 = CARTESIAN_POINT ( 'NONE',  ( -22.14868796429999875, -74.09723562380000317, -32.50232833649999975 ) ) ;
#13817 = EDGE_LOOP ( 'NONE', ( #17715, #1285, #6090, #570 ) ) ;
#13818 = DIRECTION ( 'NONE',  ( 0.000000000000000000, -1.000000000000000000, 0.000000000000000000 ) ) ;
#13819 = EDGE_CURVE ( 'NONE', #8764, #22228, #19753, .T. ) ;
#13820 = CARTESIAN_POINT ( 'NONE',  ( 0.8834120860809999698, -100.8023006570000035, -15.75170354469999978 ) ) ;
#13821 = CARTESIAN_POINT ( 'NONE',  ( -18.51733628490000072, -18.50000000000000000, 14.45311368080000136 ) ) ;
#13822 = ORIENTED_EDGE ( 'NONE', *, *, #16045, .F. ) ;
#13823 = EDGE_CURVE ( 'NONE', #8389, #22342, #28322, .T. ) ;
#13824 = CARTESIAN_POINT ( 'NONE',  ( -11.84764024939999949, -93.03217248389999838, -23.86222728849999797 ) ) ;
#13825 = CARTESIAN_POINT ( 'NONE',  ( 23.56065605869999757, -94.89197151660000884, -2.367189373290000010 ) ) ;
#13826 = CARTESIAN_POINT ( 'NONE',  ( 8.079305843170001111, -34.74137583460000656, -21.08830559229999935 ) ) ;
#13827 = CARTESIAN_POINT ( 'NONE',  ( 15.82012184412321787, -101.2111896145381280, 4.085987896871170477 ) ) ;
#13828 = PLANE ( 'NONE',  #9498 ) ;
#13829 = VERTEX_POINT ( 'NONE', #19614 ) ;
#13830 = CARTESIAN_POINT ( 'NONE',  ( 47.11061145800000105, -79.77209722760001398, -1.777386438419999992 ) ) ;
#13831 = CARTESIAN_POINT ( 'NONE',  ( -14.64568814080000081, -101.2530993010000060, 4.044604232330000215 ) ) ;
#13832 = B_SPLINE_SURFACE_WITH_KNOTS ( 'NONE', 5, 5, ( 
 ( #20669, #25334, #20811, #15984, #11604, #25029, #873, #22855, #8077 ),
 ( #18625, #2898, #728, #27520, #5879, #7567, #5363, #14247, #20959 ),
 ( #26163, #24109, #6188, #24259, #8515, #21930, #4295, #8362, #12589 ),
 ( #1692, #17417, #21780, #22079, #10674, #8227, #6033, #14919, #10960 ),
 ( #19869, #28619, #6478, #10530, #17701, #19446, #26592, #15058, #21500 ),
 ( #1979, #17121, #10397, #4144, #19590, #12862, #28475, #19316, #13169 ) ),
 .UNSPECIFIED., .F., .F., .F.,
 ( 6, 6 ),
 ( 6, 3, 6 ),
 ( 4.007746616509999527, 6.717368912360000444 ),
 ( 0.000000000000000000, 1.000000000000000000, 2.000000000000000000 ),
 .UNSPECIFIED. ) ;
#13833 = CONTEXT_DEPENDENT_SHAPE_REPRESENTATION ( #26344, #13395 ) ;
#13834 = CARTESIAN_POINT ( 'NONE',  ( -11.04119194200000109, -18.61783138060000198, 18.70101294130000014 ) ) ;
#13835 = CARTESIAN_POINT ( 'NONE',  ( -11.81703488210000152, -60.57882006589999691, -20.52627317210000157 ) ) ;
#13836 = CARTESIAN_POINT ( 'NONE',  ( 25.63123037620000133, -69.68000722649999545, -9.264901491119999832 ) ) ;
#13837 = CARTESIAN_POINT ( 'NONE',  ( 0.000000000000000000, -2.000000000000000000, 0.000000000000000000 ) ) ;
#13838 = AXIS2_PLACEMENT_3D ( 'NONE', #22130, #20371, #9140 ) ;
#13839 = VERTEX_POINT ( 'NONE', #22395 ) ;
#13840 = CARTESIAN_POINT ( 'NONE',  ( -41.75000000000000000, -65.41419836839999391, -2.121055962339999823 ) ) ;
#13841 = ORIENTED_EDGE ( 'NONE', *, *, #5286, .T. ) ;
#13842 = CARTESIAN_POINT ( 'NONE',  ( 30.97576656850000276, -72.00000000000000000, -19.97576656849999921 ) ) ;
#13843 = CARTESIAN_POINT ( 'NONE',  ( -21.60034937969999902, -74.39508596250000494, -32.77174707999999725 ) ) ;
#13844 = EDGE_LOOP ( 'NONE', ( #14491, #27807, #16581, #19392 ) ) ;
#13845 = AXIS2_PLACEMENT_3D ( 'NONE', #22284, #15563, #11022 ) ;
#13846 = CARTESIAN_POINT ( 'NONE',  ( -2.581268101460000075, -55.47051022630000006, -25.18513566209999865 ) ) ;
#13847 = CONICAL_SURFACE ( 'NONE', #2696, 55.67692378859999280, 1.047197551199999799 ) ;
#13848 = CARTESIAN_POINT ( 'NONE',  ( 8.373915991510450851, -94.27895761501838479, -24.15545878555541748 ) ) ;
#13849 = CARTESIAN_POINT ( 'NONE',  ( 9.341186407280000196E-15, -73.50000000000000000, 32.75000000000000000 ) ) ;
#13850 = CARTESIAN_POINT ( 'NONE',  ( -18.00122845199999944, -98.93440624740000544, 5.015517834929999808 ) ) ;
#13851 = CARTESIAN_POINT ( 'NONE',  ( -41.37299426109999700, -65.19264941160000149, -2.813424548380000001 ) ) ;
#13852 = DIRECTION ( 'NONE',  ( 0.2414462220490760924, 0.000000000000000000, 0.9704142011833030157 ) ) ;
#13853 = EDGE_LOOP ( 'NONE', ( #28248, #4188, #1393, #11178 ) ) ;
#13854 = ADVANCED_FACE ( 'NONE', ( #15366 ), #27853, .T. ) ;
#13855 = DIRECTION ( 'NONE',  ( 0.000000000000000000, 1.000000000000000000, 0.000000000000000000 ) ) ;
#13856 = CARTESIAN_POINT ( 'NONE',  ( -37.89028998459014019, -65.69483747913999139, -0.8156460645458384340 ) ) ;
#13857 = CARTESIAN_POINT ( 'NONE',  ( -32.75442352089999787, -74.37394555080000202, -21.60834384349999837 ) ) ;
#13858 = EDGE_LOOP ( 'NONE', ( #2303, #16872, #28784, #17131 ) ) ;
#13859 = CARTESIAN_POINT ( 'NONE',  ( -38.07292563641772887, -63.35495820213566986, -1.012765098742579362 ) ) ;
#13860 = CARTESIAN_POINT ( 'NONE',  ( 7.627568735119999666, -74.00000000000000000, 38.62788659690000515 ) ) ;
#13861 = CARTESIAN_POINT ( 'NONE',  ( -22.07768936720000141, -67.34374581909999335, 16.43776412940000142 ) ) ;
#13862 = EDGE_LOOP ( 'NONE', ( #9121, #14163, #8259, #7645 ) ) ;
#13863 = EDGE_CURVE ( 'NONE', #14760, #25977, #22279, .T. ) ;
#13864 = TOROIDAL_SURFACE ( 'NONE', #12001, 24.50000000000000000, 3.000000000000000000 ) ;
#13865 = CARTESIAN_POINT ( 'NONE',  ( -17.50501298330000211, -97.01468531680001206, 11.19299372800000114 ) ) ;
#13866 = CARTESIAN_POINT ( 'NONE',  ( -18.82092041760000001, -26.09894693429999890, 11.90111641600000070 ) ) ;
#13867 = DIRECTION ( 'NONE',  ( 0.4692400087391608854, 0.000000000000000000, -0.8830706733883039172 ) ) ;
#13868 = CARTESIAN_POINT ( 'NONE',  ( -20.56018235820000228, -57.40875686090000585, 14.85415984670000000 ) ) ;
#13869 = CARTESIAN_POINT ( 'NONE',  ( 22.22481399220000142, -59.04179743959999627, -7.379008407440000639 ) ) ;
#13870 = CARTESIAN_POINT ( 'NONE',  ( 26.64666883629999816, -68.06111992670000177, 1.045296570979999951 ) ) ;
#13871 = AXIS2_PLACEMENT_3D ( 'NONE', #17813, #26703, #28711 ) ;
#13872 = CARTESIAN_POINT ( 'NONE',  ( 26.77683864449999973, -26.59999999999999787, 49.01467436490000296 ) ) ;
#13873 = ORIENTED_EDGE ( 'NONE', *, *, #3727, .F. ) ;
#13874 = DIRECTION ( 'NONE',  ( 0.000000000000000000, -1.000000000000000000, 0.000000000000000000 ) ) ;
#13875 = CARTESIAN_POINT ( 'NONE',  ( 12.41281216700000023, -98.24303092559999584, 14.67252853509999966 ) ) ;
#13876 = ORIENTED_EDGE ( 'NONE', *, *, #10145, .T. ) ;
#13877 = CARTESIAN_POINT ( 'NONE',  ( 23.00372540730000281, -92.50000000000000000, -20.02694728079999820 ) ) ;
#13878 = FACE_OUTER_BOUND ( 'NONE', #6262, .T. ) ;
#13879 = AXIS2_PLACEMENT_3D ( 'NONE', #1038, #20688, #23293 ) ;
#13880 = CARTESIAN_POINT ( 'NONE',  ( -24.52910776410000082, -80.00000000000000000, -34.42860270069999729 ) ) ;
#13881 = CARTESIAN_POINT ( 'NONE',  ( -7.374356127060000432, -100.8685038539999965, 13.89626452919999977 ) ) ;
#13882 = AXIS2_PLACEMENT_3D ( 'NONE', #4644, #11329, #13520 ) ;
#13883 = CARTESIAN_POINT ( 'NONE',  ( 3.976803427850000183, -92.99999854809999533, 28.21756021889999744 ) ) ;
#13884 = DIRECTION ( 'NONE',  ( 0.000000000000000000, 0.000000000000000000, 1.000000000000000000 ) ) ;
#13885 =( REPRESENTATION_RELATIONSHIP ('NONE','NONE', #26008, #10734 ) REPRESENTATION_RELATIONSHIP_WITH_TRANSFORMATION ( #20700 )SHAPE_REPRESENTATION_RELATIONSHIP( ) );
#13886 = CARTESIAN_POINT ( 'NONE',  ( 9.334885652660000588, -35.98248194970000213, -19.73601135230000025 ) ) ;
#13887 = CARTESIAN_POINT ( 'NONE',  ( 7.629218925470000023, -101.5342894280000081, 14.06592359269999903 ) ) ;
#13888 = ORIENTED_EDGE ( 'NONE', *, *, #17777, .F. ) ;
#13889 = ADVANCED_FACE ( 'NONE', ( #13333 ), #922, .T. ) ;
#13890 = CARTESIAN_POINT ( 'NONE',  ( 8.882943487429999507, -98.83600327540000308, 16.35256359799999970 ) ) ;
#13891 = CARTESIAN_POINT ( 'NONE',  ( -28.31007805460000171, -40.00000000000000000, -51.82125027960000097 ) ) ;
#13892 = CARTESIAN_POINT ( 'NONE',  ( 0.5588920821209999446, -99.64579499010000063, -17.31215308460000202 ) ) ;
#13893 = FACE_OUTER_BOUND ( 'NONE', #24956, .T. ) ;
#13894 = CARTESIAN_POINT ( 'NONE',  ( 11.86104588439999930, -101.2306315440000049, -11.05401200120000027 ) ) ;
#13895 = CARTESIAN_POINT ( 'NONE',  ( -2.528726852669999747, -39.31812514059999586, -24.13485223549999859 ) ) ;
#13896 = B_SPLINE_CURVE_WITH_KNOTS ( 'NONE', 3,
 ( #27679, #27944, #7718, #14117, #16870, #25759, #25479, #14529, #9874, #7980 ),
 .UNSPECIFIED., .F., .F.,
 ( 4, 2, 2, 2, 4 ),
 ( 0.000000000000000000, 0.2500000000000000000, 0.5000000000000000000, 0.7500000000000000000, 1.000000000000000000 ),
 .UNSPECIFIED. ) ;
#13897 = CARTESIAN_POINT ( 'NONE',  ( 12.79340726668418959, -96.37047651198221843, 17.28024789624581814 ) ) ;
#13898 = DIRECTION ( 'NONE',  ( 0.000000000000000000, 1.000000000000000000, 0.000000000000000000 ) ) ;
#13899 = CARTESIAN_POINT ( 'NONE',  ( 21.30736387581682934, -36.52594040275587872, -8.753883468101205878 ) ) ;
#13900 = CARTESIAN_POINT ( 'NONE',  ( 22.06548297080000154, -49.09615641340000280, -8.529247663889998776 ) ) ;
#13901 = DIRECTION ( 'NONE',  ( 0.9704142011833032377, 0.000000000000000000, -0.2414462220490753985 ) ) ;
#13902 = CARTESIAN_POINT ( 'NONE',  ( 0.000000000000000000, -83.75000000000000000, 0.000000000000000000 ) ) ;
#13903 = VERTEX_POINT ( 'NONE', #11135 ) ;
#13904 = CARTESIAN_POINT ( 'NONE',  ( 36.38830550880000203, -74.66455843740000375, -14.80879927640000027 ) ) ;
#13905 = AXIS2_PLACEMENT_3D ( 'NONE', #17732, #274, #4466 ) ;
#13906 = AXIS2_PLACEMENT_3D ( 'NONE', #4712, #223, #17973 ) ;
#13907 = CARTESIAN_POINT ( 'NONE',  ( 7.030727077140000780, -101.5369810359999860, 14.37272453779999992 ) ) ;
#13908 = CARTESIAN_POINT ( 'NONE',  ( -22.36358135397400915, -79.84238795997771376, -32.77853236111499058 ) ) ;
#13909 = CARTESIAN_POINT ( 'NONE',  ( 8.099920077730001111, -100.8733989549999990, 13.47813240850000049 ) ) ;
#13910 = CARTESIAN_POINT ( 'NONE',  ( -14.26285779270000020, -66.60919528889999697, 22.17889389219999785 ) ) ;
#13911 = CARTESIAN_POINT ( 'NONE',  ( 19.49544348129999705, -35.50000000000000000, -8.986258391389998934 ) ) ;
#13912 = CARTESIAN_POINT ( 'NONE',  ( -12.04650752959999949, -69.29982884310000202, -25.46956806489999892 ) ) ;
#13913 = B_SPLINE_CURVE_WITH_KNOTS ( 'NONE', 3,
 ( #6696, #15557, #12645, #19370, #18200, #4647 ),
 .UNSPECIFIED., .F., .F.,
 ( 4, 2, 4 ),
 ( 0.000000000000000000, 0.5000000000000000000, 1.000000000000000000 ),
 .UNSPECIFIED. ) ;
#13914 = CARTESIAN_POINT ( 'NONE',  ( 27.11492913210000211, -72.00000000000000000, 10.50528373760000100 ) ) ;
#13915 = CARTESIAN_POINT ( 'NONE',  ( 20.64008983129999919, -36.00000000000000000, -9.237424967780000884 ) ) ;
#13916 = FACE_OUTER_BOUND ( 'NONE', #3480, .T. ) ;
#13917 = CARTESIAN_POINT ( 'NONE',  ( -11.43065410415306360, -54.25046843265613461, -22.55607764996867814 ) ) ;
#13918 = VERTEX_POINT ( 'NONE', #15668 ) ;
#13919 = AXIS2_PLACEMENT_3D ( 'NONE', #15386, #11316, #17895 ) ;
#13920 = CARTESIAN_POINT ( 'NONE',  ( -1.372953186662330349, -68.20869324698577429, -26.54380194214392219 ) ) ;
#13921 = CARTESIAN_POINT ( 'NONE',  ( -15.31473116159999925, -99.60591459030000294, -8.206551967759999400 ) ) ;
#13922 = ORIENTED_EDGE ( 'NONE', *, *, #25889, .T. ) ;
#13923 = CARTESIAN_POINT ( 'NONE',  ( -30.49520906449999913, -92.50000000000000000, 0.5405775709410000074 ) ) ;
#13924 = AXIS2_PLACEMENT_3D ( 'NONE', #25649, #21270, #3776 ) ;
#13925 = CIRCLE ( 'NONE', #6967, 32.39999999999999858 ) ;
#13926 = EDGE_CURVE ( 'NONE', #4628, #6607, #6353, .T. ) ;
#13927 = DIRECTION ( 'NONE',  ( 0.000000000000000000, 1.000000000000000000, 0.000000000000000000 ) ) ;
#13928 = CARTESIAN_POINT ( 'NONE',  ( -41.45000000000000284, -63.07912966450000880, -2.857883832489999776 ) ) ;
#13929 = DIRECTION ( 'NONE',  ( 1.000000000000000000, 0.000000000000000000, 0.000000000000000000 ) ) ;
#13930 = CARTESIAN_POINT ( 'NONE',  ( 23.25682987829999959, -94.57749572790000059, -6.685469233060000072 ) ) ;
#13931 = CARTESIAN_POINT ( 'NONE',  ( -14.44374894240000096, -74.20280742140000996, 36.65188832069999592 ) ) ;
#13932 = DIRECTION ( 'NONE',  ( 0.000000000000000000, -1.000000000000000000, 0.000000000000000000 ) ) ;
#13933 = CARTESIAN_POINT ( 'NONE',  ( -13.46935432499999941, -20.29228382570000022, 20.41725230879999842 ) ) ;
#13934 = ORIENTED_EDGE ( 'NONE', *, *, #28769, .T. ) ;
#13935 = CARTESIAN_POINT ( 'NONE',  ( -12.70614022820000066, -71.64735197429999403, -25.11726403489999981 ) ) ;
#13936 = CARTESIAN_POINT ( 'NONE',  ( 8.113044424579999969, -34.60505785169999626, -21.05852071150000171 ) ) ;
#13937 = CARTESIAN_POINT ( 'NONE',  ( -12.56556452559999926, -99.92384627689999377, -11.31794108169999902 ) ) ;
#13938 = CARTESIAN_POINT ( 'NONE',  ( -12.29363612059999866, -101.2530993000000024, -8.928690578620001261 ) ) ;
#13939 = CARTESIAN_POINT ( 'NONE',  ( 15.54119309900000090, -100.8869817940000075, 1.981729577500000339 ) ) ;
#13940 = ORIENTED_EDGE ( 'NONE', *, *, #23610, .T. ) ;
#13941 = CIRCLE ( 'NONE', #25576, 21.60095686220000033 ) ;
#13942 = CARTESIAN_POINT ( 'NONE',  ( 26.94827291246611622, -92.54893169919635909, -14.28427949690044052 ) ) ;
#13943 = EDGE_LOOP ( 'NONE', ( #14180, #9425, #17590, #22708 ) ) ;
#13944 = CIRCLE ( 'NONE', #19980, 7.750000000000000000 ) ;
#13945 = EDGE_CURVE ( 'NONE', #24813, #22412, #21546, .T. ) ;
#13946 = CARTESIAN_POINT ( 'NONE',  ( -2.353367699040000094, -57.44036955189999816, -24.34033158609999958 ) ) ;
#13947 = CARTESIAN_POINT ( 'NONE',  ( 9.452942635460001242, -37.37167648650000018, -22.96193664180000127 ) ) ;
#13948 = CARTESIAN_POINT ( 'NONE',  ( -3.732180049640000163, -98.24302442990000372, 18.85290869059999963 ) ) ;
#13949 = CARTESIAN_POINT ( 'NONE',  ( 10.50529330130000005, -92.86738811510001312, 27.55314313410000082 ) ) ;
#13950 = ORIENTED_EDGE ( 'NONE', *, *, #11222, .T. ) ;
#13951 = CARTESIAN_POINT ( 'NONE',  ( -22.50373292842316886, -69.08892850191131174, 14.88162393626444668 ) ) ;
#13952 = CARTESIAN_POINT ( 'NONE',  ( -22.83021220420000219, -92.50000647099999185, -19.05479008140000374 ) ) ;
#13953 = CARTESIAN_POINT ( 'NONE',  ( 46.77849477899999897, -74.12949171449999142, -3.288587074160000068 ) ) ;
#13954 = ORIENTED_EDGE ( 'NONE', *, *, #13396, .F. ) ;
#13955 = DIRECTION ( 'NONE',  ( 0.6285074900730002190, 0.000000000000000000, -0.7778035323410003032 ) ) ;
#13956 = CARTESIAN_POINT ( 'NONE',  ( -11.41973371908083301, -61.05366698308790774, 20.89350501692665318 ) ) ;
#13957 = CARTESIAN_POINT ( 'NONE',  ( -11.25325031930000108, -94.84397446139999488, -20.59894429220000234 ) ) ;
#13958 = CARTESIAN_POINT ( 'NONE',  ( -3.360703170379999438, -72.70510570390000282, -28.43098690960000141 ) ) ;
#13959 = CARTESIAN_POINT ( 'NONE',  ( -14.97759602049999827, -68.79203770149999286, 22.77015088919999997 ) ) ;
#13960 = ORIENTED_EDGE ( 'NONE', *, *, #19807, .T. ) ;
#13961 = AXIS2_PLACEMENT_3D ( 'NONE', #4822, #24783, #4515 ) ;
#13962 = COLOUR_RGB ( '', 0.31764706, 0.68627451, 0.89019608) ;
#13963 = CARTESIAN_POINT ( 'NONE',  ( 36.68836020269999665, -74.16367787109999199, -14.39348829000000052 ) ) ;
#13964 = CARTESIAN_POINT ( 'NONE',  ( -12.09704001540000107, -74.00000000000000000, 47.10905722069999513 ) ) ;
#13965 = CARTESIAN_POINT ( 'NONE',  ( 24.62807377229999872, -60.38561542509999924, 1.171175192380000230 ) ) ;
#13966 = CARTESIAN_POINT ( 'NONE',  ( -30.49520906449999913, -92.50000000000000000, 0.5405775709410000074 ) ) ;
#13967 = VERTEX_POINT ( 'NONE', #24428 ) ;
#13968 = DIRECTION ( 'NONE',  ( 0.9773425350887455787, 0.000000000000000000, 0.2116638115179453050 ) ) ;
#13969 = CARTESIAN_POINT ( 'NONE',  ( -7.435894661898926117, -73.99970680622588759, 39.09073924653432641 ) ) ;
#13970 = CARTESIAN_POINT ( 'NONE',  ( 23.65724685329999843, -92.50000647099999185, -18.01772143370000023 ) ) ;
#13971 = ORIENTED_EDGE ( 'NONE', *, *, #21169, .T. ) ;
#13972 = CARTESIAN_POINT ( 'NONE',  ( -9.594728507420001051, -93.84506351590000861, -23.13300608200000141 ) ) ;
#13973 = CARTESIAN_POINT ( 'NONE',  ( 21.36082767509999769, -61.85641277710000452, 10.97888673409999960 ) ) ;
#13974 = CARTESIAN_POINT ( 'NONE',  ( -39.18882116139999994, -65.49083508809999898, -2.489060262989999828 ) ) ;
#13975 = CARTESIAN_POINT ( 'NONE',  ( 16.80289107651169189, -99.96200787837224766, 4.259014394836682982 ) ) ;
#13976 = FACE_OUTER_BOUND ( 'NONE', #25558, .T. ) ;
#13977 = ORIENTED_EDGE ( 'NONE', *, *, #28515, .T. ) ;
#13978 = CARTESIAN_POINT ( 'NONE',  ( 47.11148591230000449, -79.71592019339999524, -1.801975019300000147 ) ) ;
#13979 = CONTEXT_DEPENDENT_SHAPE_REPRESENTATION ( #1978, #8725 ) ;
#13980 = CARTESIAN_POINT ( 'NONE',  ( -12.05127807179999877, -63.53922775760000263, -21.48197960690000130 ) ) ;
#13981 = CARTESIAN_POINT ( 'NONE',  ( 37.17270558886492893, -79.97602054853541631, -13.97001007350288404 ) ) ;
#13982 = CIRCLE ( 'NONE', #25171, 6.749999999999999112 ) ;
#13983 = CARTESIAN_POINT ( 'NONE',  ( 46.25000000000000000, -75.00000000000000000, -13.75000000000000000 ) ) ;
#13984 = CARTESIAN_POINT ( 'NONE',  ( 7.564829567879999012E-15, -69.50000000000000000, 47.25000000000000000 ) ) ;
#13986 = EDGE_CURVE ( 'NONE', #24255, #20007, #18098, .T. ) ;
#13985 = AXIS2_PLACEMENT_3D ( 'NONE', #26671, #11034, #6858 ) ;
#13987 = VERTEX_POINT ( 'NONE', #10698 ) ;
#13988 = AXIS2_PLACEMENT_3D ( 'NONE', #6812, #13494, #22402 ) ;
#13989 = DIRECTION ( 'NONE',  ( 0.000000000000000000, 1.000000000000000000, 0.000000000000000000 ) ) ;
#13990 = ORIENTED_EDGE ( 'NONE', *, *, #24213, .F. ) ;
#13991 = CARTESIAN_POINT ( 'NONE',  ( 20.69873715099999956, -52.63055504209999924, 10.61298605969999898 ) ) ;
#13992 = DIRECTION ( 'NONE',  ( 0.8775825618903722036, 0.000000000000000000, -0.4794255386042041156 ) ) ;
#13993 = EDGE_CURVE ( 'NONE', #24483, #21652, #25999, .T. ) ;
#13994 = EDGE_LOOP ( 'NONE', ( #24032, #26043, #25784, #17300, #6756 ) ) ;
#13995 = CARTESIAN_POINT ( 'NONE',  ( -36.92846103339999786, -69.50000000000000000, 1.677989385109999843 ) ) ;
#13996 = EDGE_CURVE ( 'NONE', #26201, #20928, #13423, .T. ) ;
#13997 = CARTESIAN_POINT ( 'NONE',  ( 2.407211674977468352, -93.02765837720274078, -29.45082399442910770 ) ) ;
#13998 = DIRECTION ( 'NONE',  ( 0.4151946956541399669, 0.5000000000001689759, 0.7600087925152558821 ) ) ;
#13999 = CARTESIAN_POINT ( 'NONE',  ( -13.13595842799045066, -101.5839620086842672, -9.219410581145925931 ) ) ;
#14000 = CARTESIAN_POINT ( 'NONE',  ( -5.417927868154690074, -95.55433702422656950, -21.95361345762339411 ) ) ;
#14001 = CARTESIAN_POINT ( 'NONE',  ( 47.01838349386816418, -79.64000543255396281, -2.294466949720601168 ) ) ;
#14002 = ORIENTED_EDGE ( 'NONE', *, *, #16116, .T. ) ;
#14003 = CARTESIAN_POINT ( 'NONE',  ( -32.56304129029999217, -80.37807044109999310, -21.91706417159999987 ) ) ;
#14004 = DIRECTION ( 'NONE',  ( 0.4707989697561778542, 0.1888473936500709438, 0.8617917335343248109 ) ) ;
#14005 = CARTESIAN_POINT ( 'NONE',  ( 26.69293917519999937, -26.90310889129999694, 48.86109741659999628 ) ) ;
#14006 = ORIENTED_EDGE ( 'NONE', *, *, #5122, .F. ) ;
#14007 = DIRECTION ( 'NONE',  ( 0.9295286103719511139, 0.000000000000000000, 0.3687499999999862554 ) ) ;
#14008 = CARTESIAN_POINT ( 'NONE',  ( -12.61948338259999858, -101.6484611540000031, -9.836088610590000059 ) ) ;
#14009 = FACE_OUTER_BOUND ( 'NONE', #21262, .T. ) ;
#14011 = VERTEX_POINT ( 'NONE', #28639 ) ;
#14010 = B_SPLINE_CURVE_WITH_KNOTS ( 'NONE', 3,
 ( #24450, #6679, #26492, #6371, #24010, #6233, #11319, #15388, #21974, #4345, #28655, #1877, #8557, #2024, #6530, #11002, #4044, #10863, #19633, #8686 ),
 .UNSPECIFIED., .F., .F.,
 ( 4, 2, 1, 2, 2, 2, 2, 1, 2, 2, 4 ),
 ( 0.000000000000000000, 0.1250000000000299760, 0.1875000000000449640, 0.2187500000000577038, 0.2500000000000704437, 0.5000000000000650591, 0.6250000000000579536, 0.6875000000000579536, 0.7187500000000521805, 0.7500000000000465183, 1.000000000000000000 ),
 .UNSPECIFIED. ) ;
#14012 = CARTESIAN_POINT ( 'NONE',  ( -3.055530165179999980, -94.70873790529999781, 23.49572270359999848 ) ) ;
#14013 = CARTESIAN_POINT ( 'NONE',  ( -19.73589946059999889, -32.67314204020000545, 14.40166454639999927 ) ) ;
#14014 = DIRECTION ( 'NONE',  ( 0.000000000000000000, 1.000000000000000000, 0.000000000000000000 ) ) ;
#14015 = CARTESIAN_POINT ( 'NONE',  ( 20.84156035690000053, -36.00000000000000000, -10.47482617329999854 ) ) ;
#14016 = CARTESIAN_POINT ( 'NONE',  ( 22.21260241310000083, -59.01992241779999659, -8.007694976899999872 ) ) ;
#14017 = CARTESIAN_POINT ( 'NONE',  ( 26.10056038380000132, -66.79872818009998525, 0.8445247833500000301 ) ) ;
#14018 = EDGE_CURVE ( 'NONE', #19383, #7537, #3850, .T. ) ;
#14019 = EDGE_LOOP ( 'NONE', ( #7805, #7705, #17043, #4510 ) ) ;
#14020 = DIRECTION ( 'NONE',  ( 0.000000000000000000, 1.000000000000000000, 0.000000000000000000 ) ) ;
#14021 = FACE_BOUND ( 'NONE', #11302, .T. ) ;
#14022 = CARTESIAN_POINT ( 'NONE',  ( 21.30736387649999841, -36.52594040320000346, -8.753883468490000652 ) ) ;
#14023 = CARTESIAN_POINT ( 'NONE',  ( 17.53803339859999966, -96.16784812509999369, 14.96109425939999937 ) ) ;
#14024 = ORIENTED_EDGE ( 'NONE', *, *, #17528, .F. ) ;
#14025 = AXIS2_PLACEMENT_3D ( 'NONE', #18750, #12307, #21216 ) ;
#14026 = CARTESIAN_POINT ( 'NONE',  ( 7.215414233289999757, -74.50000000000000000, 40.70731707320000226 ) ) ;
#14027 = CARTESIAN_POINT ( 'NONE',  ( 46.45339896309999261, -74.00000000000000000, -4.166463576890000020 ) ) ;
#14028 = CIRCLE ( 'NONE', #7973, 0.4999999999999982236 ) ;
#14029 = ADVANCED_FACE ( 'NONE', ( #14083 ), #7104, .T. ) ;
#14030 = CIRCLE ( 'NONE', #17215, 6.000000000000000000 ) ;
#14031 = LINE ( 'NONE', #10064, #5607 ) ;
#14032 = DIRECTION ( 'NONE',  ( 0.000000000000000000, -1.000000000000000000, 0.000000000000000000 ) ) ;
#14033 = CARTESIAN_POINT ( 'NONE',  ( -10.66266547438723578, -93.83956660848620857, -23.27634539248033008 ) ) ;
#14034 = B_SPLINE_CURVE_WITH_KNOTS ( 'NONE', 3,
 ( #18415, #4559, #365, #2542, #24825, #26722, #26866, #4862, #9070, #13743, #22643, #18266, #27013, #518, #7199, #27304, #2682, #20153, #22346 ),
 .UNSPECIFIED., .F., .F.,
 ( 4, 2, 2, 2, 1, 1, 1, 2, 2, 2, 4 ),
 ( 0.000000000000000000, 0.2499999999997740696, 0.3749999999996625477, 0.4374999999996090905, 0.4687499999995831668, 0.4843749999995707878, 0.4921874999995670130, 0.4960937499995651256, 0.4999999999995631272, 0.7499999999997815081, 1.000000000000000000 ),
 .UNSPECIFIED. ) ;
#14035 = FACE_OUTER_BOUND ( 'NONE', #20062, .T. ) ;
#14036 = CARTESIAN_POINT ( 'NONE',  ( 7.620081227840000082, -101.5353651350000064, 14.07009485169999863 ) ) ;
#14037 = VERTEX_POINT ( 'NONE', #14235 ) ;
#14038 = DIRECTION ( 'NONE',  ( 0.9295286103719527793, 0.000000000000000000, 0.3687499999999814260 ) ) ;
#14039 = CARTESIAN_POINT ( 'NONE',  ( 23.99041810810000186, -19.49268907760000147, 1.535546174039999823 ) ) ;
#14040 = CARTESIAN_POINT ( 'NONE',  ( 11.97116049530000126, -98.43722211939999056, -15.53505339789999873 ) ) ;
#14041 = ORIENTED_EDGE ( 'NONE', *, *, #19562, .T. ) ;
#14042 = CARTESIAN_POINT ( 'NONE',  ( -2.204108355239595252, -19.47440675035694113, -22.78057140629209698 ) ) ;
#14043 = FACE_OUTER_BOUND ( 'NONE', #28116, .T. ) ;
#14044 = CARTESIAN_POINT ( 'NONE',  ( -1.520194665700000058, -32.72716367869999488, -22.67437676309999972 ) ) ;
#14045 = CARTESIAN_POINT ( 'NONE',  ( 13.35125805077294281, -96.09071899285407881, 17.31197431996907810 ) ) ;
#14046 = LINE ( 'NONE', #3137, #9047 ) ;
#14047 = DIRECTION ( 'NONE',  ( 1.000000000000000000, 0.000000000000000000, 0.000000000000000000 ) ) ;
#14048 = FACE_OUTER_BOUND ( 'NONE', #15832, .T. ) ;
#14049 = CARTESIAN_POINT ( 'NONE',  ( 7.426814492070000107, -35.28814190290000141, -21.34788074219999743 ) ) ;
#14050 = DIRECTION ( 'NONE',  ( 0.000000000000000000, 1.000000000000000000, 0.000000000000000000 ) ) ;
#14051 = AXIS2_PLACEMENT_3D ( 'NONE', #9488, #2213, #6735 ) ;
#14052 = EDGE_LOOP ( 'NONE', ( #14329, #5984, #15787, #22212 ) ) ;
#14053 = AXIS2_PLACEMENT_3D ( 'NONE', #15118, #10460, #27991 ) ;
#14054 = CARTESIAN_POINT ( 'NONE',  ( 6.638042613879999720, -101.0956037589999994, 14.05630584859999921 ) ) ;
#14055 = CARTESIAN_POINT ( 'NONE',  ( 14.01548305848342935, -98.16872836011999937, -13.77740321380717248 ) ) ;
#14056 = EDGE_CURVE ( 'NONE', #22316, #24445, #6437, .T. ) ;
#14057 = CARTESIAN_POINT ( 'NONE',  ( -15.04362262010000073, -66.18012799950000158, 22.59069390079999806 ) ) ;
#14058 = CARTESIAN_POINT ( 'NONE',  ( 8.991798710090000313, -35.60470291170000223, -19.53731210289999964 ) ) ;
#14059 = CYLINDRICAL_SURFACE ( 'NONE', #1083, 20.64285714289999163 ) ;
#14060 = ADVANCED_FACE ( 'NONE', ( #24870 ), #24517, .T. ) ;
#14061 = CARTESIAN_POINT ( 'NONE',  ( -2.567353809430000133, -52.57401960329944757, -24.80239345939998330 ) ) ;
#14062 = CARTESIAN_POINT ( 'NONE',  ( 0.000000000000000000, -19.70310889130000120, 0.000000000000000000 ) ) ;
#14063 = CARTESIAN_POINT ( 'NONE',  ( -39.31219897219543924, -74.09468416701456306, 7.479537002224956765 ) ) ;
#14064 = EDGE_CURVE ( 'NONE', #19645, #12096, #23671, .T. ) ;
#14065 = CIRCLE ( 'NONE', #15921, 3.499999999999999556 ) ;
#14066 = SURFACE_STYLE_FILL_AREA ( #20923 ) ;
#14067 = ORIENTED_EDGE ( 'NONE', *, *, #9868, .T. ) ;
#14068 = CARTESIAN_POINT ( 'NONE',  ( 8.097647218569999694, -101.1461874760000086, 13.98396581760000146 ) ) ;
#14069 = CARTESIAN_POINT ( 'NONE',  ( 23.50753042992814557, -18.50000000000000000, 9.440918867846139761 ) ) ;
#14070 = EDGE_LOOP ( 'NONE', ( #21576, #18820, #21323, #18973 ) ) ;
#14071 = VECTOR ( 'NONE', #28753, 1000.000000000000000 ) ;
#14072 = CARTESIAN_POINT ( 'NONE',  ( -4.636291350829999812E-13, -101.6484611540000031, 1.074695887839999887E-13 ) ) ;
#14073 = ORIENTED_EDGE ( 'NONE', *, *, #25266, .F. ) ;
#14074 = CARTESIAN_POINT ( 'NONE',  ( 0.4613846910555384762, -101.2145573445051241, -16.33011699766660030 ) ) ;
#14075 = DIRECTION ( 'NONE',  ( 0.000000000000000000, -1.000000000000000000, 0.000000000000000000 ) ) ;
#14076 = DIRECTION ( 'NONE',  ( -0.5000000000001882938, 0.000000000000000000, -0.8660254037843300168 ) ) ;
#14077 = CARTESIAN_POINT ( 'NONE',  ( -7.243395527613476936, -74.19510049677808183, -40.30949744608958696 ) ) ;
#14078 = CARTESIAN_POINT ( 'NONE',  ( -14.59815767989999991, -74.50000000000000000, 36.63377406709999917 ) ) ;
#14079 = CARTESIAN_POINT ( 'NONE',  ( -4.790709198910000133, -98.40794110039999509, -18.33800208579999946 ) ) ;
#14080 = CARTESIAN_POINT ( 'NONE',  ( 14.26399793470000077, -97.58045781620000980, -14.03566137740000208 ) ) ;
#14081 = B_SPLINE_SURFACE_WITH_KNOTS ( 'NONE', 5, 5, ( 
 ( #13700, #20108, #24481, #9164, #176, #2056, #27118, #23, #13391 ),
 ( #18221, #4514, #10896, #19803, #28683, #2343, #9024, #17930, #13543 ),
 ( #22451, #2497, #24782, #11351, #21132, #22745, #18808, #2787, #14141 ),
 ( #5256, #23039, #3088, #12081, #25500, #2935, #10027, #25372, #11939 ),
 ( #1055, #5531, #27559, #25075, #23312, #7602, #23177, #7456, #20852 ),
 ( #25227, #14420, #27700, #912, #14281, #7738, #16166, #16605, #11644 ) ),
 .UNSPECIFIED., .F., .F., .F.,
 ( 6, 6 ),
 ( 6, 3, 6 ),
 ( 33.01978391549999969, 86.80576485550000143 ),
 ( 0.000000000000000000, 1.000000000000000000, 2.000000000000000000 ),
 .UNSPECIFIED. ) ;
#14082 = ORIENTED_EDGE ( 'NONE', *, *, #7478, .F. ) ;
#14083 = FACE_OUTER_BOUND ( 'NONE', #28407, .T. ) ;
#14084 = CARTESIAN_POINT ( 'NONE',  ( 8.968815321630000170, -28.58309803750000100, -19.70170933860000062 ) ) ;
#14085 = CARTESIAN_POINT ( 'NONE',  ( -0.8479692464762066395, -57.47815905588110041, -23.34776748300164684 ) ) ;
#14086 = CARTESIAN_POINT ( 'NONE',  ( -27.18988201479999844, -16.70155444569999759, -49.77074518290000071 ) ) ;
#14087 = CARTESIAN_POINT ( 'NONE',  ( 16.08037952269999948, -101.3150705500000157, 2.354224216990000063 ) ) ;
#14088 = ORIENTED_EDGE ( 'NONE', *, *, #11030, .F. ) ;
#14089 = AXIS2_PLACEMENT_3D ( 'NONE', #2329, #8857, #11181 ) ;
#14090 = B_SPLINE_CURVE_WITH_KNOTS ( 'NONE', 5,
 ( #2269, #11116, #8948, #17857, #26755, #13469, #22375, #2422, #11277 ),
 .UNSPECIFIED., .F., .F.,
 ( 6, 3, 6 ),
 ( 0.000000000000000000, 0.5000000000000000000, 1.000000000000000000 ),
 .UNSPECIFIED. ) ;
#14091 = ORIENTED_EDGE ( 'NONE', *, *, #700, .F. ) ;
#14092 = TOROIDAL_SURFACE ( 'NONE', #8945, 3.750000000000000000, 1.000000000000000000 ) ;
#14093 = ADVANCED_FACE ( 'NONE', ( #22547 ), #5200, .T. ) ;
#14094 = B_SPLINE_CURVE_WITH_KNOTS ( 'NONE', 3,
 ( #17768, #11177, #26653, #6697, #2325, #15558, #24463, #22277 ),
 .UNSPECIFIED., .F., .F.,
 ( 4, 2, 2, 4 ),
 ( 0.000000000000000000, 0.2500000000000013323, 0.5000000000000026645, 1.000000000000000000 ),
 .UNSPECIFIED. ) ;
#14095 = CARTESIAN_POINT ( 'NONE',  ( -14.14515361762423495, -80.00000000000660805, 37.00794155579307443 ) ) ;
#14096 = CARTESIAN_POINT ( 'NONE',  ( -0.7643172187030000675, -95.76596938490000355, 22.73307493400000112 ) ) ;
#14097 = ADVANCED_FACE ( 'NONE', ( #9847 ), #7552, .F. ) ;
#14098 = CARTESIAN_POINT ( 'NONE',  ( 2.785942070970000461, -93.82249895229999481, 24.67684871370000010 ) ) ;
#14099 = EDGE_LOOP ( 'NONE', ( #14477, #2644, #24943, #11950 ) ) ;
#14100 = ORIENTED_EDGE ( 'NONE', *, *, #8390, .T. ) ;
#14101 = AXIS2_PLACEMENT_3D ( 'NONE', #22286, #6848, #2331 ) ;
#14102 = CARTESIAN_POINT ( 'NONE',  ( -28.84886582594137749, -93.09721478952320695, 3.064172615184945769 ) ) ;
#14103 = CARTESIAN_POINT ( 'NONE',  ( 3.787197165510000296, -91.50000000000000000, -30.26395773239999798 ) ) ;
#14104 = CARTESIAN_POINT ( 'NONE',  ( 9.885503723209998483, -36.00000000000000000, -20.33566493420000043 ) ) ;
#14105 = ORIENTED_EDGE ( 'NONE', *, *, #13277, .F. ) ;
#14106 = CARTESIAN_POINT ( 'NONE',  ( 7.240437622353804947, -74.25043946920976623, -40.38463872251576703 ) ) ;
#14107 = CARTESIAN_POINT ( 'NONE',  ( 24.58030493329999899, -18.50000000000000000, 2.442848308399999890 ) ) ;
#14108 = DIRECTION ( 'NONE',  ( 0.000000000000000000, -1.000000000000000000, 0.000000000000000000 ) ) ;
#14109 = B_SPLINE_CURVE_WITH_KNOTS ( 'NONE', 5,
 ( #27449, #9931, #21301, #7494, #14318, #23214 ),
 .UNSPECIFIED., .F., .F.,
 ( 6, 6 ),
 ( 0.000000000000000000, 1.000000000000000000 ),
 .UNSPECIFIED. ) ;
#14110 = CARTESIAN_POINT ( 'NONE',  ( -1.403101961229999972, -65.53445078080000030, -25.32578616130000171 ) ) ;
#14111 = CIRCLE ( 'NONE', #17827, 0.5000000000000027756 ) ;
#14112 = DIRECTION ( 'NONE',  ( 0.000000000000000000, -1.000000000000000000, 0.000000000000000000 ) ) ;
#14113 = ORIENTED_EDGE ( 'NONE', *, *, #7012, .F. ) ;
#14114 = CARTESIAN_POINT ( 'NONE',  ( 36.26491344080000090, -73.99869055300000298, -14.02738897890000125 ) ) ;
#14115 = CARTESIAN_POINT ( 'NONE',  ( -16.79027416539999962, -100.2529091920000042, 3.234199557169999739 ) ) ;
#14116 = CARTESIAN_POINT ( 'NONE',  ( 24.45008145339999928, -61.97075362790000241, 0.7927955552359999825 ) ) ;
#14117 = CARTESIAN_POINT ( 'NONE',  ( -6.105915352247367700, -101.1416252791428434, 14.29215036881257994 ) ) ;
#14118 = ADVANCED_FACE ( 'NONE', ( #999 ), #454, .T. ) ;
#14119 = VERTEX_POINT ( 'NONE', #3860 ) ;
#14120 = FACE_OUTER_BOUND ( 'NONE', #6632, .T. ) ;
#14121 = CARTESIAN_POINT ( 'NONE',  ( -2.377347181619999805, -18.50000000000000000, -21.46086959390000004 ) ) ;
#14122 = CARTESIAN_POINT ( 'NONE',  ( -7.920105797075711607, -100.1585711159093535, 15.24014698975379112 ) ) ;
#14123 = VERTEX_POINT ( 'NONE', #17112 ) ;
#14124 = CARTESIAN_POINT ( 'NONE',  ( -11.35954001540000036, -80.00000000000000000, 45.25000000000000000 ) ) ;
#14125 = CIRCLE ( 'NONE', #3438, 0.4999999999999982236 ) ;
#14126 = CARTESIAN_POINT ( 'NONE',  ( 22.08519268120000234, -61.72813301749999937, 10.48040124129999917 ) ) ;
#14127 = CARTESIAN_POINT ( 'NONE',  ( -38.85038231309999901, -65.31510159580000163, -2.684458023169999930 ) ) ;
#14128 = CARTESIAN_POINT ( 'NONE',  ( 15.87518046294259655, -101.1248211537865700, 4.142658035507630565 ) ) ;
#14129 = DIRECTION ( 'NONE',  ( 1.000000000000000000, 0.000000000000000000, 0.000000000000000000 ) ) ;
#14130 = ORIENTED_EDGE ( 'NONE', *, *, #17372, .F. ) ;
#14131 = DIRECTION ( 'NONE',  ( -5.551115123129999410E-17, 0.000000000000000000, -1.000000000000000000 ) ) ;
#14132 = ADVANCED_FACE ( 'NONE', ( #25453 ), #28052, .T. ) ;
#14133 = CARTESIAN_POINT ( 'NONE',  ( -11.22008280819999904, -57.43018266680000039, -22.06025754099999858 ) ) ;
#14134 = AXIS2_PLACEMENT_3D ( 'NONE', #4163, #1436, #3744 ) ;
#14135 = CYLINDRICAL_SURFACE ( 'NONE', #15382, 11.00000000000000000 ) ;
#14136 = CARTESIAN_POINT ( 'NONE',  ( 21.34788034980000049, -35.28814072549999281, -7.426815654249999454 ) ) ;
#14137 = VERTEX_POINT ( 'NONE', #3305 ) ;
#14138 = LINE ( 'NONE', #5103, #1049 ) ;
#14139 = CARTESIAN_POINT ( 'NONE',  ( 22.95301417039999592, -94.52293512109999085, -6.773259939029999899 ) ) ;
#14140 = ORIENTED_EDGE ( 'NONE', *, *, #1947, .T. ) ;
#14141 = CARTESIAN_POINT ( 'NONE',  ( -13.67553535689999933, -42.20265308159999762, 20.91818002200000137 ) ) ;
#14142 = DIRECTION ( 'NONE',  ( 0.3388747807339289597, 0.000000000000000000, 0.9408314849018030168 ) ) ;
#14143 = VERTEX_POINT ( 'NONE', #26002 ) ;
#14144 = LINE ( 'NONE', #9321, #5719 ) ;
#14145 = AXIS2_PLACEMENT_3D ( 'NONE', #14124, #27243, #22729 ) ;
#14146 = ORIENTED_EDGE ( 'NONE', *, *, #5182, .F. ) ;
#14147 = CIRCLE ( 'NONE', #28106, 30.50000000000000000 ) ;
#14148 = FACE_OUTER_BOUND ( 'NONE', #1940, .T. ) ;
#14149 = CARTESIAN_POINT ( 'NONE',  ( -10.45871993891135077, -19.47933382267855151, -20.72446925435193421 ) ) ;
#14150 = CARTESIAN_POINT ( 'NONE',  ( -12.07243358760000085, -19.50000000000000000, -24.77970463289999969 ) ) ;
#14151 = CARTESIAN_POINT ( 'NONE',  ( -2.004269379255393613, -97.53591929645209291, -19.96958644832030316 ) ) ;
#14152 = CARTESIAN_POINT ( 'NONE',  ( 0.000000000000000000, -84.00000000000000000, 0.000000000000000000 ) ) ;
#14153 = ORIENTED_EDGE ( 'NONE', *, *, #19729, .F. ) ;
#14154 = CARTESIAN_POINT ( 'NONE',  ( 2.876553231629999985, -108.5000000000000000, 5.265495371340000119 ) ) ;
#14155 = B_SPLINE_CURVE_WITH_KNOTS ( 'NONE', 3,
 ( #25162, #7239, #22831, #269, #7097, #24865, #27496, #14077, #16405, #9692, #9558, #7546, #5039, #4899, #27341, #705, #18457, #9111, #13779, #2435, #24721, #9258, #11580, #4605, #2874, #20335, #18157, #7386, #20795, #4758, #20488, #11732, #5193 ),
 .UNSPECIFIED., .F., .F.,
 ( 4, 2, 2, 1, 1, 1, 2, 2, 2, 1, 1, 1, 2, 2, 2, 1, 1, 1, 2, 2, 4 ),
 ( 0.000000000000000000, 0.1250000000000962286, 0.1875000000001503520, 0.2187500000001845191, 0.2343750000002016165, 0.2421875000002045586, 0.2460937500002118861, 0.2500000000002191580, 0.3750000000000335287, 0.4374999999999393263, 0.4687499999998910316, 0.4843749999998623323, 0.4921874999998526179, 0.4999999999998428479, 0.6249999999997827294, 0.6874999999997485345, 0.7187499999997233324, 0.7343749999997187805, 0.7421874999997200018, 0.7499999999997212230, 1.000000000000000000 ),
 .UNSPECIFIED. ) ;
#14156 = CARTESIAN_POINT ( 'NONE',  ( 15.99006255310108493, -101.4218099524899657, 2.411354960305282180 ) ) ;
#14157 = EDGE_CURVE ( 'NONE', #20989, #4763, #17619, .T. ) ;
#14158 = CARTESIAN_POINT ( 'NONE',  ( -12.03627366839999802, -92.50000000000000000, 28.02459841239999960 ) ) ;
#14159 = VERTEX_POINT ( 'NONE', #23542 ) ;
#14160 = CIRCLE ( 'NONE', #16960, 55.67692378859999991 ) ;
#14161 = CARTESIAN_POINT ( 'NONE',  ( -12.13775690249999961, -101.1411470200000053, -9.460613307739999200 ) ) ;
#14162 = CARTESIAN_POINT ( 'NONE',  ( 22.58213832176329916, -18.62337006874614076, 9.587758685844438133 ) ) ;
#14163 = ORIENTED_EDGE ( 'NONE', *, *, #14568, .F. ) ;
#14164 = ADVANCED_FACE ( 'NONE', ( #28188 ), #20912, .F. ) ;
#14165 = CARTESIAN_POINT ( 'NONE',  ( -17.36676170379999817, -98.30606121530000507, 8.776474676399999453 ) ) ;
#14166 = CARTESIAN_POINT ( 'NONE',  ( -19.08606228369999869, -39.36011816909999794, 12.73950996719999829 ) ) ;
#14167 = CARTESIAN_POINT ( 'NONE',  ( -0.1779554536940000098, -111.0000000000000000, -15.99901033990000165 ) ) ;
#14168 = CARTESIAN_POINT ( 'NONE',  ( 30.51745573710000059, -72.51545259190000081, -23.74117753099999817 ) ) ;
#14169 = EDGE_CURVE ( 'NONE', #26731, #1871, #16225, .T. ) ;
#14170 = CARTESIAN_POINT ( 'NONE',  ( 22.56729896340000252, -60.49415570080000037, -8.664781794339999621 ) ) ;
#14171 = CIRCLE ( 'NONE', #15524, 30.50000000000000000 ) ;
#14172 = CARTESIAN_POINT ( 'NONE',  ( 25.99900580609999778, -64.47177033809998647, 1.411681635039999883 ) ) ;
#14173 = CIRCLE ( 'NONE', #12279, 7.249999999999999112 ) ;
#14174 = B_SPLINE_CURVE_WITH_KNOTS ( 'NONE', 3,
 ( #6449, #15315, #22055, #27009, #11244, #22340, #10938, #22496, #9066, #17969, #20445, #11393, #26863, #6903, #19844, #69, #2234, #13740, #22640, #13588, #15916, #15464, #19996, #515, #6758, #15621, #24521, #24821, #2679, #9362, #11837, #2978, #7196 ),
 .UNSPECIFIED., .F., .F.,
 ( 4, 2, 2, 1, 1, 1, 2, 2, 2, 2, 1, 2, 2, 2, 2, 1, 2, 2, 4 ),
 ( 0.000000000000000000, 0.1249999999998855915, 0.1874999999998287481, 0.2187499999998012978, 0.2343749999997877531, 0.2421874999997861155, 0.2460937499997827016, 0.2499999999997792877, 0.3749999999998528399, 0.4374999999998868128, 0.4687499999999028000, 0.4843749999999092948, 0.4999999999999157341, 0.6249999999999484857, 0.6874999999999675815, 0.7187499999999762412, 0.7343749999999791278, 0.7499999999999819034, 1.000000000000000000 ),
 .UNSPECIFIED. ) ;
#14175 = DIRECTION ( 'NONE',  ( 0.000000000000000000, 1.000000000000000000, 0.000000000000000000 ) ) ;
#14176 = ORIENTED_EDGE ( 'NONE', *, *, #2528, .T. ) ;
#14177 = CARTESIAN_POINT ( 'NONE',  ( -39.31656870549072380, -73.61799623142519522, -7.217717631503997033 ) ) ;
#14178 = CARTESIAN_POINT ( 'NONE',  ( 21.49088915159999758, -36.91774715450000599, -8.428213728399999383 ) ) ;
#14179 = CARTESIAN_POINT ( 'NONE',  ( -7.627568735119999666, -74.00000000000000000, -38.62788659690000515 ) ) ;
#14180 = ORIENTED_EDGE ( 'NONE', *, *, #7384, .T. ) ;
#14181 = TOROIDAL_SURFACE ( 'NONE', #24397, 3.500000000000000000, 0.5000000000000000000 ) ;
#14182 = LINE ( 'NONE', #23868, #4584 ) ;
#14183 = CARTESIAN_POINT ( 'NONE',  ( -11.85289063449999958, -94.98812477599999227, -21.44324726029999795 ) ) ;
#14184 = DIRECTION ( 'NONE',  ( 0.000000000000000000, 1.000000000000000000, 0.000000000000000000 ) ) ;
#14185 = CIRCLE ( 'NONE', #4880, 0.8000000000000000444 ) ;
#14186 = CARTESIAN_POINT ( 'NONE',  ( 6.850353673539999910, -36.56979899590000116, -21.56931441210000244 ) ) ;
#14187 = CARTESIAN_POINT ( 'NONE',  ( 7.491713480479999632, -101.1706547440000037, 13.83665357419999964 ) ) ;
#14188 = VERTEX_POINT ( 'NONE', #12721 ) ;
#14189 = CARTESIAN_POINT ( 'NONE',  ( -43.20000000000000284, -65.14977478849999670, -0.1732050807570000017 ) ) ;
#14190 = CARTESIAN_POINT ( 'NONE',  ( -29.47186158120000243, -92.84292488370000740, -0.4149714379639999895 ) ) ;
#14191 = CARTESIAN_POINT ( 'NONE',  ( -12.96004524251607570, -19.48405186614310480, 19.61898934477310519 ) ) ;
#14192 = DIRECTION ( 'NONE',  ( 0.000000000000000000, 1.000000000000000000, 0.000000000000000000 ) ) ;
#14193 = ORIENTED_EDGE ( 'NONE', *, *, #11193, .F. ) ;
#14194 = AXIS2_PLACEMENT_3D ( 'NONE', #26571, #18121, #4561 ) ;
#14195 = CARTESIAN_POINT ( 'NONE',  ( -1.163833269605216492, -19.46453794989949770, -22.07359787591765610 ) ) ;
#14196 = EDGE_CURVE ( 'NONE', #20007, #14226, #16699, .T. ) ;
#14197 = DIRECTION ( 'NONE',  ( 0.000000000000000000, 1.000000000000000000, 0.000000000000000000 ) ) ;
#14198 = CARTESIAN_POINT ( 'NONE',  ( -2.013197380030000261, -45.98073373379999396, -23.47693395669999816 ) ) ;
#14199 = DIRECTION ( 'NONE',  ( -1.000000000000000000, 0.000000000000000000, -1.836909530729999990E-16 ) ) ;
#14200 = EDGE_CURVE ( 'NONE', #21056, #7866, #3718, .T. ) ;
#14201 = CARTESIAN_POINT ( 'NONE',  ( -38.71641004229999794, -73.50000000000000000, 7.135467526410000261 ) ) ;
#14202 = CARTESIAN_POINT ( 'NONE',  ( 11.90208458877192932, -101.5703832412493455, -10.78058033292013640 ) ) ;
#14203 = CARTESIAN_POINT ( 'NONE',  ( 21.57753409760000096, -40.74985578519999763, -7.517162733340000180 ) ) ;
#14204 = ADVANCED_FACE ( 'NONE', ( #12438 ), #1144, .T. ) ;
#14205 = CARTESIAN_POINT ( 'NONE',  ( 27.18988201479999844, -18.49844555430000170, 49.77074518290000071 ) ) ;
#14206 = CARTESIAN_POINT ( 'NONE',  ( 0.000000000000000000, -30.50310889129999836, 0.000000000000000000 ) ) ;
#14207 = ORIENTED_EDGE ( 'NONE', *, *, #25763, .T. ) ;
#14208 = EDGE_CURVE ( 'NONE', #17600, #11169, #20434, .T. ) ;
#14209 = CARTESIAN_POINT ( 'NONE',  ( 6.789115400040000026, -101.1417990620000040, 14.22050701429999897 ) ) ;
#14210 = CARTESIAN_POINT ( 'NONE',  ( -37.36725231429999639, -94.00000000000000000, 1.438276615809999992 ) ) ;
#14211 = AXIS2_PLACEMENT_3D ( 'NONE', #985, #25572, #25148 ) ;
#14212 = CARTESIAN_POINT ( 'NONE',  ( 7.462391103660000802, -101.2375126459999848, 13.25959037569999843 ) ) ;
#14213 = CARTESIAN_POINT ( 'NONE',  ( -11.17107965319999963, -94.77693780670000478, -20.89252829639999831 ) ) ;
#14214 = CARTESIAN_POINT ( 'NONE',  ( 7.844208135530000625, -36.11002484140000490, -21.41825414589999710 ) ) ;
#14215 = CARTESIAN_POINT ( 'NONE',  ( 11.70455088819999823, -101.1889999979999999, 8.942783294160001617 ) ) ;
#14216 = CONICAL_SURFACE ( 'NONE', #8580, 25.14975229270001833, 0.4276056667390000787 ) ;
#14217 = CARTESIAN_POINT ( 'NONE',  ( -1.993723132860002245, -52.61368720119944697, -23.68602550419998209 ) ) ;
#14218 = DIRECTION ( 'NONE',  ( 0.000000000000000000, 1.000000000000000000, 0.000000000000000000 ) ) ;
#14219 = CARTESIAN_POINT ( 'NONE',  ( -20.57686592631715072, -93.08494709825977509, -20.57755909579458375 ) ) ;
#14220 = FILL_AREA_STYLE_COLOUR ( '', #18293 ) ;
#14221 = ORIENTED_EDGE ( 'NONE', *, *, #14963, .F. ) ;
#14222 = CARTESIAN_POINT ( 'NONE',  ( 31.23163825569150731, -74.11403145701621042, -23.50616654247474813 ) ) ;
#14223 = CARTESIAN_POINT ( 'NONE',  ( -15.54410891719999910, -99.75094652210000845, -8.801109042589999376 ) ) ;
#14224 = EDGE_LOOP ( 'NONE', ( #5379, #1189, #17267, #8806, #11643, #15896, #19521 ) ) ;
#14225 = CARTESIAN_POINT ( 'NONE',  ( 23.03829042120000281, -52.56313962710000709, 10.32398954119999956 ) ) ;
#14226 = VERTEX_POINT ( 'NONE', #19438 ) ;
#14227 = CARTESIAN_POINT ( 'NONE',  ( 0.5404583983271005199, -100.1994045927584693, -17.13382711562018201 ) ) ;
#14228 = B_SPLINE_CURVE_WITH_KNOTS ( 'NONE', 5,
 ( #12295, #21206, #18449, #3017, #27487, #27636 ),
 .UNSPECIFIED., .F., .F.,
 ( 6, 6 ),
 ( 0.000000000000000000, 1.000000000000000000 ),
 .UNSPECIFIED. ) ;
#14229 = CARTESIAN_POINT ( 'NONE',  ( 29.17304402409999753, -39.50000000000000000, 53.40089889099999709 ) ) ;
#14230 = EDGE_CURVE ( 'NONE', #13209, #11679, #17052, .T. ) ;
#14231 = CARTESIAN_POINT ( 'NONE',  ( 23.56216202090000067, -73.65810230149999427, -30.93625454709999900 ) ) ;
#14232 = EDGE_CURVE ( 'NONE', #5689, #26262, #4111, .T. ) ;
#14233 = CARTESIAN_POINT ( 'NONE',  ( 0.000000000000000000, -111.0000000000000000, 0.000000000000000000 ) ) ;
#14234 = CARTESIAN_POINT ( 'NONE',  ( 23.86725312652073683, -92.82709422631835139, -18.98958227918895147 ) ) ;
#14235 = CARTESIAN_POINT ( 'NONE',  ( -1.283023294879999998, -101.3150694429999987, -16.20107482390000087 ) ) ;
#14236 = CARTESIAN_POINT ( 'NONE',  ( 7.691806989790000770, -28.53090832400000210, -20.98512114160000053 ) ) ;
#14237 = CARTESIAN_POINT ( 'NONE',  ( -0.5413028987460000163, -57.47855601759999900, -23.35488904649999853 ) ) ;
#14238 = DIRECTION ( 'NONE',  ( 1.000000000000000000, 0.000000000000000000, 0.000000000000000000 ) ) ;
#14239 = ORIENTED_EDGE ( 'NONE', *, *, #301, .F. ) ;
#14240 = EDGE_CURVE ( 'NONE', #13063, #23453, #11065, .T. ) ;
#14241 = ORIENTED_EDGE ( 'NONE', *, *, #19698, .T. ) ;
#14242 = CARTESIAN_POINT ( 'NONE',  ( -2.585646219300000048, -58.19955223950000089, -25.25977729030000063 ) ) ;
#14243 = CARTESIAN_POINT ( 'NONE',  ( -3.641088133819999850, -98.26007808079999961, 18.80451095879999812 ) ) ;
#14244 = CARTESIAN_POINT ( 'NONE',  ( 10.51100516569999854, -92.56539259249998963, 27.27496703559999958 ) ) ;
#14245 = ORIENTED_EDGE ( 'NONE', *, *, #27347, .T. ) ;
#14246 = CARTESIAN_POINT ( 'NONE',  ( -28.69446774251560939, -93.12686943463702960, 2.652929931884275838 ) ) ;
#14247 = CARTESIAN_POINT ( 'NONE',  ( 22.08144638359999945, -37.65454154180000046, -8.887095524860001206 ) ) ;
#14248 = DIRECTION ( 'NONE',  ( -0.000000000000000000, 1.000000000000000000, 0.000000000000000000 ) ) ;
#14249 = EDGE_LOOP ( 'NONE', ( #20400, #15038, #2900, #2017 ) ) ;
#14250 = TOROIDAL_SURFACE ( 'NONE', #17963, 9.000000000000000000, 1.000000000000000000 ) ;
#14251 = DIRECTION ( 'NONE',  ( -0.9295286103719527793, 0.000000000000000000, -0.3687499999999814260 ) ) ;
#14252 = DIRECTION ( 'NONE',  ( 0.000000000000000000, -1.000000000000000000, 0.000000000000000000 ) ) ;
#14253 = CARTESIAN_POINT ( 'NONE',  ( -14.81965868650000040, -80.12520894669999905, 36.34494071330000509 ) ) ;
#14254 = CARTESIAN_POINT ( 'NONE',  ( -2.686253848720000281, -64.98911155900000836, -26.08437766659999824 ) ) ;
#14255 = CARTESIAN_POINT ( 'NONE',  ( -13.44405896729999839, -68.28990507160000334, 22.97003116759999841 ) ) ;
#14256 = ORIENTED_EDGE ( 'NONE', *, *, #1002, .F. ) ;
#14257 = CARTESIAN_POINT ( 'NONE',  ( -14.66608910859999959, -79.49999990052810972, 36.47374631070000106 ) ) ;
#14258 = EDGE_CURVE ( 'NONE', #1054, #23896, #14286, .T. ) ;
#14259 = CARTESIAN_POINT ( 'NONE',  ( -16.51010518360000034, -100.0706250509999933, 2.778373719329999769 ) ) ;
#14260 = CARTESIAN_POINT ( 'NONE',  ( 25.02058483049999538, -57.41946977210000114, 1.375913446200000001 ) ) ;
#14261 = CARTESIAN_POINT ( 'NONE',  ( -20.55514986509999886, -63.54004463729999230, 13.57251594750000123 ) ) ;
#14262 = ORIENTED_EDGE ( 'NONE', *, *, #13690, .T. ) ;
#14263 = CARTESIAN_POINT ( 'NONE',  ( 0.000000000000000000, -89.00000000000000000, 0.000000000000000000 ) ) ;
#14264 = CARTESIAN_POINT ( 'NONE',  ( -2.900367791859999933, -18.50000000000000000, -22.38632968349999786 ) ) ;
#14265 = CARTESIAN_POINT ( 'NONE',  ( -7.918607114148264792, -100.1240332945198759, 15.27233837034834529 ) ) ;
#14266 = VERTEX_POINT ( 'NONE', #1825 ) ;
#14267 = CARTESIAN_POINT ( 'NONE',  ( -14.16021440419999955, -18.50000000000000000, 19.51963099740000018 ) ) ;
#14268 = CARTESIAN_POINT ( 'NONE',  ( 0.000000000000000000, -90.50000000000000000, 0.000000000000000000 ) ) ;
#14269 = CARTESIAN_POINT ( 'NONE',  ( -41.74999999999999289, -65.67306013599217351, -1.491601497600667958 ) ) ;
#14270 = CARTESIAN_POINT ( 'NONE',  ( 15.91717527196672854, -101.0610180774675371, 4.179821879114435035 ) ) ;
#14271 = CARTESIAN_POINT ( 'NONE',  ( -12.99961906594058370, -67.23928497083132072, 22.67538121095307346 ) ) ;
#14272 = VERTEX_POINT ( 'NONE', #19581 ) ;
#14273 = CARTESIAN_POINT ( 'NONE',  ( -11.54098094750000136, -61.67863912299999640, -22.71160036779999913 ) ) ;
#14274 = CARTESIAN_POINT ( 'NONE',  ( 25.99810659739999963, -69.13393204870000375, -10.72511447639999993 ) ) ;
#14275 = CARTESIAN_POINT ( 'NONE',  ( 9.630000870221753217, -93.08383529948000046, 27.46986062684589669 ) ) ;
#14276 = ORIENTED_EDGE ( 'NONE', *, *, #19435, .T. ) ;
#14277 = EDGE_CURVE ( 'NONE', #22701, #10529, #6624, .T. ) ;
#14278 = LINE ( 'NONE', #20849, #4236 ) ;
#14279 = CARTESIAN_POINT ( 'NONE',  ( 2.636840462319999912, -110.0000000000000000, 4.826704090399999814 ) ) ;
#14280 = VERTEX_POINT ( 'NONE', #26154 ) ;
#14281 = CARTESIAN_POINT ( 'NONE',  ( -12.31618287409999901, -19.44965574909999617, 19.12321486129999926 ) ) ;
#14282 = CARTESIAN_POINT ( 'NONE',  ( -6.158276018989999656, -101.3256027080000052, 14.66656444329999864 ) ) ;
#14283 = ORIENTED_EDGE ( 'NONE', *, *, #5146, .T. ) ;
#14284 = DIRECTION ( 'NONE',  ( 0.000000000000000000, 1.000000000000000000, 0.000000000000000000 ) ) ;
#14285 = DIRECTION ( 'NONE',  ( 1.000000000000000000, 0.000000000000000000, 0.000000000000000000 ) ) ;
#14286 = B_SPLINE_CURVE_WITH_KNOTS ( 'NONE', 5,
 ( #21218, #25869, #16981, #14646, #23674, #10108, #16840, #25729, #15332 ),
 .UNSPECIFIED., .F., .F.,
 ( 6, 3, 6 ),
 ( 0.000000000000000000, 0.5000000000000000000, 1.000000000000000000 ),
 .UNSPECIFIED. ) ;
#14287 = CARTESIAN_POINT ( 'NONE',  ( 0.000000000000000000, -92.50000000000000000, 29.91857981989999971 ) ) ;
#14288 = CARTESIAN_POINT ( 'NONE',  ( -11.29202010641374621, -19.46468326931980997, -18.92074617257421920 ) ) ;
#14289 = FACE_OUTER_BOUND ( 'NONE', #11706, .T. ) ;
#14290 = DIRECTION ( 'NONE',  ( 0.8775825618903722036, 0.000000000000000000, -0.4794255386042041156 ) ) ;
#14291 = CARTESIAN_POINT ( 'NONE',  ( 47.09481590257341566, -79.53590158212925587, -1.887627026932961138 ) ) ;
#14292 = ORIENTED_EDGE ( 'NONE', *, *, #22620, .F. ) ;
#14293 = CARTESIAN_POINT ( 'NONE',  ( 12.94734957360000038, -94.70873790539999959, -19.84316983170000270 ) ) ;
#14294 = EDGE_CURVE ( 'NONE', #25354, #3493, #13303, .T. ) ;
#14295 = DIRECTION ( 'NONE',  ( -1.000000000000000000, 0.000000000000000000, -3.154042683594194627E-16 ) ) ;
#14296 = CARTESIAN_POINT ( 'NONE',  ( -32.61798281429999946, -80.00000000000000000, -22.71848787769999944 ) ) ;
#14297 = VERTEX_POINT ( 'NONE', #24395 ) ;
#14298 = CARTESIAN_POINT ( 'NONE',  ( 13.78600338218322818, -95.55433702442398669, -17.92376068152854529 ) ) ;
#14299 = DIRECTION ( 'NONE',  ( 0.000000000000000000, 1.000000000000000000, 0.000000000000000000 ) ) ;
#14300 = ORIENTED_EDGE ( 'NONE', *, *, #21606, .T. ) ;
#14301 = EDGE_CURVE ( 'NONE', #1715, #17343, #5059, .T. ) ;
#14302 = DIRECTION ( 'NONE',  ( 0.4396719266362648648, 0.000000000000000000, -0.8981584475625418174 ) ) ;
#14303 = CARTESIAN_POINT ( 'NONE',  ( -19.51583823489999858, -52.61368720120000120, 13.56962763329999966 ) ) ;
#14304 = DIRECTION ( 'NONE',  ( 0.4794255386042040046, 0.000000000000000000, 0.8775825618903722036 ) ) ;
#14305 = CARTESIAN_POINT ( 'NONE',  ( 31.96452224769999617, -73.88714870409999946, -21.93835394839999964 ) ) ;
#14306 = CARTESIAN_POINT ( 'NONE',  ( 23.56559805210000036, -58.81638232979999970, -9.577937461890000392 ) ) ;
#14307 = CONICAL_SURFACE ( 'NONE', #6379, 13.13304743849999667, 0.9119902906770002149 ) ;
#14308 = ORIENTED_EDGE ( 'NONE', *, *, #11539, .T. ) ;
#14309 = ADVANCED_FACE ( 'NONE', ( #20165 ), #21347, .T. ) ;
#14310 = DIRECTION ( 'NONE',  ( 0.000000000000000000, -1.000000000000000000, 0.000000000000000000 ) ) ;
#14311 = ADVANCED_FACE ( 'NONE', ( #8506 ), #27416, .T. ) ;
#14312 = CONICAL_SURFACE ( 'NONE', #6386, 1.732050807582486307, 1.047197551199999799 ) ;
#14313 = CARTESIAN_POINT ( 'NONE',  ( 20.26985721470000001, -35.99252858750000428, -9.303161554559999047 ) ) ;
#14314 = DIRECTION ( 'NONE',  ( -0.000000000000000000, 1.000000000000000000, 0.000000000000000000 ) ) ;
#14315 = ORIENTED_EDGE ( 'NONE', *, *, #13439, .T. ) ;
#14316 = CARTESIAN_POINT ( 'NONE',  ( -13.16239993169999956, -100.8816835080000089, -8.729908192910000864 ) ) ;
#14317 = B_SPLINE_SURFACE_WITH_KNOTS ( 'NONE', 5, 5, ( 
 ( #12575, #7688, #23400, #23540, #25865, #7812, #12166, #28049, #1545 ),
 ( #21346, #10250, #10105, #25313, #12436, #19302, #27911, #21489, #27646 ),
 ( #5341, #1405, #1140, #28186, #5757, #5616, #3576, #12019, #16553 ),
 ( #14770, #3715, #8217, #14231, #7949, #14499, #16837, #14367, #23260 ),
 ( #18892, #20936, #14641, #19025, #25449, #3165, #9978, #8087, #3303 ),
 ( #27774, #16686, #25590, #3440, #19163, #5892, #23119, #5480, #996 ) ),
 .UNSPECIFIED., .F., .F., .F.,
 ( 6, 6 ),
 ( 6, 3, 6 ),
 ( 0.000000000000000000, 12.56695009720000122 ),
 ( 0.000000000000000000, 1.000000000000000000, 2.000000000000000000 ),
 .UNSPECIFIED. ) ;
#14318 = CARTESIAN_POINT ( 'NONE',  ( -21.05833095636783270, -65.01950792717818217, 13.71407545850738785 ) ) ;
#14319 = CARTESIAN_POINT ( 'NONE',  ( 6.153538985549999119, -93.00000450890000536, 28.82528036289999918 ) ) ;
#14320 = CYLINDRICAL_SURFACE ( 'NONE', #2023, 9.500000000000001776 ) ;
#14321 = ADVANCED_FACE ( 'NONE', ( #4288 ), #11095, .T. ) ;
#14322 = CARTESIAN_POINT ( 'NONE',  ( 7.307353180730000730, -101.1411471079999984, 13.54367522859999973 ) ) ;
#14323 = ORIENTED_EDGE ( 'NONE', *, *, #3278, .T. ) ;
#14324 = AXIS2_PLACEMENT_3D ( 'NONE', #17824, #361, #8765 ) ;
#14325 = CARTESIAN_POINT ( 'NONE',  ( -40.42867112537203411, -74.28469014306668328, 7.237400523868926072 ) ) ;
#14326 = FACE_OUTER_BOUND ( 'NONE', #24191, .T. ) ;
#14327 = CARTESIAN_POINT ( 'NONE',  ( -12.98455916887866479, -19.48459622965902938, 19.64307623567460936 ) ) ;
#14328 = CARTESIAN_POINT ( 'NONE',  ( 11.54254854999999935, -98.24302442830000359, -15.36655156750000017 ) ) ;
#14329 = ORIENTED_EDGE ( 'NONE', *, *, #7024, .F. ) ;
#14330 = CARTESIAN_POINT ( 'NONE',  ( 19.98345451299999809, -18.50000000000000000, -7.491375432139999901 ) ) ;
#14331 = DIRECTION ( 'NONE',  ( 0.000000000000000000, -1.000000000000000000, 0.000000000000000000 ) ) ;
#14332 = DIRECTION ( 'NONE',  ( 0.000000000000000000, 1.000000000000000000, 0.000000000000000000 ) ) ;
#14333 = DIRECTION ( 'NONE',  ( 0.000000000000000000, 1.000000000000000000, 0.000000000000000000 ) ) ;
#14334 = CARTESIAN_POINT ( 'NONE',  ( -1.851961808682860200, -74.06886391613052467, 47.01299730337805016 ) ) ;
#14335 = AXIS2_PLACEMENT_3D ( 'NONE', #28221, #23298, #21530 ) ;
#14336 = DIRECTION ( 'NONE',  ( 0.8775825618903724257, 0.000000000000000000, 0.4794255386042036160 ) ) ;
#14337 = CARTESIAN_POINT ( 'NONE',  ( 22.83553957720000227, -53.24879282940000280, -9.272014655159999563 ) ) ;
#14338 = CARTESIAN_POINT ( 'NONE',  ( -39.48500436417592141, -74.13942000225500806, -7.435977656810683456 ) ) ;
#14339 = CARTESIAN_POINT ( 'NONE',  ( 36.24656906829999770, -74.82938568209999630, -15.05817820240000060 ) ) ;
#14340 = ORIENTED_EDGE ( 'NONE', *, *, #589, .F. ) ;
#14341 = CARTESIAN_POINT ( 'NONE',  ( 6.615597047280000531, -101.2530993010000060, 13.67879707989999893 ) ) ;
#14342 = CARTESIAN_POINT ( 'NONE',  ( 12.82422237299999956, -94.98812477769999418, -19.93894812050000098 ) ) ;
#14343 = CARTESIAN_POINT ( 'NONE',  ( 7.521915565509999624, -101.1193270250000040, 13.57310074129999933 ) ) ;
#14344 = AXIS2_PLACEMENT_3D ( 'NONE', #3700, #18735, #21200 ) ;
#14345 = CARTESIAN_POINT ( 'NONE',  ( -11.76876610979999960, -94.80026829410000744, -21.40432538299999976 ) ) ;
#14346 = AXIS2_PLACEMENT_3D ( 'NONE', #27974, #10576, #8011 ) ;
#14347 = CARTESIAN_POINT ( 'NONE',  ( 21.12347101519999981, -34.87913938230000355, -8.043102957309999468 ) ) ;
#14348 = DIRECTION ( 'NONE',  ( 0.000000000000000000, 1.000000000000000000, 0.000000000000000000 ) ) ;
#14349 = AXIS2_PLACEMENT_3D ( 'NONE', #26217, #10727, #6245 ) ;
#14350 = DIRECTION ( 'NONE',  ( 1.000000000000000000, 0.000000000000000000, 0.000000000000000000 ) ) ;
#14351 = CARTESIAN_POINT ( 'NONE',  ( -3.252988965690000178, -72.00000000000000000, -30.32986301179999700 ) ) ;
#14352 = CARTESIAN_POINT ( 'NONE',  ( -39.48497135293115434, -74.13941005061472822, 7.435983480943145096 ) ) ;
#14353 = EDGE_CURVE ( 'NONE', #24664, #6516, #24533, .T. ) ;
#14354 = DIRECTION ( 'NONE',  ( 0.000000000000000000, 0.000000000000000000, -1.000000000000000000 ) ) ;
#14355 = ORIENTED_EDGE ( 'NONE', *, *, #24788, .T. ) ;
#14356 = CARTESIAN_POINT ( 'NONE',  ( -1.061013842608576230, -66.63438001457079451, -25.83911284170473621 ) ) ;
#14357 = CARTESIAN_POINT ( 'NONE',  ( -42.25000000000000000, -63.00000000000000000, -0.7216878364880000563 ) ) ;
#14358 = ORIENTED_EDGE ( 'NONE', *, *, #11016, .F. ) ;
#14359 = ADVANCED_FACE ( 'NONE', ( #22357 ), #6465, .T. ) ;
#14360 = DIRECTION ( 'NONE',  ( 1.000000000000000000, 0.000000000000000000, 0.000000000000000000 ) ) ;
#14361 = EDGE_CURVE ( 'NONE', #15244, #10596, #7326, .T. ) ;
#14362 = CARTESIAN_POINT ( 'NONE',  ( 0.5870844549389877542, -100.3617719035924978, -17.00173476966439878 ) ) ;
#14363 = CARTESIAN_POINT ( 'NONE',  ( 6.615597047280000531, -101.2530993010000060, 13.67879707989999893 ) ) ;
#14364 = DIRECTION ( 'NONE',  ( 0.9144078985680119676, 0.000000000000000000, 0.4047940155640056270 ) ) ;
#14365 = CARTESIAN_POINT ( 'NONE',  ( 19.97576656849999921, -36.00000000000000000, -19.97576656849999921 ) ) ;
#14366 = FACE_BOUND ( 'NONE', #15613, .T. ) ;
#14367 = CARTESIAN_POINT ( 'NONE',  ( 23.69384752110000036, -72.68281501180000248, -30.54094685289999944 ) ) ;
#14368 = AXIS2_PLACEMENT_3D ( 'NONE', #3337, #16003, #18790 ) ;
#14369 = DIRECTION ( 'NONE',  ( 1.000000000000000000, 0.000000000000000000, 0.000000000000000000 ) ) ;
#14370 = CARTESIAN_POINT ( 'NONE',  ( 14.09492607880000037, -96.58372172939999700, -15.97495134070000056 ) ) ;
#14371 = VECTOR ( 'NONE', #2533, 1000.000000000000114 ) ;
#14372 = CARTESIAN_POINT ( 'NONE',  ( 0.000000000000000000, -33.79999999999999716, 0.000000000000000000 ) ) ;
#14373 = CARTESIAN_POINT ( 'NONE',  ( 8.965967837319999134, -34.65022641339999865, -19.90557312019999969 ) ) ;
#14374 = FACE_OUTER_BOUND ( 'NONE', #19924, .T. ) ;
#14375 = CARTESIAN_POINT ( 'NONE',  ( 40.00000000000000000, -73.50000000000000000, 2.065014825799999939E-15 ) ) ;
#14376 = ORIENTED_EDGE ( 'NONE', *, *, #23338, .T. ) ;
#14377 = FACE_OUTER_BOUND ( 'NONE', #12570, .T. ) ;
#14378 = VERTEX_POINT ( 'NONE', #6178 ) ;
#14379 = CARTESIAN_POINT ( 'NONE',  ( -1.156101949690000019, -58.35063071660000134, -23.44148674059999848 ) ) ;
#14380 = AXIS2_PLACEMENT_3D ( 'NONE', #1729, #10570, #28372 ) ;
#14381 = DIRECTION ( 'NONE',  ( 0.000000000000000000, 1.000000000000000000, 0.000000000000000000 ) ) ;
#14382 = CARTESIAN_POINT ( 'NONE',  ( -28.44519471329999760, -92.55031878709998239, 3.282258450510000092 ) ) ;
#14383 = DIRECTION ( 'NONE',  ( 0.4794255386042041711, 0.000000000000000000, 0.8775825618903722036 ) ) ;
#14384 = ORIENTED_EDGE ( 'NONE', *, *, #1633, .F. ) ;
#14386 = EDGE_CURVE ( 'NONE', #13209, #17197, #20904, .T. ) ;
#14385 = AXIS2_PLACEMENT_3D ( 'NONE', #10761, #8878, #31 ) ;
#14387 = AXIS2_PLACEMENT_3D ( 'NONE', #10444, #19222, #21688 ) ;
#14388 = CIRCLE ( 'NONE', #26958, 1.000000000000000444 ) ;
#14389 = CARTESIAN_POINT ( 'NONE',  ( -28.91764959275750257, -93.08494709829881231, 3.257743348587014420 ) ) ;
#14390 = CYLINDRICAL_SURFACE ( 'NONE', #3681, 3.000000000000001332 ) ;
#14391 = ORIENTED_EDGE ( 'NONE', *, *, #7478, .T. ) ;
#14392 = CARTESIAN_POINT ( 'NONE',  ( 7.611151840291949355, -37.24567261342306068, -21.50381023462963270 ) ) ;
#14393 = DIRECTION ( 'NONE',  ( 0.000000000000000000, 1.000000000000000000, 0.000000000000000000 ) ) ;
#14394 = EDGE_CURVE ( 'NONE', #20323, #8116, #13925, .T. ) ;
#14395 = CARTESIAN_POINT ( 'NONE',  ( -3.296126547070000079, -69.13896873960000278, -27.54013567880000224 ) ) ;
#14396 = ORIENTED_EDGE ( 'NONE', *, *, #12465, .F. ) ;
#14397 = DIRECTION ( 'NONE',  ( 0.3799696139668880535, 0.000000000000000000, -0.9249989688977248159 ) ) ;
#14398 = CARTESIAN_POINT ( 'NONE',  ( -15.56430586970000007, -100.7823373549999957, 2.734376720570000252 ) ) ;
#14399 = DIRECTION ( 'NONE',  ( 1.000000000000000000, 0.000000000000000000, 0.000000000000000000 ) ) ;
#14400 = CARTESIAN_POINT ( 'NONE',  ( -20.47698326670000313, -61.75818586239999775, 14.68202960460000028 ) ) ;
#14401 = VERTEX_POINT ( 'NONE', #21920 ) ;
#14402 = CIRCLE ( 'NONE', #11592, 55.50192378860000275 ) ;
#14403 = CARTESIAN_POINT ( 'NONE',  ( -0.5335602090290000321, -52.63293862049999916, -23.18581005440000098 ) ) ;
#14404 = CARTESIAN_POINT ( 'NONE',  ( -2.987826558189999648, -18.62337006899999992, -24.35058490870000014 ) ) ;
#14405 = DIRECTION ( 'NONE',  ( 1.000000000000000000, 0.000000000000000000, 0.000000000000000000 ) ) ;
#14406 = ORIENTED_EDGE ( 'NONE', *, *, #16193, .T. ) ;
#14407 = AXIS2_PLACEMENT_3D ( 'NONE', #24882, #4918, #13794 ) ;
#14408 = AXIS2_PLACEMENT_3D ( 'NONE', #4526, #13405, #22022 ) ;
#14409 = DIRECTION ( 'NONE',  ( 1.000000000000000000, 0.000000000000000000, 0.000000000000000000 ) ) ;
#14410 = CARTESIAN_POINT ( 'NONE',  ( 36.36887067909999871, -79.00000000000000000, -14.85406736540000061 ) ) ;
#14411 = CARTESIAN_POINT ( 'NONE',  ( 19.57843399940000140, -94.59276292389999696, 13.52682119470000011 ) ) ;
#14412 = ORIENTED_EDGE ( 'NONE', *, *, #18953, .T. ) ;
#14413 = UNCERTAINTY_MEASURE_WITH_UNIT (LENGTH_MEASURE( 1.000000000000000082E-05 ), #1808, 'distance_accuracy_value', 'NONE');
#14414 = EDGE_CURVE ( 'NONE', #19113, #21973, #6258, .T. ) ;
#14415 = CARTESIAN_POINT ( 'NONE',  ( 2.220446049249999745E-14, -15.00000000000000000, -31.00000000000000000 ) ) ;
#14416 = ORIENTED_EDGE ( 'NONE', *, *, #1109, .F. ) ;
#14417 = EDGE_CURVE ( 'NONE', #5336, #11019, #10638, .T. ) ;
#14418 = CARTESIAN_POINT ( 'NONE',  ( 46.40078773993090522, -73.62157574275342142, -3.405080668251522003 ) ) ;
#14419 = ORIENTED_EDGE ( 'NONE', *, *, #26187, .F. ) ;
#14420 = CARTESIAN_POINT ( 'NONE',  ( -10.91687328849999794, -19.46548165690000332, 19.14227818649999691 ) ) ;
#14421 = DIRECTION ( 'NONE',  ( 0.9408314849018030168, 0.000000000000000000, -0.3388747807339287377 ) ) ;
#14422 = ORIENTED_EDGE ( 'NONE', *, *, #12389, .F. ) ;
#14423 = DIRECTION ( 'NONE',  ( 1.000000000000000000, 0.000000000000000000, 0.000000000000000000 ) ) ;
#14424 = TOROIDAL_SURFACE ( 'NONE', #12540, 52.35000000000000142, 1.000000000000000000 ) ;
#14425 = EDGE_CURVE ( 'NONE', #27919, #26201, #12499, .T. ) ;
#14426 = VERTEX_POINT ( 'NONE', #21447 ) ;
#14427 = CARTESIAN_POINT ( 'NONE',  ( 38.71640952649999434, -73.65708014139998738, 7.135466514619999145 ) ) ;
#14428 = CARTESIAN_POINT ( 'NONE',  ( 25.57115952125134939, -69.12177585505048683, -8.648957911665412723 ) ) ;
#14429 = FACE_OUTER_BOUND ( 'NONE', #13540, .T. ) ;
#14430 = CARTESIAN_POINT ( 'NONE',  ( -13.55845375110000006, -93.00000046469999404, 27.19007892950000027 ) ) ;
#14431 = VERTEX_POINT ( 'NONE', #1924 ) ;
#14432 = DIRECTION ( 'NONE',  ( 0.000000000000000000, 0.000000000000000000, -1.000000000000000000 ) ) ;
#14433 = CARTESIAN_POINT ( 'NONE',  ( 15.76736775957732206, -101.6407018583229274, 2.752252931809222147 ) ) ;
#14434 = CARTESIAN_POINT ( 'NONE',  ( 0.000000000000000000, -17.50000000000000000, 0.000000000000000000 ) ) ;
#14435 = CARTESIAN_POINT ( 'NONE',  ( -9.476764215410000247, -84.00000000000000000, 38.08875739639999836 ) ) ;
#14436 = ORIENTED_EDGE ( 'NONE', *, *, #6399, .T. ) ;
#14437 = CARTESIAN_POINT ( 'NONE',  ( -1.441012333810000046, -80.05618323510000778, 47.15972982670000135 ) ) ;
#14438 = CARTESIAN_POINT ( 'NONE',  ( -1.776356839399999804E-15, -79.50000000000000000, 47.25000000000000000 ) ) ;
#14439 = ORIENTED_EDGE ( 'NONE', *, *, #27562, .F. ) ;
#14440 = CARTESIAN_POINT ( 'NONE',  ( 0.000000000000000000, -84.75000000000000000, 0.000000000000000000 ) ) ;
#14441 = CARTESIAN_POINT ( 'NONE',  ( -36.23922253580000330, -74.00000000000000000, -26.33972759919999973 ) ) ;
#14442 = CARTESIAN_POINT ( 'NONE',  ( 10.33697414329999908, -72.00000000000000000, -28.69893982729999848 ) ) ;
#14443 = CARTESIAN_POINT ( 'NONE',  ( 30.97095762050000189, -72.31416070160000231, -20.30102759929999934 ) ) ;
#14444 = APPLICATION_CONTEXT ( 'automotive_design' ) ;
#14445 = CARTESIAN_POINT ( 'NONE',  ( -14.37578563377381435, -74.06475120341723084, 36.25117000458550365 ) ) ;
#14446 = AXIS2_PLACEMENT_3D ( 'NONE', #6946, #3574, #5614 ) ;
#14447 = SHAPE_REPRESENTATION_RELATIONSHIP ( 'NONE' , 'NONE' ,  #5912, #25525 ) ;
#14448 = ORIENTED_EDGE ( 'NONE', *, *, #16156, .T. ) ;
#14449 = ADVANCED_FACE ( 'NONE', ( #19676 ), #10345, .T. ) ;
#14450 = B_SPLINE_CURVE_WITH_KNOTS ( 'NONE', 5,
 ( #1074, #16621, #6099, #3645, #17042, #8282 ),
 .UNSPECIFIED., .F., .F.,
 ( 6, 6 ),
 ( 0.000000000000000000, 1.000000000000000000 ),
 .UNSPECIFIED. ) ;
#14451 = CARTESIAN_POINT ( 'NONE',  ( 20.05332756480000000, -35.50840382379999483, -8.956869086990002060 ) ) ;
#14452 = CARTESIAN_POINT ( 'NONE',  ( 27.05591625959999647, -93.00000000000000000, 12.64646362319999895 ) ) ;
#14453 = CARTESIAN_POINT ( 'NONE',  ( 20.34791740889999900, -35.98209074209999159, -9.112674168019999854 ) ) ;
#14454 = CARTESIAN_POINT ( 'NONE',  ( -21.69554430422256175, -79.50000022090000584, -32.70900267937481942 ) ) ;
#14455 = ORIENTED_EDGE ( 'NONE', *, *, #24505, .T. ) ;
#14456 = CARTESIAN_POINT ( 'NONE',  ( -13.14229091329999832, -100.8869817940000075, -8.528547626079999944 ) ) ;
#14457 = DIRECTION ( 'NONE',  ( 0.000000000000000000, -1.000000000000000000, 0.000000000000000000 ) ) ;
#14458 = CARTESIAN_POINT ( 'NONE',  ( 0.000000000000000000, -21.50000000000000000, 0.000000000000000000 ) ) ;
#14459 = EDGE_CURVE ( 'NONE', #9863, #77, #7435, .T. ) ;
#14460 = DIRECTION ( 'NONE',  ( -0.9993816408608721114, 0.000000000000000000, 0.03516156865429537204 ) ) ;
#14461 = CARTESIAN_POINT ( 'NONE',  ( -13.55845375110000006, -93.00000046469999404, 27.19007892950000027 ) ) ;
#14462 = CARTESIAN_POINT ( 'NONE',  ( 7.218659600080000516, -101.2530993709999905, 13.36960380829999906 ) ) ;
#14463 = VERTEX_POINT ( 'NONE', #11048 ) ;
#14464 = LINE ( 'NONE', #25274, #6757 ) ;
#14465 = VECTOR ( 'NONE', #15295, 1000.000000000000000 ) ;
#14466 = CARTESIAN_POINT ( 'NONE',  ( -27.05658671429999984, -93.01085527740001169, -4.217795407459999701 ) ) ;
#14467 = CARTESIAN_POINT ( 'NONE',  ( 10.55213757090000115, -95.76596938280000870, -20.15016797799999893 ) ) ;
#14468 = ORIENTED_EDGE ( 'NONE', *, *, #21838, .F. ) ;
#14469 = CARTESIAN_POINT ( 'NONE',  ( 18.85230044180000064, -18.50000000000000000, -8.028472989679999117 ) ) ;
#14470 = CARTESIAN_POINT ( 'NONE',  ( -41.61797703107799151, -63.05366661936065498, -2.876041293750446481 ) ) ;
#14471 = CARTESIAN_POINT ( 'NONE',  ( -18.11129459295214517, -92.54383083955173106, 24.54040303195527173 ) ) ;
#14472 = CARTESIAN_POINT ( 'NONE',  ( -1.000575989186441417, -74.24539519982145919, 47.18104523406701389 ) ) ;
#14473 = EDGE_CURVE ( 'NONE', #6167, #17563, #6003, .T. ) ;
#14474 = CARTESIAN_POINT ( 'NONE',  ( 21.47211211410000331, -36.57019168810000309, -7.156454249520000310 ) ) ;
#14475 = CARTESIAN_POINT ( 'NONE',  ( 13.82853744383082351, -98.09459741723881621, 15.06191675743312608 ) ) ;
#14476 = CARTESIAN_POINT ( 'NONE',  ( -11.17082021589999918, -34.59963798429999571, -22.14893711949999755 ) ) ;
#14477 = ORIENTED_EDGE ( 'NONE', *, *, #22923, .F. ) ;
#14478 = CARTESIAN_POINT ( 'NONE',  ( 6.715091161579999302, -101.1180794200000008, 13.99142704490000177 ) ) ;
#14479 = CARTESIAN_POINT ( 'NONE',  ( -22.13232332860000184, -74.50000000000000000, -32.73892504640000567 ) ) ;
#14480 = CIRCLE ( 'NONE', #10707, 3.000000000000002665 ) ;
#14481 = AXIS2_PLACEMENT_3D ( 'NONE', #5358, #18765, #25180 ) ;
#14482 = AXIS2_PLACEMENT_3D ( 'NONE', #22311, #26838, #6869 ) ;
#14483 = CARTESIAN_POINT ( 'NONE',  ( -11.47583862359999962, -94.67274582490000512, -20.72942797039999974 ) ) ;
#14484 = CARTESIAN_POINT ( 'NONE',  ( 20.39306988279999899, -34.78953926309999645, -8.798269974460000142 ) ) ;
#14485 = CARTESIAN_POINT ( 'NONE',  ( -26.60903970598167589, -19.40000000000000213, -48.70752046822583736 ) ) ;
#14486 = DIRECTION ( 'NONE',  ( 0.000000000000000000, 1.000000000000000000, 0.000000000000000000 ) ) ;
#14487 = CARTESIAN_POINT ( 'NONE',  ( 0.000000000000000000, -80.50000000000000000, 0.000000000000000000 ) ) ;
#14488 = ORIENTED_EDGE ( 'NONE', *, *, #7673, .F. ) ;
#14489 = DIRECTION ( 'NONE',  ( 0.000000000000000000, 1.000000000000000000, 0.000000000000000000 ) ) ;
#14490 = DIRECTION ( 'NONE',  ( 0.000000000000000000, -1.000000000000000000, 0.000000000000000000 ) ) ;
#14491 = ORIENTED_EDGE ( 'NONE', *, *, #13382, .T. ) ;
#14492 = CARTESIAN_POINT ( 'NONE',  ( -13.18754275750000104, -69.02891040180000459, -23.50545369980000032 ) ) ;
#14493 = CARTESIAN_POINT ( 'NONE',  ( 0.5331203104650162894, -101.0610180774177138, -16.44819632410123589 ) ) ;
#14494 = CARTESIAN_POINT ( 'NONE',  ( -11.93462531391737791, -19.46927944529031151, 19.09349998647691393 ) ) ;
#14495 = CARTESIAN_POINT ( 'NONE',  ( 6.038481244350000665, -100.8023006570000035, 14.57509264930000015 ) ) ;
#14496 = CARTESIAN_POINT ( 'NONE',  ( 13.58333658430973756, -92.61393927545320537, 27.30833405384957757 ) ) ;
#14497 = AXIS2_PLACEMENT_3D ( 'NONE', #19644, #23888, #26359 ) ;
#14498 = CARTESIAN_POINT ( 'NONE',  ( 15.67714813079999736, -101.1412505549999992, 3.951871014550000005 ) ) ;
#14499 = CARTESIAN_POINT ( 'NONE',  ( 23.62363097839999782, -73.01595982080000624, -30.63067135909999905 ) ) ;
#14500 = VECTOR ( 'NONE', #18446, 1000.000000000000000 ) ;
#14501 = CARTESIAN_POINT ( 'NONE',  ( 28.69894246159999796, -72.00000000000000000, -10.33698060819999931 ) ) ;
#14502 = EDGE_CURVE ( 'NONE', #87, #3592, #22300, .T. ) ;
#14503 = DIRECTION ( 'NONE',  ( 0.000000000000000000, 0.000000000000000000, 1.000000000000000000 ) ) ;
#14504 = CARTESIAN_POINT ( 'NONE',  ( -0.2819570041572871943, -95.90275867845988955, 23.35952539960409169 ) ) ;
#14505 = FACE_OUTER_BOUND ( 'NONE', #9039, .T. ) ;
#14506 = CARTESIAN_POINT ( 'NONE',  ( -41.58361464086270587, -63.05597747387622576, 2.885209034396454708 ) ) ;
#14507 = ORIENTED_EDGE ( 'NONE', *, *, #21578, .T. ) ;
#14508 = EDGE_CURVE ( 'NONE', #22866, #7412, #16245, .T. ) ;
#14509 = DIRECTION ( 'NONE',  ( 0.000000000000000000, 1.000000000000000000, 0.000000000000000000 ) ) ;
#14510 = ORIENTED_EDGE ( 'NONE', *, *, #7639, .T. ) ;
#14511 = ADVANCED_FACE ( 'NONE', ( #187 ), #11508, .T. ) ;
#14512 = EDGE_CURVE ( 'NONE', #13967, #23133, #18233, .T. ) ;
#14513 = DIRECTION ( 'NONE',  ( 0.9952295494196653491, 0.000000000000000000, -0.09756097560976997873 ) ) ;
#14514 = B_SPLINE_CURVE_WITH_KNOTS ( 'NONE', 3,
 ( #24271, #13185, #28770, #26605, #18007, #552 ),
 .UNSPECIFIED., .F., .F.,
 ( 4, 2, 4 ),
 ( 0.000000000000000000, 0.5000000000000000000, 1.000000000000000000 ),
 .UNSPECIFIED. ) ;
#14515 = FACE_OUTER_BOUND ( 'NONE', #10768, .T. ) ;
#14516 = VECTOR ( 'NONE', #7177, 1000.000000000000114 ) ;
#14517 = CARTESIAN_POINT ( 'NONE',  ( 26.60903970598167589, -19.40000000000000213, 48.70752046822583736 ) ) ;
#14518 = DIRECTION ( 'NONE',  ( 0.000000000000000000, 1.000000000000000000, 0.000000000000000000 ) ) ;
#14519 = ORIENTED_EDGE ( 'NONE', *, *, #8628, .T. ) ;
#14520 = LINE ( 'NONE', #18775, #6186 ) ;
#14521 = CARTESIAN_POINT ( 'NONE',  ( 9.107729735749998667, -35.83389485320000034, -19.55231199680000387 ) ) ;
#14522 = CARTESIAN_POINT ( 'NONE',  ( 21.84994998139999822, -44.93330283399999558, -6.931585813899999948 ) ) ;
#14523 = CARTESIAN_POINT ( 'NONE',  ( 26.62478236560000155, -92.85282594270000800, -10.14810411050000027 ) ) ;
#14524 = CARTESIAN_POINT ( 'NONE',  ( -16.01759400379999931, -69.30633957129998635, 23.18138418170000037 ) ) ;
#14525 = VERTEX_POINT ( 'NONE', #20119 ) ;
#14526 = CARTESIAN_POINT ( 'NONE',  ( -14.90965166979999879, -101.1292387920000095, 4.262398319349999909 ) ) ;
#14527 = CARTESIAN_POINT ( 'NONE',  ( -16.50888742379999741, -100.1721652129999995, 2.973064930670000106 ) ) ;
#14528 = CARTESIAN_POINT ( 'NONE',  ( -32.83566817730000054, -74.50000000000000000, -22.22906645950000026 ) ) ;
#14529 = CARTESIAN_POINT ( 'NONE',  ( -6.275498632237177077, -101.4628082233731732, 14.68909490417829211 ) ) ;
#14530 = ORIENTED_EDGE ( 'NONE', *, *, #3378, .T. ) ;
#14531 = DIRECTION ( 'NONE',  ( -1.000000000000000000, 0.000000000000000000, 0.000000000000000000 ) ) ;
#14532 = AXIS2_PLACEMENT_3D ( 'NONE', #22485, #20437, #22332 ) ;
#14533 = CARTESIAN_POINT ( 'NONE',  ( -3.035021987659999976, -18.62259217289999924, -24.02173570430000282 ) ) ;
#14534 = CARTESIAN_POINT ( 'NONE',  ( 36.60600030368150470, -74.15649605208299988, -14.28714990587511124 ) ) ;
#14535 = ORIENTED_EDGE ( 'NONE', *, *, #15956, .F. ) ;
#14536 = EDGE_CURVE ( 'NONE', #16695, #13357, #23254, .T. ) ;
#14537 = CARTESIAN_POINT ( 'NONE',  ( 0.000000000000000000, -19.00000000000000000, 0.000000000000000000 ) ) ;
#14538 = FACE_OUTER_BOUND ( 'NONE', #21234, .T. ) ;
#14539 = CARTESIAN_POINT ( 'NONE',  ( 36.54355158469999765, -79.59555342380001264, -14.63615714969999893 ) ) ;
#14540 = CARTESIAN_POINT ( 'NONE',  ( 19.89027988503224265, -94.80026864431334843, 14.17835479305916202 ) ) ;
#14541 = ORIENTED_EDGE ( 'NONE', *, *, #12300, .F. ) ;
#14542 = ADVANCED_FACE ( 'NONE', ( #2355 ), #1383, .F. ) ;
#14543 = EDGE_CURVE ( 'NONE', #8365, #23467, #21833, .T. ) ;
#14544 = B_SPLINE_SURFACE_WITH_KNOTS ( 'NONE', 5, 5, ( 
 ( #11766, #18781, #11914, #20966, #13958, #3193 ),
 ( #2754, #2905, #7711, #16579, #25471, #13808 ),
 ( #5506, #18485, #5371, #11610, #16437, #27376 ),
 ( #9434, #14395, #5072, #7417, #23146, #23285 ),
 ( #20818, #20523, #591, #18342, #25341, #12051 ),
 ( #7269, #16135, #20676, #25038, #22864, #880 ),
 ( #737, #18632, #16282, #9722, #27529, #1027 ),
 ( #9585, #14254, #25197, #5226, #14110, #23009 ),
 ( #3059, #7574, #5024, #13315, #15497, #9389 ) ),
 .UNSPECIFIED., .F., .F., .F.,
 ( 6, 3, 6 ),
 ( 6, 6 ),
 ( 41.71218049600000199, 49.83411874629999971, 53.81665561330000003 ),
 ( 0.000000000000000000, 2.000000000000000000 ),
 .UNSPECIFIED. ) ;
#14545 = CARTESIAN_POINT ( 'NONE',  ( 7.146599689825861468, -99.96200787832681556, 15.79248128130144835 ) ) ;
#14546 = CARTESIAN_POINT ( 'NONE',  ( -1.226789154321535680, -79.95994320750210704, 47.14707426476502405 ) ) ;
#14547 = ORIENTED_EDGE ( 'NONE', *, *, #2594, .F. ) ;
#14548 = CARTESIAN_POINT ( 'NONE',  ( -18.30346299744424954, -98.29032200027317856, 5.174493964400173951 ) ) ;
#14549 = VERTEX_POINT ( 'NONE', #13111 ) ;
#14550 = AXIS2_PLACEMENT_3D ( 'NONE', #8837, #4634, #293 ) ;
#14551 = CARTESIAN_POINT ( 'NONE',  ( 28.34114226579999851, -92.53610955750001210, 8.350028085840000003 ) ) ;
#14552 = CARTESIAN_POINT ( 'NONE',  ( -6.091317750690000032, -101.3957169669999985, 14.78042619649999878 ) ) ;
#14553 = ORIENTED_EDGE ( 'NONE', *, *, #11802, .F. ) ;
#14554 = CIRCLE ( 'NONE', #18296, 0.9999999999999997780 ) ;
#14555 = CARTESIAN_POINT ( 'NONE',  ( 27.49607050420000220, -19.50000000000000000, 1.934818144049999855 ) ) ;
#14556 = DIRECTION ( 'NONE',  ( 1.000000000000000000, 0.000000000000000000, 0.000000000000000000 ) ) ;
#14557 = ORIENTED_EDGE ( 'NONE', *, *, #26819, .T. ) ;
#14558 = CARTESIAN_POINT ( 'NONE',  ( 23.35417726369999869, -57.47855601759999900, -0.5711878298099999363 ) ) ;
#14559 = LINE ( 'NONE', #18673, #12039 ) ;
#14560 = CARTESIAN_POINT ( 'NONE',  ( 47.16844854119278807, -79.40106950755198056, -1.389656841691803590 ) ) ;
#14561 = ORIENTED_EDGE ( 'NONE', *, *, #17105, .F. ) ;
#14562 = CARTESIAN_POINT ( 'NONE',  ( -18.81329003759999807, -96.93384555689999615, -9.961933200989999904 ) ) ;
#14563 = CARTESIAN_POINT ( 'NONE',  ( 8.965966766827932588, -34.65022632772699751, -19.90557426916371497 ) ) ;
#14564 = CARTESIAN_POINT ( 'NONE',  ( 8.986258419809999509, -35.50000000000000000, -19.49544308430000328 ) ) ;
#14565 = DIRECTION ( 'NONE',  ( -0.7071067811865475727, 0.000000000000000000, -0.7071067811865475727 ) ) ;
#14566 = CARTESIAN_POINT ( 'NONE',  ( -2.567353809430000133, -52.57401960349999825, -24.80239345940000106 ) ) ;
#14567 = B_SPLINE_CURVE_WITH_KNOTS ( 'NONE', 3,
 ( #22413, #5062, #22258, #15835, #9131, #22566, #6674, #13501, #9280, #4630, #18180, #27077, #13800, #13660, #15983, #22705, #13951, #24746, #26790, #8985, #6972, #2460 ),
 .UNSPECIFIED., .F., .F.,
 ( 4, 2, 1, 1, 1, 2, 2, 2, 1, 1, 1, 2, 2, 4 ),
 ( 0.000000000000000000, 0.1250000000000226208, 0.1875000000000338340, 0.2187500000000397460, 0.2343750000000427991, 0.2421875000000443257, 0.2500000000000458522, 0.3750000000000830447, 0.4375000000000992539, 0.4687500000001053602, 0.4843750000001084133, 0.4921875000001078027, 0.5000000000001071365, 1.000000000000000000 ),
 .UNSPECIFIED. ) ;
#14568 = EDGE_CURVE ( 'NONE', #9504, #4936, #2768, .T. ) ;
#14569 = CARTESIAN_POINT ( 'NONE',  ( -2.675072049550000219E-13, -79.50000000000000000, 47.25000000000000000 ) ) ;
#14570 = CYLINDRICAL_SURFACE ( 'NONE', #27072, 0.1999999999999996780 ) ;
#14571 = ORIENTED_EDGE ( 'NONE', *, *, #8516, .F. ) ;
#14572 = EDGE_CURVE ( 'NONE', #2880, #11154, #22776, .T. ) ;
#14573 = CARTESIAN_POINT ( 'NONE',  ( 36.24656994149999889, -79.00000000000000000, -15.05817610060000078 ) ) ;
#14574 = DIRECTION ( 'NONE',  ( 0.4794255386042036160, 0.000000000000000000, 0.8775825618903723147 ) ) ;
#14575 = CARTESIAN_POINT ( 'NONE',  ( 0.000000000000000000, -6.000000000000000000, 0.000000000000000000 ) ) ;
#14576 = CARTESIAN_POINT ( 'NONE',  ( 32.20446920490000053, -74.00073021550001329, -21.99457402419999852 ) ) ;
#14577 = ADVANCED_FACE ( 'NONE', ( #13557 ), #11975, .F. ) ;
#14578 = CARTESIAN_POINT ( 'NONE',  ( -14.20278481966783168, -74.02954850625619088, 36.23557363773064566 ) ) ;
#14579 = AXIS2_PLACEMENT_3D ( 'NONE', #23005, #877, #5367 ) ;
#14580 = EDGE_CURVE ( 'NONE', #13695, #2130, #27439, .T. ) ;
#14581 = DIRECTION ( 'NONE',  ( 1.000000000000000000, 0.000000000000000000, 0.000000000000000000 ) ) ;
#14582 = VERTEX_POINT ( 'NONE', #14154 ) ;
#14583 = CARTESIAN_POINT ( 'NONE',  ( 9.698193454340000130, -36.00000000010000178, -20.58262106160000116 ) ) ;
#14584 = CARTESIAN_POINT ( 'NONE',  ( -40.14660266887646856, -74.07739338315893463, -7.248706349658688097 ) ) ;
#14585 = CIRCLE ( 'NONE', #6694, 4.999999999999999112 ) ;
#14586 = CARTESIAN_POINT ( 'NONE',  ( 21.24969070070000043, -36.48513442969999687, -8.723503615720002102 ) ) ;
#14587 = CARTESIAN_POINT ( 'NONE',  ( 6.998258279363821721, -92.73901256244006674, -28.68106635605278498 ) ) ;
#14588 = ORIENTED_EDGE ( 'NONE', *, *, #4208, .T. ) ;
#14589 = CARTESIAN_POINT ( 'NONE',  ( -13.01247235640000000, -101.5369810359999860, -9.310661355180000598 ) ) ;
#14590 = DIRECTION ( 'NONE',  ( -5.788992577199999305E-17, 0.000000000000000000, 1.000000000000000000 ) ) ;
#14591 = CARTESIAN_POINT ( 'NONE',  ( -7.888947276530000607, -100.3517545579999961, 14.77732780220000031 ) ) ;
#14592 = CARTESIAN_POINT ( 'NONE',  ( -0.2283560652399999891, -93.01584738779999384, 26.42460660340000089 ) ) ;
#14593 = LINE ( 'NONE', #2980, #646 ) ;
#14594 = VECTOR ( 'NONE', #15992, 1000.000000000000000 ) ;
#14595 = CARTESIAN_POINT ( 'NONE',  ( 7.273173879219999804, -101.1845941320000009, 13.44072509259999926 ) ) ;
#14596 = ORIENTED_EDGE ( 'NONE', *, *, #15609, .F. ) ;
#14597 = DIRECTION ( 'NONE',  ( 0.4794255386042041156, 0.000000000000000000, 0.8775825618903722036 ) ) ;
#14598 = DIRECTION ( 'NONE',  ( 1.000000000000000000, 0.000000000000000000, 0.000000000000000000 ) ) ;
#14599 = CARTESIAN_POINT ( 'NONE',  ( 26.38387136229999896, -71.18862645909999287, 10.78376531940000049 ) ) ;
#14600 = DIRECTION ( 'NONE',  ( 0.4794255386042036160, 0.000000000000000000, 0.8775825618903723147 ) ) ;
#14601 = ORIENTED_EDGE ( 'NONE', *, *, #24534, .F. ) ;
#14602 = CARTESIAN_POINT ( 'NONE',  ( 20.63161943080000071, -19.46510050319999863, -7.734358783100000245 ) ) ;
#14603 = CARTESIAN_POINT ( 'NONE',  ( 12.02399834240000054, -101.4254868729999970, -10.50861765550000015 ) ) ;
#14604 = CARTESIAN_POINT ( 'NONE',  ( -14.67203031310000050, -74.27627443250000283, 36.35843490820000312 ) ) ;
#14605 = CARTESIAN_POINT ( 'NONE',  ( -3.883346862689999845, -9.250000000000000000, -7.108418751309999450 ) ) ;
#14606 = CARTESIAN_POINT ( 'NONE',  ( -18.15215127219713764, -92.53708507728566701, 24.51021966657489060 ) ) ;
#14607 = ORIENTED_EDGE ( 'NONE', *, *, #15360, .F. ) ;
#14608 = EDGE_CURVE ( 'NONE', #26756, #5668, #15273, .T. ) ;
#14609 = AXIS2_PLACEMENT_3D ( 'NONE', #23332, #14977, #24175 ) ;
#14610 = CARTESIAN_POINT ( 'NONE',  ( 14.28941763439999946, -93.00000000000000000, -3.575252188409999921 ) ) ;
#14611 = AXIS2_PLACEMENT_3D ( 'NONE', #18360, #611, #22733 ) ;
#14612 = ADVANCED_FACE ( 'NONE', ( #18821 ), #23189, .F. ) ;
#14613 = CARTESIAN_POINT ( 'NONE',  ( -0.1699704075889999777, -101.1848541609999899, -15.28111812279999882 ) ) ;
#14614 = CARTESIAN_POINT ( 'NONE',  ( 7.727580379730000004, -65.07443080049999651, -23.93312984690000178 ) ) ;
#14615 = CARTESIAN_POINT ( 'NONE',  ( 15.41249585359999941, -101.0535396030000044, 2.362963133130000060 ) ) ;
#14616 = CARTESIAN_POINT ( 'NONE',  ( 22.30996026260000065, -58.68498324060000471, 10.16715434780000038 ) ) ;
#14617 = ORIENTED_EDGE ( 'NONE', *, *, #17692, .T. ) ;
#14618 = B_SPLINE_CURVE_WITH_KNOTS ( 'NONE', 5,
 ( #15587, #7305, #11648, #24486, #17789, #18077 ),
 .UNSPECIFIED., .F., .F.,
 ( 6, 6 ),
 ( 0.000000000000000000, 1.000000000000000000 ),
 .UNSPECIFIED. ) ;
#14619 = CARTESIAN_POINT ( 'NONE',  ( 6.555554406829999792, -100.6809449770000100, 15.07230642660000086 ) ) ;
#14620 = CARTESIAN_POINT ( 'NONE',  ( -27.68682485439999752, -24.80000000000000071, -50.68039294919999804 ) ) ;
#14621 = CARTESIAN_POINT ( 'NONE',  ( -11.43284111409999859, -94.65020208389999823, -20.93784837230000306 ) ) ;
#14622 = CARTESIAN_POINT ( 'NONE',  ( 7.836711220800001598, -35.70895110779999726, -21.34303704659999568 ) ) ;
#14623 = CARTESIAN_POINT ( 'NONE',  ( 7.246150394359973212, -73.82038814068835109, 39.74699101863826201 ) ) ;
#14624 = TOROIDAL_SURFACE ( 'NONE', #12309, 43.34897771020000334, 20.00000000000000000 ) ;
#14625 = CARTESIAN_POINT ( 'NONE',  ( -7.879418878250000091, -99.92967428129999519, 15.46932493210000104 ) ) ;
#14626 = DIRECTION ( 'NONE',  ( -0.7975023596669910120, 0.000000000000000000, -0.6033158263509930119 ) ) ;
#14627 = CARTESIAN_POINT ( 'NONE',  ( 8.080976620399999533, -94.09272382160000348, -24.58537356260000095 ) ) ;
#14628 = EDGE_CURVE ( 'NONE', #26186, #26809, #5123, .T. ) ;
#14629 = CARTESIAN_POINT ( 'NONE',  ( 19.14378155729999875, -25.56710285120000137, -9.006608812259999652 ) ) ;
#14630 = DIRECTION ( 'NONE',  ( 0.000000000000000000, 1.000000000000000000, 0.000000000000000000 ) ) ;
#14631 = ORIENTED_EDGE ( 'NONE', *, *, #14301, .F. ) ;
#14632 = VECTOR ( 'NONE', #17975, 1000.000000000000000 ) ;
#14633 = CARTESIAN_POINT ( 'NONE',  ( 20.33566493080000015, -36.00000000000000000, -9.885503730140001721 ) ) ;
#14634 = B_SPLINE_CURVE_WITH_KNOTS ( 'NONE', 3,
 ( #8739, #13116, #19540, #6134 ),
 .UNSPECIFIED., .F., .F.,
 ( 4, 4 ),
 ( 0.000000000000000000, 1.000000000000000000 ),
 .UNSPECIFIED. ) ;
#14635 = CARTESIAN_POINT ( 'NONE',  ( 40.00000000000000000, -73.50000000000000000, 2.065014825799999939E-15 ) ) ;
#14636 = VERTEX_POINT ( 'NONE', #27710 ) ;
#14637 = CARTESIAN_POINT ( 'NONE',  ( 25.33520153630000138, -65.80271596200000772, -10.35056873939999988 ) ) ;
#14638 = CARTESIAN_POINT ( 'NONE',  ( 0.4072779472236851550, -101.3038909013372262, -16.26179699871198636 ) ) ;
#14639 = CARTESIAN_POINT ( 'NONE',  ( -40.00000000000000000, -73.50000000000000000, 3.397282455350000038E-15 ) ) ;
#14640 = CARTESIAN_POINT ( 'NONE',  ( -13.12430501772102254, -92.94830743985350807, -23.71755625844523863 ) ) ;
#14641 = CARTESIAN_POINT ( 'NONE',  ( 21.89558901659999890, -73.74042638279999551, -31.74625209310000429 ) ) ;
#14642 = EDGE_CURVE ( 'NONE', #8148, #20809, #479, .T. ) ;
#14643 = ADVANCED_FACE ( 'NONE', ( #18386 ), #26859, .T. ) ;
#14644 = CARTESIAN_POINT ( 'NONE',  ( -22.23253203089999985, -69.48726973570001064, 15.83344364000000049 ) ) ;
#14645 = CIRCLE ( 'NONE', #17918, 3.750000000000000000 ) ;
#14646 = CARTESIAN_POINT ( 'NONE',  ( 11.43994069400000058, -100.8816835080000089, -10.88980376029999952 ) ) ;
#14647 = CARTESIAN_POINT ( 'NONE',  ( -12.05063396289999922, -64.89165752090001149, -22.22490323269999735 ) ) ;
#14648 = CARTESIAN_POINT ( 'NONE',  ( 16.83483077069999823, -99.92967571559999840, 4.239603657359999112 ) ) ;
#14649 = ORIENTED_EDGE ( 'NONE', *, *, #3278, .F. ) ;
#14650 = CARTESIAN_POINT ( 'NONE',  ( 9.457230477735794949, -35.99973515773508126, -20.00996444815637432 ) ) ;
#14651 = EDGE_CURVE ( 'NONE', #24358, #27117, #20459, .T. ) ;
#14652 = CIRCLE ( 'NONE', #21181, 2.000000000000001332 ) ;
#14653 = ORIENTED_EDGE ( 'NONE', *, *, #26485, .T. ) ;
#14654 = CYLINDRICAL_SURFACE ( 'NONE', #16838, 1.000000000000000888 ) ;
#14655 = CARTESIAN_POINT ( 'NONE',  ( -2.530235925970000022, -63.52052399810000338, -25.57870722859999901 ) ) ;
#14656 = CARTESIAN_POINT ( 'NONE',  ( 33.25000000000000000, -69.50000000000000000, -1.707239799929999782E-15 ) ) ;
#14657 = FACE_OUTER_BOUND ( 'NONE', #1312, .T. ) ;
#14658 = EDGE_CURVE ( 'NONE', #22615, #23918, #13452, .T. ) ;
#14659 = AXIS2_PLACEMENT_3D ( 'NONE', #20399, #619, #16164 ) ;
#14660 = VERTEX_POINT ( 'NONE', #28112 ) ;
#14661 = CARTESIAN_POINT ( 'NONE',  ( -7.498737045662836387, -73.99999999999910472, 38.65106196168373032 ) ) ;
#14662 = EDGE_CURVE ( 'NONE', #21398, #5069, #16993, .T. ) ;
#14663 = ORIENTED_EDGE ( 'NONE', *, *, #20609, .T. ) ;
#14664 = DIRECTION ( 'NONE',  ( 0.4692400087391608854, 0.000000000000000000, -0.8830706733883039172 ) ) ;
#14665 = CARTESIAN_POINT ( 'NONE',  ( 9.151216319970000512, -35.87888623290000112, -19.56023227720000079 ) ) ;
#14666 = ADVANCED_FACE ( 'NONE', ( #5949 ), #7102, .T. ) ;
#14667 = CARTESIAN_POINT ( 'NONE',  ( 38.79561088300408045, -74.00013394014689538, 7.600490370444946464 ) ) ;
#14668 = VERTEX_POINT ( 'NONE', #19365 ) ;
#14669 = CARTESIAN_POINT ( 'NONE',  ( -15.40337430839999833, -101.5317003319999998, 4.643717924509999762 ) ) ;
#14670 = CARTESIAN_POINT ( 'NONE',  ( -16.72188147059999963, -99.89426761010000178, 2.874729616160000223 ) ) ;
#14671 = CARTESIAN_POINT ( 'NONE',  ( -32.67765636376323357, -74.21958180435098029, -22.19105059018374249 ) ) ;
#14672 = CARTESIAN_POINT ( 'NONE',  ( 36.34100412979999817, -74.29447080869999809, -14.83252444919999924 ) ) ;
#14673 = ORIENTED_EDGE ( 'NONE', *, *, #27291, .F. ) ;
#14674 = CARTESIAN_POINT ( 'NONE',  ( 20.42065948455764257, -98.07566645793311011, -1.447915294044073375 ) ) ;
#14675 = LINE ( 'NONE', #22765, #19490 ) ;
#14676 = CARTESIAN_POINT ( 'NONE',  ( -3.160010391330000168, -18.50000000000000000, -22.19765357320000376 ) ) ;
#14677 = CARTESIAN_POINT ( 'NONE',  ( -11.77049175740000209, -94.59276292389999696, -20.68200892780000189 ) ) ;
#14678 = ORIENTED_EDGE ( 'NONE', *, *, #22245, .T. ) ;
#14679 = CLOSED_SHELL ( 'NONE', ( #22519, #26991, #6036, #22003, #5902, #17066, #9491, #17163, #25042, #17558, #16054, #23862, #24411, #22990, #19157, #12541, #17660, #14029, #15906, #12616, #14311, #12444, #25086, #13620, #6961, #8605, #25571, #13512, #7260, #13813, #6259, #27606, #28610, #20885, #22926, #13726, #15164, #12712, #28450, #12801, #28580, #533, #4248, #20353, #20949, #15446, #868, #9513, #20138, #23579, #17737, #5541, #1492, #24598, #24033, #21932, #28570, #25157, #19952, #26082, #18648, #8591, #26551, #26299, #1343, #18268, #27428, #15918, #23838, #25294, #1068, #3063, #24248, #20022, #13446, #738, #12548, #28029, #19860, #23240, #28644, #14695, #14944, #20679, #26348, #2823, #16320, #28721, #5561, #5472, #23680, #6218, #14643, #15075, #10249, #13854, #15736, #4661, #1911, #14449, #18578, #25847, #24916, #16318, #18189, #23150, #1539, #15436, #334, #15158, #5447, #10578, #3441, #12386, #28796, #11258, #7935, #21137, #8371, #28034, #25485, #13210, #1097, #16052, #4739, #6585, #27066, #17468, #4204, #12989, #7813, #22317, #27725, #706, #19573, #14060, #18204, #15049, #6365, #15403, #11944, #21290, #26783, #14097, #17742, #18305, #19282, #28091, #10199, #14511, #10164, #17972, #20614, #16916, #28208, #9203, #18676, #19981, #26552, #4787, #3098, #24787, #24851, #9501, #7418, #4126, #10516, #1219, #27266, #9809, #17012, #28584, #2311, #9134, #22213, #1365, #15119, #19271, #11074, #24685, #21324, #18718, #21946, #16647, #20394, #19758, #27316, #4380, #27828, #14132, #1445, #3655, #12451, #1247, #13132, #28269, #8207, #17154, #14321, #12192, #24348, #18067, #15573, #2792, #23534, #14851, #5113, #55, #729, #22653, #18604, #27934, #26193, #12037, #17633, #21972, #9330, #4951, #22715, #11913, #23272, #25348, #23236, #5110, #28508, #27576, #24637, #3773, #25983, #10212, #23851, #10705, #21, #1039, #9930, #4535, #19925, #19856, #24338, #13889, #20342, #3854, #16328, #23682, #3539, #2088, #28062, #11850, #26019, #21675, #9540, #25415, #20504, #21707, #27096, #16938, #24441, #8507, #20100, #25671, #15372, #15355, #5497, #15990, #24474, #23881, #830, #27293, #19184, #27389, #26554, #2581, #10251, #13787, #4495, #10919, #22473, #24012, #5796, #19489, #7066, #21081, #796, #14204, #4779, #1183, #16028, #19571, #11533, #26763, #4543, #17135, #20881, #8862, #25885, #8129, #5695, #15495, #10398, #13183, #10021, #19150, #19343, #25613, #19597, #3316, #5752, #6374, #27431, #18339 ) ) ;
#14680 = CARTESIAN_POINT ( 'NONE',  ( -7.215414233289999757, -84.00000000000000000, 40.70731707320000226 ) ) ;
#14681 = CARTESIAN_POINT ( 'NONE',  ( -31.64302845809999809, -79.50000000000000000, -31.64302845809999809 ) ) ;
#14682 = CARTESIAN_POINT ( 'NONE',  ( 36.24656994149999889, -79.27200282849999269, -15.05817610060000078 ) ) ;
#14683 = EDGE_LOOP ( 'NONE', ( #27152, #4586, #2026, #22031 ) ) ;
#14684 = CARTESIAN_POINT ( 'NONE',  ( -15.00047198269999882, -79.50000000000000000, 39.16845525979999820 ) ) ;
#14685 = CIRCLE ( 'NONE', #20287, 2.000000000000001776 ) ;
#14686 = ORIENTED_EDGE ( 'NONE', *, *, #5734, .F. ) ;
#14687 = CARTESIAN_POINT ( 'NONE',  ( -18.46601579710593555, -98.10212143905430082, 5.492879491436290174 ) ) ;
#14688 = ORIENTED_EDGE ( 'NONE', *, *, #24752, .F. ) ;
#14689 = CARTESIAN_POINT ( 'NONE',  ( 27.34475978920000117, -92.65997674700000175, 9.666848034470000073 ) ) ;
#14690 = CARTESIAN_POINT ( 'NONE',  ( 8.028473304129999377, -18.50000000000000000, -18.85230009969999898 ) ) ;
#14691 = EDGE_LOOP ( 'NONE', ( #16988, #18789, #147, #25426 ) ) ;
#14692 = ADVANCED_FACE ( 'NONE', ( #23595 ), #24147, .F. ) ;
#14693 = CARTESIAN_POINT ( 'NONE',  ( 12.69294339169999830, -100.9137139110000021, -9.125620792290000338 ) ) ;
#14694 = DIRECTION ( 'NONE',  ( 0.000000000000000000, -1.000000000000000000, 0.000000000000000000 ) ) ;
#14695 = ADVANCED_FACE ( 'NONE', ( #1738 ), #12500, .T. ) ;
#14696 = ORIENTED_EDGE ( 'NONE', *, *, #17406, .F. ) ;
#14697 = DIRECTION ( 'NONE',  ( 0.000000000000000000, 1.000000000000000000, 0.000000000000000000 ) ) ;
#14698 = CARTESIAN_POINT ( 'NONE',  ( 9.082471092209999597, -36.23996849139999910, -21.28200090970000247 ) ) ;
#14699 = EDGE_CURVE ( 'NONE', #2955, #14037, #19765, .T. ) ;
#14700 = CARTESIAN_POINT ( 'NONE',  ( 8.171241461239999770E-14, -101.6484611540000031, -6.927791673659999887E-14 ) ) ;
#14701 = CARTESIAN_POINT ( 'NONE',  ( 25.58194701613479083, -68.15800876155556409, 10.86896338428304709 ) ) ;
#14702 = VERTEX_POINT ( 'NONE', #6382 ) ;
#14703 = EDGE_CURVE ( 'NONE', #9479, #7740, #7966, .T. ) ;
#14704 = CARTESIAN_POINT ( 'NONE',  ( 14.62430634820000108, -72.00000000000000000, 26.76961320899999919 ) ) ;
#14705 = CARTESIAN_POINT ( 'NONE',  ( 15.84942546552125009, -101.5703832412493597, 2.583842542799739128 ) ) ;
#14706 = CARTESIAN_POINT ( 'NONE',  ( -20.16709992299999854, -93.01085577540001736, 18.52401656639999672 ) ) ;
#14707 = CARTESIAN_POINT ( 'NONE',  ( 24.17069834520000171, -93.81709628040000837, -8.947401651030000735 ) ) ;
#14708 = ORIENTED_EDGE ( 'NONE', *, *, #15779, .F. ) ;
#14709 = B_SPLINE_CURVE_WITH_KNOTS ( 'NONE', 5,
 ( #25260, #16633, #22930, #27728, #20741, #799 ),
 .UNSPECIFIED., .F., .F.,
 ( 6, 6 ),
 ( 0.000000000000000000, 6.855861996789999857 ),
 .UNSPECIFIED. ) ;
#14710 = CARTESIAN_POINT ( 'NONE',  ( 10.33697414329999908, -72.00000000000000000, -28.69893982729999848 ) ) ;
#14711 = CARTESIAN_POINT ( 'NONE',  ( -19.15417045299999899, -18.86697026210000061, 14.26418949420000004 ) ) ;
#14712 = ORIENTED_EDGE ( 'NONE', *, *, #13008, .F. ) ;
#14713 = DIRECTION ( 'NONE',  ( 0.000000000000000000, 1.000000000000000000, 0.000000000000000000 ) ) ;
#14714 = CARTESIAN_POINT ( 'NONE',  ( 0.000000000000000000, -107.1975888269999899, 0.000000000000000000 ) ) ;
#14715 = CARTESIAN_POINT ( 'NONE',  ( -23.77081188420000046, -93.00000000000000000, -19.11016751280000037 ) ) ;
#14716 = CARTESIAN_POINT ( 'NONE',  ( 28.92477265019999777, -73.91965247389998694, -26.58576722179999763 ) ) ;
#14717 = CARTESIAN_POINT ( 'NONE',  ( -16.56294617018072657, -72.37489744396329172, 23.47174545849500404 ) ) ;
#14718 =( NAMED_UNIT ( * ) SI_UNIT ( $, .STERADIAN. ) SOLID_ANGLE_UNIT ( ) );
#14719 = DIRECTION ( 'NONE',  ( 0.4794255386042000078, 0.000000000000000000, 0.8775825618903743131 ) ) ;
#14720 = ORIENTED_EDGE ( 'NONE', *, *, #941, .T. ) ;
#14721 = DIRECTION ( 'NONE',  ( -0.8775825618903722036, 0.000000000000000000, 0.4794255386042041156 ) ) ;
#14722 = CARTESIAN_POINT ( 'NONE',  ( 21.53016318250000083, -37.05551862909999983, -8.186295007220000031 ) ) ;
#14723 = CARTESIAN_POINT ( 'NONE',  ( 7.206351956654603264, -92.50000267097107098, -28.91782128996979750 ) ) ;
#14724 = VERTEX_POINT ( 'NONE', #22576 ) ;
#14725 = CARTESIAN_POINT ( 'NONE',  ( -12.94585355969999974, -101.6484611540000031, -9.402386697529999893 ) ) ;
#14726 = EDGE_CURVE ( 'NONE', #16034, #13313, #19042, .T. ) ;
#14727 = CARTESIAN_POINT ( 'NONE',  ( -16.08621294430000148, -93.02865658550000205, -23.59017073649999929 ) ) ;
#14728 = CARTESIAN_POINT ( 'NONE',  ( -1.381300513170000022, -100.8816824760000088, -15.73378836020000016 ) ) ;
#14729 = CARTESIAN_POINT ( 'NONE',  ( 7.274533568879999912, -49.11506481659999679, -21.89436955060000045 ) ) ;
#14730 = CARTESIAN_POINT ( 'NONE',  ( 11.67392084060484869, -98.28141829054760592, -16.48995336470006734 ) ) ;
#14731 = ORIENTED_EDGE ( 'NONE', *, *, #3160, .F. ) ;
#14732 = ADVANCED_FACE ( 'NONE', ( #20231 ), #24603, .T. ) ;
#14733 = CARTESIAN_POINT ( 'NONE',  ( 13.05823860876455633, -101.2111896145002419, -9.821097530008616516 ) ) ;
#14734 = CARTESIAN_POINT ( 'NONE',  ( -22.27192494970000070, -94.59276479679999738, -8.381614403809997782 ) ) ;
#14735 = CARTESIAN_POINT ( 'NONE',  ( 39.48689401879786232, -73.68677077069324355, 7.232334316206437741 ) ) ;
#14736 = ORIENTED_EDGE ( 'NONE', *, *, #20948, .T. ) ;
#14737 = CARTESIAN_POINT ( 'NONE',  ( 20.62158124919999835, -19.15810967940000253, -7.730595680639999578 ) ) ;
#14738 = CARTESIAN_POINT ( 'NONE',  ( -14.29690427480000103, -74.09825332389999630, 36.44846386569999908 ) ) ;
#14739 = DIRECTION ( 'NONE',  ( 0.4151946956541399669, 0.5000000000001689759, 0.7600087925152558821 ) ) ;
#14740 = CARTESIAN_POINT ( 'NONE',  ( -18.07483010357461595, -92.55017404142755311, 24.56726588061794203 ) ) ;
#14741 = ORIENTED_EDGE ( 'NONE', *, *, #4229, .T. ) ;
#14742 = DIRECTION ( 'NONE',  ( 0.000000000000000000, -1.000000000000000000, 0.000000000000000000 ) ) ;
#14743 = DIRECTION ( 'NONE',  ( 1.738658080640003812E-17, 0.000000000000000000, -1.000000000000000000 ) ) ;
#14744 = CARTESIAN_POINT ( 'NONE',  ( 26.78710329588840366, -92.73901256241863678, -12.41089373421818465 ) ) ;
#14745 = CARTESIAN_POINT ( 'NONE',  ( -39.64169929219999489, -73.82505177980000610, -7.260629317050000253 ) ) ;
#14746 = CARTESIAN_POINT ( 'NONE',  ( 20.68132854559999956, -58.35623000289999851, 10.95980495770000118 ) ) ;
#14747 = ORIENTED_EDGE ( 'NONE', *, *, #15642, .F. ) ;
#14748 = CARTESIAN_POINT ( 'NONE',  ( 6.364863104659999493, -100.8772072149999985, 14.46207622220000033 ) ) ;
#14749 = CARTESIAN_POINT ( 'NONE',  ( -13.91416830965637885, -92.72284173551921072, -24.03918013284343402 ) ) ;
#14750 = B_SPLINE_CURVE_WITH_KNOTS ( 'NONE', 5,
 ( #4230, #15881, #8876, #26978, #11042, #22017, #6864, #9173, #2064 ),
 .UNSPECIFIED., .F., .F.,
 ( 6, 3, 6 ),
 ( 0.000000000000000000, 0.5000000000000000000, 1.000000000000000000 ),
 .UNSPECIFIED. ) ;
#14751 = CARTESIAN_POINT ( 'NONE',  ( -32.75504890064814845, -74.50000000070001249, -22.14844718283469760 ) ) ;
#14752 = CARTESIAN_POINT ( 'NONE',  ( 4.403302820470730516, -92.82334897395796247, -30.18047277449198162 ) ) ;
#14753 = CARTESIAN_POINT ( 'NONE',  ( -6.858700158590000484, -97.53592492849999473, 18.86158608849999752 ) ) ;
#14754 = CARTESIAN_POINT ( 'NONE',  ( 8.578180688210000682, -94.24983875559999547, -23.91258280499999955 ) ) ;
#14755 = DIRECTION ( 'NONE',  ( 0.000000000000000000, 1.000000000000000000, 0.000000000000000000 ) ) ;
#14756 = EDGE_CURVE ( 'NONE', #14297, #623, #15586, .T. ) ;
#14757 = AXIS2_PLACEMENT_3D ( 'NONE', #2103, #15766, #26566 ) ;
#14758 = CARTESIAN_POINT ( 'NONE',  ( 9.502793637310000818, -50.93917412489999919, -23.34524706979999920 ) ) ;
#14759 = DIRECTION ( 'NONE',  ( 1.000000000000000000, 0.000000000000000000, 0.000000000000000000 ) ) ;
#14760 = VERTEX_POINT ( 'NONE', #11325 ) ;
#14761 = CARTESIAN_POINT ( 'NONE',  ( -12.04116395852593691, -49.87586154376180758, -19.70838305107999489 ) ) ;
#14762 = CARTESIAN_POINT ( 'NONE',  ( -16.99615325119999909, -99.69348474340000621, 3.341833029000000010 ) ) ;
#14763 = ORIENTED_EDGE ( 'NONE', *, *, #21327, .T. ) ;
#14764 = ORIENTED_EDGE ( 'NONE', *, *, #19493, .T. ) ;
#14765 = EDGE_CURVE ( 'NONE', #11594, #8116, #8847, .T. ) ;
#14766 = CARTESIAN_POINT ( 'NONE',  ( -0.9248989260280000568, -101.3957169669999985, -15.95962757919999753 ) ) ;
#14767 = CARTESIAN_POINT ( 'NONE',  ( -7.265381620139999441, -73.99590173020000350, 39.73102114399999607 ) ) ;
#14768 = CARTESIAN_POINT ( 'NONE',  ( 27.89292634430000106, -72.00000000000000000, 12.34776042340000046 ) ) ;
#14769 = AXIS2_PLACEMENT_3D ( 'NONE', #20461, #7357, #4874 ) ;
#14770 = CARTESIAN_POINT ( 'NONE',  ( 23.59360194539999966, -74.10313260709999383, -31.26971289790000341 ) ) ;
#14771 = DIRECTION ( 'NONE',  ( 1.000000000000000000, 0.000000000000000000, 0.000000000000000000 ) ) ;
#14772 = PRODUCT ( 'Mechanical Shaft Face Seal', 'Mechanical Shaft Face Seal', '', ( #15569 ) ) ;
#14773 = DIRECTION ( 'NONE',  ( 0.000000000000000000, -1.000000000000000000, 0.000000000000000000 ) ) ;
#14774 = CARTESIAN_POINT ( 'NONE',  ( -12.43380386830000006, -65.01950800350000748, -21.83872194130000111 ) ) ;
#14775 = CARTESIAN_POINT ( 'NONE',  ( 7.187003541560001096, -35.30712889009999600, -21.41502073610000068 ) ) ;
#14776 = FACE_BOUND ( 'NONE', #9834, .T. ) ;
#14777 = EDGE_LOOP ( 'NONE', ( #23806, #21338, #8046, #12905 ) ) ;
#14778 = CARTESIAN_POINT ( 'NONE',  ( -40.16286846138842748, -63.35496709432901241, -2.175426692284139651 ) ) ;
#14779 = CIRCLE ( 'NONE', #2231, 6.750000000000000000 ) ;
#14780 = EDGE_LOOP ( 'NONE', ( #27133, #25441, #26022, #28285 ) ) ;
#14781 = EDGE_LOOP ( 'NONE', ( #21222, #3757 ) ) ;
#14782 = CARTESIAN_POINT ( 'NONE',  ( 6.850353625200000351, -36.56979901409999911, -21.56931447779999900 ) ) ;
#14783 = AXIS2_PLACEMENT_3D ( 'NONE', #26508, #25357, #9599 ) ;
#14784 = CARTESIAN_POINT ( 'NONE',  ( 9.324355421639999975, -37.67772341970000127, -22.72952601809999962 ) ) ;
#14785 = CARTESIAN_POINT ( 'NONE',  ( -29.21843977289999827, -92.50000942380000879, 6.434612924249999644 ) ) ;
#14786 = CARTESIAN_POINT ( 'NONE',  ( -0.7205257404357856554, -101.5555610555564812, -15.98376809946171129 ) ) ;
#14787 = EDGE_CURVE ( 'NONE', #25061, #3132, #5087, .T. ) ;
#14788 = CARTESIAN_POINT ( 'NONE',  ( 19.40204233298638670, -19.49096807709544521, -8.935689512806787249 ) ) ;
#14789 = ORIENTED_EDGE ( 'NONE', *, *, #28286, .F. ) ;
#14790 = CARTESIAN_POINT ( 'NONE',  ( 21.34291133579999666, -34.88462696900000282, -7.355130963909999764 ) ) ;
#14791 = DIRECTION ( 'NONE',  ( 0.4794255386042040601, 0.000000000000000000, 0.8775825618903720926 ) ) ;
#14792 = VERTEX_POINT ( 'NONE', #17907 ) ;
#14793 = CARTESIAN_POINT ( 'NONE',  ( 7.688401808063399123, -37.38063849119085802, -21.51556169207930225 ) ) ;
#14794 = EDGE_LOOP ( 'NONE', ( #24630, #7737, #7378, #24415 ) ) ;
#14795 = AXIS2_PLACEMENT_3D ( 'NONE', #11620, #18492, #13968 ) ;
#14796 = CARTESIAN_POINT ( 'NONE',  ( -14.07972454189999922, -80.06168576349999455, 36.83675998920000438 ) ) ;
#14797 = CIRCLE ( 'NONE', #2261, 23.36116116979999902 ) ;
#14798 = CARTESIAN_POINT ( 'NONE',  ( -21.60034894820000062, -79.50000026560000776, -32.77174736439999947 ) ) ;
#14799 = CARTESIAN_POINT ( 'NONE',  ( 22.77479935359999885, -18.50000000000000000, 9.339609977220000303 ) ) ;
#14800 = CARTESIAN_POINT ( 'NONE',  ( 50.00000000000000000, 0.000000000000000000, -4.500000000000000000 ) ) ;
#14801 = CARTESIAN_POINT ( 'NONE',  ( -20.30440251859999989, -57.41946959940000283, 14.68517168900000058 ) ) ;
#14802 = ORIENTED_EDGE ( 'NONE', *, *, #25132, .T. ) ;
#14803 = B_SPLINE_CURVE_WITH_KNOTS ( 'NONE', 3,
 ( #11983, #2983, #18710, #14325, #27864, #27607, #12123, #7345, #7911, #814, #23219, #5713, #9799, #2831, #18417, #11844, #21041, #16210, #20603, #1098, #27306, #18852, #27739, #7775, #5156, #16648, #9656, #16365, #9525, #11551, #528, #5312, #14201 ),
 .UNSPECIFIED., .F., .F.,
 ( 4, 2, 2, 1, 1, 1, 2, 2, 2, 1, 1, 1, 2, 2, 2, 1, 1, 1, 2, 2, 4 ),
 ( 0.000000000000000000, 0.1249999999997201128, 0.1874999999995801137, 0.2187499999995101141, 0.2343749999994829691, 0.2421874999994777233, 0.2460937499994894084, 0.2499999999995011213, 0.3749999999996395106, 0.4374999999997140621, 0.4687499999997555844, 0.4843749999997764011, 0.4921874999997811750, 0.4999999999997859490, 0.6249999999997878364, 0.6874999999997887246, 0.7187499999997886135, 0.7343749999997895017, 0.7421874999997863931, 0.7499999999997831734, 1.000000000000000000 ),
 .UNSPECIFIED. ) ;
#14804 = DIRECTION ( 'NONE',  ( 0.000000000000000000, 1.000000000000000000, 0.000000000000000000 ) ) ;
#14805 = CARTESIAN_POINT ( 'NONE',  ( -12.46510431380000128, -101.3138676899999950, -9.893369620240001439 ) ) ;
#14806 = CARTESIAN_POINT ( 'NONE',  ( -7.250909741841712552, -73.85719096284161367, 39.82033721815452765 ) ) ;
#14807 = CARTESIAN_POINT ( 'NONE',  ( -7.339513061798150773, -101.3846248973262618, 14.44658188679844102 ) ) ;
#14808 = EDGE_LOOP ( 'NONE', ( #10957, #4427, #17389, #12845 ) ) ;
#14809 = FACE_OUTER_BOUND ( 'NONE', #15425, .T. ) ;
#14810 = CYLINDRICAL_SURFACE ( 'NONE', #14335, 0.8000000000000005995 ) ;
#14811 = CARTESIAN_POINT ( 'NONE',  ( 36.86771591380000501, -80.05866228240000737, -13.93700013870000021 ) ) ;
#14812 = ORIENTED_EDGE ( 'NONE', *, *, #7253, .F. ) ;
#14813 = AXIS2_PLACEMENT_3D ( 'NONE', #15518, #11295, #2289 ) ;
#14814 = VECTOR ( 'NONE', #16175, 1000.000000000000000 ) ;
#14815 = FACE_OUTER_BOUND ( 'NONE', #7569, .T. ) ;
#14816 = CARTESIAN_POINT ( 'NONE',  ( -28.54979082390000045, -12.59999999999999964, -52.26004156059999417 ) ) ;
#14817 = ORIENTED_EDGE ( 'NONE', *, *, #26826, .F. ) ;
#14818 = CARTESIAN_POINT ( 'NONE',  ( 46.34744280896714486, -73.59863498251932867, -3.503223591168824314 ) ) ;
#14819 = ORIENTED_EDGE ( 'NONE', *, *, #295, .T. ) ;
#14820 = CARTESIAN_POINT ( 'NONE',  ( 26.25071228570000059, -93.07694010310001431, 10.86079363670000042 ) ) ;
#14821 = CARTESIAN_POINT ( 'NONE',  ( 21.71672445076383440, -36.72346566043151483, -8.838003624040505102 ) ) ;
#14822 = CARTESIAN_POINT ( 'NONE',  ( -7.135467526410000261, -73.50000000000000000, -38.71641004229999794 ) ) ;
#14823 = ORIENTED_EDGE ( 'NONE', *, *, #13200, .F. ) ;
#14824 = CARTESIAN_POINT ( 'NONE',  ( 7.066909182079999852, -57.47855601759999900, -22.26662627820000040 ) ) ;
#14825 = DIRECTION ( 'NONE',  ( 0.5439177849611214199, 0.000000000000000000, -0.8391385125251892285 ) ) ;
#14826 = AXIS2_PLACEMENT_3D ( 'NONE', #138, #8987, #18036 ) ;
#14827 = CARTESIAN_POINT ( 'NONE',  ( 22.01683849324958331, -37.96202148674316845, -8.793068656874689637 ) ) ;
#14828 = CARTESIAN_POINT ( 'NONE',  ( 19.55470396879999839, -26.09861276219999837, 10.64709123559999959 ) ) ;
#14829 = CARTESIAN_POINT ( 'NONE',  ( -0.9583274171050000234, -18.50000000000000000, -21.03286107679999972 ) ) ;
#14830 = EDGE_LOOP ( 'NONE', ( #11365, #3766, #5647, #2209 ) ) ;
#14831 = TOROIDAL_SURFACE ( 'NONE', #6942, 15.50000000000000000, 0.5000000000000000000 ) ;
#14832 = VECTOR ( 'NONE', #24796, 1000.000000000000000 ) ;
#14833 = CARTESIAN_POINT ( 'NONE',  ( -16.89577420600000224, -97.73638926269998706, -10.62153989119999942 ) ) ;
#14834 = CARTESIAN_POINT ( 'NONE',  ( 12.22678147189999898, -101.0956037589999994, -9.599435331940000538 ) ) ;
#14835 = CARTESIAN_POINT ( 'NONE',  ( 23.35417726369999869, -57.47855601759999900, -0.5711878298099999363 ) ) ;
#14836 = CARTESIAN_POINT ( 'NONE',  ( 24.69157579510000033, -92.76550115769998683, -13.71735200580000047 ) ) ;
#14837 = CARTESIAN_POINT ( 'NONE',  ( -2.565902251719999860, -54.99674360790000094, -24.86453770889999859 ) ) ;
#14838 = TOROIDAL_SURFACE ( 'NONE', #19955, 3.500000000000000000, 0.5000000000000000000 ) ;
#14839 = CARTESIAN_POINT ( 'NONE',  ( -1.521130821679999912, -79.83261741180000115, 47.18112646320000181 ) ) ;
#14840 = PLANE ( 'NONE',  #25679 ) ;
#14841 = ORIENTED_EDGE ( 'NONE', *, *, #20330, .T. ) ;
#14842 = CARTESIAN_POINT ( 'NONE',  ( 40.00000000000000000, -84.50000000000000000, -8.798132407700000305E-16 ) ) ;
#14843 = B_SPLINE_CURVE_WITH_KNOTS ( 'NONE', 5,
 ( #25862, #27906, #7947, #7684, #1403, #14495, #10246, #23395, #5753, #7543, #14363, #5474 ),
 .UNSPECIFIED., .F., .F.,
 ( 6, 3, 3, 6 ),
 ( 0.000000000000000000, 0.4964111757630880195, 0.7833083924342724158, 1.000000000000000000 ),
 .UNSPECIFIED. ) ;
#14844 = EDGE_CURVE ( 'NONE', #17563, #5033, #28789, .T. ) ;
#14845 = DIRECTION ( 'NONE',  ( 0.000000000000000000, -1.000000000000000000, 0.000000000000000000 ) ) ;
#14846 = DIRECTION ( 'NONE',  ( 0.8775825618903722036, 0.000000000000000000, -0.4794255386042041156 ) ) ;
#14847 = CARTESIAN_POINT ( 'NONE',  ( -7.879410208250000380, -99.92967571559999840, 15.46934584979999983 ) ) ;
#14848 = EDGE_CURVE ( 'NONE', #5829, #13319, #4622, .T. ) ;
#14849 = CARTESIAN_POINT ( 'NONE',  ( 5.988482279510000053E-15, -69.50000000000000000, 40.00000000000000000 ) ) ;
#14850 = EDGE_CURVE ( 'NONE', #3921, #13319, #2472, .T. ) ;
#14851 = ADVANCED_FACE ( 'NONE', ( #4794 ), #2677, .T. ) ;
#14852 = AXIS2_PLACEMENT_3D ( 'NONE', #3148, #7530, #16386 ) ;
#14853 = VERTEX_POINT ( 'NONE', #13814 ) ;
#14854 = CARTESIAN_POINT ( 'NONE',  ( 11.70455088819999823, -93.00000000000000000, 8.942783294160001617 ) ) ;
#14855 = ORIENTED_EDGE ( 'NONE', *, *, #9401, .F. ) ;
#14856 = CARTESIAN_POINT ( 'NONE',  ( 21.27799938559999759, -36.28875681020000599, -8.154524242129999934 ) ) ;
#14857 = CARTESIAN_POINT ( 'NONE',  ( -21.99985828019999801, -74.00000000000000000, -31.89935321680000158 ) ) ;
#14858 = ORIENTED_EDGE ( 'NONE', *, *, #1683, .F. ) ;
#14859 = CARTESIAN_POINT ( 'NONE',  ( 12.00742146600000204, -96.90532602029999509, 17.10694051450000330 ) ) ;
#14860 = CARTESIAN_POINT ( 'NONE',  ( -8.303419408699999948, -99.91102932029998840, 14.75134094139999874 ) ) ;
#14861 = CARTESIAN_POINT ( 'NONE',  ( -2.934900197419999746, -94.89197151660000884, 23.49669041109999768 ) ) ;
#14862 = CARTESIAN_POINT ( 'NONE',  ( 9.063833271400000058, -53.25913232279999932, -22.59227796120000065 ) ) ;
#14863 = ORIENTED_EDGE ( 'NONE', *, *, #14056, .T. ) ;
#14864 = CARTESIAN_POINT ( 'NONE',  ( 12.83479102393274296, -101.4241070620153806, -9.841145288938006885 ) ) ;
#14865 = CARTESIAN_POINT ( 'NONE',  ( 24.10233903080000317, -34.62274519429999486, 1.400979379020000026 ) ) ;
#14866 = CARTESIAN_POINT ( 'NONE',  ( 39.81550290694978855, -73.86170940508526428, 7.247654292427061051 ) ) ;
#14867 = ORIENTED_EDGE ( 'NONE', *, *, #7429, .T. ) ;
#14868 = CARTESIAN_POINT ( 'NONE',  ( -14.63774944959999935, -74.36723410090000641, 36.92911291229999904 ) ) ;
#14869 = AXIS2_PLACEMENT_3D ( 'NONE', #4765, #4321, #20055 ) ;
#14870 = CARTESIAN_POINT ( 'NONE',  ( -14.74467115470000067, -74.36322263760000340, 36.36119636340000483 ) ) ;
#14871 = CARTESIAN_POINT ( 'NONE',  ( 0.000000000000000000, -84.00000000000000000, -40.00000000000000000 ) ) ;
#14872 = DIRECTION ( 'NONE',  ( 1.000000000000000000, 0.000000000000000000, 0.000000000000000000 ) ) ;
#14873 = EDGE_LOOP ( 'NONE', ( #28120, #19627, #3798, #9437, #14041, #3474 ) ) ;
#14874 = CIRCLE ( 'NONE', #986, 39.25000000000000000 ) ;
#14875 = AXIS2_PLACEMENT_3D ( 'NONE', #7231, #6642, #8950 ) ;
#14876 = DIRECTION ( 'NONE',  ( 0.000000000000000000, -1.000000000000000000, 0.000000000000000000 ) ) ;
#14877 = CARTESIAN_POINT ( 'NONE',  ( 0.1178905558060000108, -101.2358105800000061, -15.21680457949999976 ) ) ;
#14878 = CARTESIAN_POINT ( 'NONE',  ( 9.246558180430000107, -61.84557969829999990, -23.23378279429999793 ) ) ;
#14879 = CARTESIAN_POINT ( 'NONE',  ( -12.80327907979999935, -69.29931929910000576, -23.86045200970000124 ) ) ;
#14880 = DIRECTION ( 'NONE',  ( 1.000000000000000000, 0.000000000000000000, 0.000000000000000000 ) ) ;
#14881 = CARTESIAN_POINT ( 'NONE',  ( -11.41591306159999952, -19.46348310600000175, -18.84564791440000064 ) ) ;
#14882 = ORIENTED_EDGE ( 'NONE', *, *, #19158, .T. ) ;
#14883 = EDGE_CURVE ( 'NONE', #4936, #7139, #3196, .T. ) ;
#14884 = CARTESIAN_POINT ( 'NONE',  ( 6.820352230450000164, -100.2522625769999962, 15.59059167250000044 ) ) ;
#14885 = CARTESIAN_POINT ( 'NONE',  ( -15.60709619170274998, -92.58000264305866267, -24.03322618717208314 ) ) ;
#14886 = EDGE_CURVE ( 'NONE', #14636, #2790, #970, .T. ) ;
#14887 = CARTESIAN_POINT ( 'NONE',  ( -40.09065349277244650, -65.74402559150934167, -2.175413822581698575 ) ) ;
#14888 = CARTESIAN_POINT ( 'NONE',  ( 5.634073923585436461, -92.54893169919640172, -29.97511075432250749 ) ) ;
#14889 = CARTESIAN_POINT ( 'NONE',  ( -12.47194051069999965, -65.04696943620000127, 21.82660845869999733 ) ) ;
#14890 = ORIENTED_EDGE ( 'NONE', *, *, #18238, .T. ) ;
#14891 = CIRCLE ( 'NONE', #10675, 32.39999999999999858 ) ;
#14892 = CARTESIAN_POINT ( 'NONE',  ( 6.395435569720000046, -92.99570653130000153, -26.06839265949999884 ) ) ;
#14893 = AXIS2_PLACEMENT_3D ( 'NONE', #9318, #7008, #22601 ) ;
#14894 = AXIS2_PLACEMENT_3D ( 'NONE', #26573, #15176, #24089 ) ;
#14895 = DIRECTION ( 'NONE',  ( 0.000000000000000000, 1.000000000000000000, 0.000000000000000000 ) ) ;
#14896 = CARTESIAN_POINT ( 'NONE',  ( -6.659687227720000102, -101.1292389600000092, 14.00371911340000075 ) ) ;
#14897 = EDGE_LOOP ( 'NONE', ( #27127, #27368, #19197, #7361, #12138 ) ) ;
#14898 = DIRECTION ( 'NONE',  ( 1.000000000000000000, 0.000000000000000000, 0.000000000000000000 ) ) ;
#14899 = DIRECTION ( 'NONE',  ( 1.000000000000000000, 0.000000000000000000, 0.000000000000000000 ) ) ;
#14900 = ORIENTED_EDGE ( 'NONE', *, *, #7512, .F. ) ;
#14901 = CARTESIAN_POINT ( 'NONE',  ( -1.164566756239999945, -101.0314399550000104, -15.81222527010000078 ) ) ;
#14902 = CARTESIAN_POINT ( 'NONE',  ( 29.17304402409999753, -10.50000000000000000, 53.40089889099999709 ) ) ;
#14903 = CARTESIAN_POINT ( 'NONE',  ( -13.14595447578818010, -93.06132686323303460, -23.62747619079523531 ) ) ;
#14904 = DIRECTION ( 'NONE',  ( 1.000000000000000000, 0.000000000000000000, 0.000000000000000000 ) ) ;
#14905 = CARTESIAN_POINT ( 'NONE',  ( 16.39013412538344383, -94.61155572397261437, 17.21914651918165973 ) ) ;
#14906 = CARTESIAN_POINT ( 'NONE',  ( 27.18988201479999844, -27.50155444569999830, 49.77074518290000071 ) ) ;
#14908 = EDGE_CURVE ( 'NONE', #22782, #18665, #26382, .T. ) ;
#14907 = DIRECTION ( 'NONE',  ( -0.000000000000000000, 1.000000000000000000, 0.000000000000000000 ) ) ;
#14909 = DIRECTION ( 'NONE',  ( -0.8791797166759636184, 0.000000000000000000, -0.4764903207679798691 ) ) ;
#14910 = DIRECTION ( 'NONE',  ( 0.000000000000000000, 1.000000000000000000, 0.000000000000000000 ) ) ;
#14911 = AXIS2_PLACEMENT_3D ( 'NONE', #17360, #21451, #17506 ) ;
#14912 = ORIENTED_EDGE ( 'NONE', *, *, #11591, .F. ) ;
#14913 = ADVANCED_FACE ( 'NONE', ( #25200 ), #17668, .F. ) ;
#14914 = CARTESIAN_POINT ( 'NONE',  ( -10.57118441995368130, -18.60777261480114575, -22.16921275799352742 ) ) ;
#14915 = AXIS2_PLACEMENT_3D ( 'NONE', #27608, #3269, #7647 ) ;
#14916 = B_SPLINE_CURVE_WITH_KNOTS ( 'NONE', 3,
 ( #10699, #4323, #8537, #17442, #8671, #2146 ),
 .UNSPECIFIED., .F., .F.,
 ( 4, 2, 4 ),
 ( 0.000000000000000000, 0.5000000000000000000, 1.000000000000000000 ),
 .UNSPECIFIED. ) ;
#14917 = EDGE_LOOP ( 'NONE', ( #26352, #15095, #10649, #25047 ) ) ;
#14918 = AXIS2_PLACEMENT_3D ( 'NONE', #10839, #4161, #8811 ) ;
#14919 = CARTESIAN_POINT ( 'NONE',  ( 22.49121776710000020, -37.66961400949999472, -9.214873578599998893 ) ) ;
#14920 = ADVANCED_FACE ( 'NONE', ( #25043 ), #12054, .F. ) ;
#14921 = ORIENTED_EDGE ( 'NONE', *, *, #1683, .T. ) ;
#14922 = CARTESIAN_POINT ( 'NONE',  ( -1.604812631230000175, -64.93834956060000252, -25.19372014690000228 ) ) ;
#14923 = CARTESIAN_POINT ( 'NONE',  ( 10.32053900859999906, -36.18404281990000015, -22.30282316619999960 ) ) ;
#14924 = CARTESIAN_POINT ( 'NONE',  ( -28.98513075869999867, -93.04780269100000112, 3.123877206889999592 ) ) ;
#14925 = CARTESIAN_POINT ( 'NONE',  ( -11.35954001540000036, -74.50000000000000000, 46.75000000000000000 ) ) ;
#14926 = CARTESIAN_POINT ( 'NONE',  ( -32.75000000000000000, -73.50000000000000000, 4.241051954069999455E-15 ) ) ;
#14927 = ORIENTED_EDGE ( 'NONE', *, *, #20939, .F. ) ;
#14928 = CARTESIAN_POINT ( 'NONE',  ( 21.44331570410000154, -35.78513242900000080, -7.217843123729999810 ) ) ;
#14929 = CARTESIAN_POINT ( 'NONE',  ( -12.68423258129978315, -57.45864775708258065, 20.28109956509949896 ) ) ;
#14930 = ORIENTED_EDGE ( 'NONE', *, *, #10364, .T. ) ;
#14931 = CIRCLE ( 'NONE', #19603, 11.00000000000000000 ) ;
#14932 = FACE_OUTER_BOUND ( 'NONE', #504, .T. ) ;
#14933 = AXIS2_PLACEMENT_3D ( 'NONE', #22119, #13658, #17598 ) ;
#14934 = CARTESIAN_POINT ( 'NONE',  ( -17.58882677589999943, -18.50000000000000000, 13.37910508939999943 ) ) ;
#14935 = CARTESIAN_POINT ( 'NONE',  ( -15.58072764279999944, -101.4054056550000098, 3.556023071709999872 ) ) ;
#14936 = CARTESIAN_POINT ( 'NONE',  ( -32.48620205747189971, -74.10974938391861144, -22.14461327791768142 ) ) ;
#14937 = CARTESIAN_POINT ( 'NONE',  ( -19.79578083020000179, -57.47815899190000266, 12.40825019989999767 ) ) ;
#14938 = ORIENTED_EDGE ( 'NONE', *, *, #8030, .T. ) ;
#14939 = DIRECTION ( 'NONE',  ( 0.2414462220490750377, 0.000000000000000000, -0.9704142011833034598 ) ) ;
#14940 = CARTESIAN_POINT ( 'NONE',  ( -12.57055767900000021, -101.5369810359999860, -9.898859202520000622 ) ) ;
#14941 = CARTESIAN_POINT ( 'NONE',  ( 18.00137301776900856, -94.36683344921111427, 16.74636862984975139 ) ) ;
#14942 = DIRECTION ( 'NONE',  ( 0.4794255386042040601, 0.000000000000000000, 0.8775825618903720926 ) ) ;
#14943 = ORIENTED_EDGE ( 'NONE', *, *, #17606, .F. ) ;
#14944 = ADVANCED_FACE ( 'NONE', ( #9438 ), #9725, .T. ) ;
#14945 = VECTOR ( 'NONE', #17132, 1000.000000000000000 ) ;
#14946 = CARTESIAN_POINT ( 'NONE',  ( -14.93121066289999987, -74.50000000000000000, 36.29905574720000061 ) ) ;
#14947 = CARTESIAN_POINT ( 'NONE',  ( -32.09407551019999971, -74.00665451570000641, -22.04839896869999905 ) ) ;
#14948 = CARTESIAN_POINT ( 'NONE',  ( 7.627568735119999666, -74.00000000000000000, 38.62788659690000515 ) ) ;
#14949 = ORIENTED_EDGE ( 'NONE', *, *, #23358, .F. ) ;
#14950 = EDGE_CURVE ( 'NONE', #16297, #6421, #9758, .T. ) ;
#14951 = TOROIDAL_SURFACE ( 'NONE', #3366, 3.750000000000000000, 1.000000000000000000 ) ;
#14952 = CARTESIAN_POINT ( 'NONE',  ( 7.033065480937148450, -100.0863963177764617, 15.73315454065260255 ) ) ;
#14953 = CARTESIAN_POINT ( 'NONE',  ( -2.658799883775093686, -80.38812240490400995, 46.74488113567394976 ) ) ;
#14954 = VERTEX_POINT ( 'NONE', #20680 ) ;
#14955 = CYLINDRICAL_SURFACE ( 'NONE', #2096, 7.249999999999999112 ) ;
#14956 = VERTEX_POINT ( 'NONE', #9871 ) ;
#14957 = CARTESIAN_POINT ( 'NONE',  ( 29.11677851939999684, -92.50000942380000879, 6.880019978119999990 ) ) ;
#14958 = CARTESIAN_POINT ( 'NONE',  ( 0.000000000000000000, -89.50000000000000000, 0.000000000000000000 ) ) ;
#14959 = CARTESIAN_POINT ( 'NONE',  ( -7.219524535890000649, -73.62955962630000784, -39.18053445169999804 ) ) ;
#14960 = VERTEX_POINT ( 'NONE', #11918 ) ;
#14961 = CARTESIAN_POINT ( 'NONE',  ( 12.08982211680000063, -101.2010924020000004, -9.314613846919998608 ) ) ;
#14962 = CARTESIAN_POINT ( 'NONE',  ( -3.610293368829999849, -18.50000000000000000, -24.43613445369999937 ) ) ;
#14963 = EDGE_CURVE ( 'NONE', #23549, #14989, #11596, .T. ) ;
#14964 = CARTESIAN_POINT ( 'NONE',  ( 9.510883186780000997, -36.00000000010000178, -20.82957718990000018 ) ) ;
#14965 = CARTESIAN_POINT ( 'NONE',  ( -42.25000000000000000, -63.30468293320000583, -0.7216878364880000563 ) ) ;
#14966 = CIRCLE ( 'NONE', #1984, 4.750000000000000888 ) ;
#14967 = CARTESIAN_POINT ( 'NONE',  ( -1.776356839399999804E-15, -79.50000000000000000, 47.25000000000000000 ) ) ;
#14968 = EDGE_LOOP ( 'NONE', ( #13435, #15285, #1319 ) ) ;
#14969 = CARTESIAN_POINT ( 'NONE',  ( -20.51958746069999862, -95.60035679230000483, -9.357022945640000700 ) ) ;
#14970 = CARTESIAN_POINT ( 'NONE',  ( 12.52961185140000033, -101.3852859389999992, -9.939768331349998931 ) ) ;
#14971 = CARTESIAN_POINT ( 'NONE',  ( -2.876553231629999985, -108.5000000000000000, -5.265495371340000119 ) ) ;
#14972 = CARTESIAN_POINT ( 'NONE',  ( 23.41224063439999981, -93.87552273890000265, -8.246875224729999232 ) ) ;
#14973 = CARTESIAN_POINT ( 'NONE',  ( -2.360777964760000458, -53.80651132049999319, -24.23647548509999794 ) ) ;
#14974 = CARTESIAN_POINT ( 'NONE',  ( 29.84440213756046845, -92.58347372263781949, 6.289810756387969271 ) ) ;
#14975 = LINE ( 'NONE', #28389, #27573 ) ;
#14976 = EDGE_LOOP ( 'NONE', ( #11218, #1988, #21396, #13645 ) ) ;
#14978 = EDGE_CURVE ( 'NONE', #22416, #24004, #3784, .T. ) ;
#14977 = DIRECTION ( 'NONE',  ( -0.2796552172570731520, 0.000000000000000000, -0.9601004944592516077 ) ) ;
#14979 = DIRECTION ( 'NONE',  ( 0.4794255386042040601, 0.000000000000000000, 0.8775825618903722036 ) ) ;
#14980 = CARTESIAN_POINT ( 'NONE',  ( 18.29259584288750773, -98.99956642725410916, 3.353674926929683497 ) ) ;
#14981 = CARTESIAN_POINT ( 'NONE',  ( -38.25000000000000000, -65.17124718639999514, 2.640283750789999662 ) ) ;
#14982 = CARTESIAN_POINT ( 'NONE',  ( -14.48905496503022583, -70.53876985267483235, 23.53798342341141492 ) ) ;
#14983 = CARTESIAN_POINT ( 'NONE',  ( 0.000000000000000000, -102.8486084350000027, 0.000000000000000000 ) ) ;
#14984 = AXIS2_PLACEMENT_3D ( 'NONE', #27755, #7794, #16665 ) ;
#14985 = AXIS2_PLACEMENT_3D ( 'NONE', #325, #19664, #13099 ) ;
#14986 = ORIENTED_EDGE ( 'NONE', *, *, #15467, .T. ) ;
#14987 = CARTESIAN_POINT ( 'NONE',  ( -6.705637591229999472, -74.00000000000000000, 35.51864961870000315 ) ) ;
#14988 = CARTESIAN_POINT ( 'NONE',  ( 20.69709980620000067, -35.75422006420000542, -8.773405848899999526 ) ) ;
#14989 = VERTEX_POINT ( 'NONE', #8502 ) ;
#14990 = CARTESIAN_POINT ( 'NONE',  ( 20.16934030379999854, -35.86380921170000136, -9.031588964350000026 ) ) ;
#14991 = DIRECTION ( 'NONE',  ( 0.000000000000000000, 1.000000000000000000, 0.000000000000000000 ) ) ;
#14992 = VERTEX_POINT ( 'NONE', #26435 ) ;
#14993 = CARTESIAN_POINT ( 'NONE',  ( -12.41793182790000039, -101.2530993039999885, -8.757551688899999576 ) ) ;
#14994 = CARTESIAN_POINT ( 'NONE',  ( 3.940393887960000008, -92.70565333729999224, 28.26336050760000163 ) ) ;
#14995 = AXIS2_PLACEMENT_3D ( 'NONE', #22322, #8471, #24066 ) ;
#14996 = DIRECTION ( 'NONE',  ( 0.000000000000000000, -1.000000000000000000, 0.000000000000000000 ) ) ;
#14997 = CARTESIAN_POINT ( 'NONE',  ( -29.72951945062797918, -92.77521214513809866, 6.812272564689533461 ) ) ;
#14998 = CYLINDRICAL_SURFACE ( 'NONE', #24618, 5.999999999999999112 ) ;
#14999 = EDGE_LOOP ( 'NONE', ( #2058, #7769, #8903, #9297 ) ) ;
#15000 = CARTESIAN_POINT ( 'NONE',  ( 13.23050100943412133, -101.0147714270161288, -9.847845762695030203 ) ) ;
#15001 = CARTESIAN_POINT ( 'NONE',  ( 22.27593118400000094, -19.46147658920000012, 0.5502460698960000007 ) ) ;
#15002 = CARTESIAN_POINT ( 'NONE',  ( 24.87884979860000101, -67.58705842039999823, 10.90550133649999864 ) ) ;
#15003 = CARTESIAN_POINT ( 'NONE',  ( -50.00000000000000000, 0.000000000000000000, 4.500000000000000000 ) ) ;
#15004 = ORIENTED_EDGE ( 'NONE', *, *, #8663, .T. ) ;
#15005 = CARTESIAN_POINT ( 'NONE',  ( -40.28432270880000488, -74.37142462010000088, 7.256994698139999755 ) ) ;
#15006 = EDGE_CURVE ( 'NONE', #4268, #28156, #22801, .T. ) ;
#15007 = AXIS2_PLACEMENT_3D ( 'NONE', #16933, #25538, #20893 ) ;
#15008 = DIRECTION ( 'NONE',  ( 1.000000000000000000, 0.000000000000000000, 0.000000000000000000 ) ) ;
#15009 = CARTESIAN_POINT ( 'NONE',  ( -17.68470881210000201, -94.03347263330000771, 17.09197474180000142 ) ) ;
#15010 = CARTESIAN_POINT ( 'NONE',  ( -20.63373432448497269, -93.20343033882606676, 16.19767797687812916 ) ) ;
#15011 = ORIENTED_EDGE ( 'NONE', *, *, #23622, .F. ) ;
#15012 = CARTESIAN_POINT ( 'NONE',  ( 26.61465533970000052, -68.28989644159999273, 0.1578866888799999868 ) ) ;
#15013 = CARTESIAN_POINT ( 'NONE',  ( -0.07581514835600000612, -101.1292389600000092, -15.50644495179999893 ) ) ;
#15014 = CARTESIAN_POINT ( 'NONE',  ( 9.111815586569999681, -58.91975330950000256, -22.76485177850000241 ) ) ;
#15015 = CARTESIAN_POINT ( 'NONE',  ( -13.17060624760000032, -68.28989248250000799, -23.12789913420000332 ) ) ;
#15016 = CARTESIAN_POINT ( 'NONE',  ( 20.64374742240000060, -57.47815889169999792, 10.93951826979999886 ) ) ;
#15017 = CARTESIAN_POINT ( 'NONE',  ( 0.000000000000000000, -37.57799544290000426, 0.000000000000000000 ) ) ;
#15018 = ORIENTED_EDGE ( 'NONE', *, *, #13648, .F. ) ;
#15019 = CARTESIAN_POINT ( 'NONE',  ( 6.592724576960000249, -99.70407914540000149, 15.88227091829999971 ) ) ;
#15020 = CARTESIAN_POINT ( 'NONE',  ( 15.63748056140000209, -101.5369810359999860, 3.386620984279999913 ) ) ;
#15021 = AXIS2_PLACEMENT_3D ( 'NONE', #9400, #18154, #13778 ) ;
#15022 = CARTESIAN_POINT ( 'NONE',  ( -28.44874375979999925, -10.08849557519999962, -52.07507615039999394 ) ) ;
#15023 = CARTESIAN_POINT ( 'NONE',  ( 4.907579521315320825, -92.69183043809221090, -30.10272373264253787 ) ) ;
#15024 = B_SPLINE_CURVE_WITH_KNOTS ( 'NONE', 5,
 ( #11045, #19961, #24490, #24793, #9176, #27126, #15434, #9478, #17940 ),
 .UNSPECIFIED., .F., .F.,
 ( 6, 3, 6 ),
 ( 0.000000000000000000, 0.3290135943971881360, 1.000000000000000000 ),
 .UNSPECIFIED. ) ;
#15025 = DIRECTION ( 'NONE',  ( -0.3390050494208429743, 0.7071067811866730279, -0.6205445805637129775 ) ) ;
#15026 = ORIENTED_EDGE ( 'NONE', *, *, #13684, .T. ) ;
#15027 = AXIS2_PLACEMENT_3D ( 'NONE', #22028, #24497, #6581 ) ;
#15028 = CARTESIAN_POINT ( 'NONE',  ( 4.747154956369999290, -93.07693985719998864, -28.00930810119999848 ) ) ;
#15029 = CARTESIAN_POINT ( 'NONE',  ( 27.68682485439999752, -24.80000000000000071, 50.68039294919999804 ) ) ;
#15030 = CARTESIAN_POINT ( 'NONE',  ( -1.303833584549999980, -101.1364147039999892, -15.29041300709999796 ) ) ;
#15031 = CARTESIAN_POINT ( 'NONE',  ( -6.833925942180000490, -101.4254868729999970, 14.43295880549999843 ) ) ;
#15032 = ORIENTED_EDGE ( 'NONE', *, *, #941, .F. ) ;
#15033 = DIRECTION ( 'NONE',  ( -7.486357007659999211E-17, 0.000000000000000000, 1.000000000000000000 ) ) ;
#15034 = CARTESIAN_POINT ( 'NONE',  ( -12.46005120850608705, -101.3038909013870921, -10.45748730976263374 ) ) ;
#15035 = ORIENTED_EDGE ( 'NONE', *, *, #15531, .F. ) ;
#15036 = EDGE_CURVE ( 'NONE', #20989, #24745, #24661, .T. ) ;
#15037 = DIRECTION ( 'NONE',  ( 0.000000000000000000, -1.000000000000000000, 0.000000000000000000 ) ) ;
#15038 = ORIENTED_EDGE ( 'NONE', *, *, #81, .T. ) ;
#15039 = ADVANCED_FACE ( 'NONE', ( #10278 ), #3332, .F. ) ;
#15040 = CARTESIAN_POINT ( 'NONE',  ( -0.7205257403800000571, -101.6484611540000031, -15.98376809950000066 ) ) ;
#15041 = VECTOR ( 'NONE', #9916, 1000.000000000000000 ) ;
#15042 = DIRECTION ( 'NONE',  ( 0.000000000000000000, 1.000000000000000000, 0.000000000000000000 ) ) ;
#15043 = CARTESIAN_POINT ( 'NONE',  ( 14.62247892739999955, -90.50000000000000000, 26.76626813769999913 ) ) ;
#15044 = CIRCLE ( 'NONE', #7187, 2.000000000000000888 ) ;
#15045 = CARTESIAN_POINT ( 'NONE',  ( 12.88056670439999962, -94.79581646409999962, -19.86310537439999990 ) ) ;
#15046 = DIRECTION ( 'NONE',  ( -1.000000000000000000, 0.000000000000000000, -1.224606353820000075E-16 ) ) ;
#15047 = EDGE_CURVE ( 'NONE', #20359, #22101, #1862, .T. ) ;
#15048 = CARTESIAN_POINT ( 'NONE',  ( 19.24256498990000352, -18.50000000000000000, -7.923762209979999582 ) ) ;
#15049 = ADVANCED_FACE ( 'NONE', ( #12196 ), #26499, .F. ) ;
#15050 = FACE_OUTER_BOUND ( 'NONE', #6876, .T. ) ;
#15051 = CARTESIAN_POINT ( 'NONE',  ( 0.000000000000000000, -83.75000000000000000, 0.000000000000000000 ) ) ;
#15052 = CARTESIAN_POINT ( 'NONE',  ( -18.82843809638912447, -19.48034373446246548, 13.69127826824404615 ) ) ;
#15053 = AXIS2_PLACEMENT_3D ( 'NONE', #18239, #27134, #4973 ) ;
#15054 = CARTESIAN_POINT ( 'NONE',  ( 7.506539852059999518, -35.02344201600000417, -21.30237675789999940 ) ) ;
#15055 = CARTESIAN_POINT ( 'NONE',  ( -19.73459501710000197, -19.50000000000000000, 14.41863426819999994 ) ) ;
#15056 = ORIENTED_EDGE ( 'NONE', *, *, #11125, .T. ) ;
#15057 = CARTESIAN_POINT ( 'NONE',  ( 7.780770465739999864, -18.50000000000000000, -19.47999901649999543 ) ) ;
#15058 = CARTESIAN_POINT ( 'NONE',  ( 22.72952646779999952, -37.67772343429999893, -9.324355546680001439 ) ) ;
#15059 = CARTESIAN_POINT ( 'NONE',  ( -1.195589003429999853, -62.93490527480000196, -24.29973956710000138 ) ) ;
#15060 = VECTOR ( 'NONE', #4753, 1000.000000000000114 ) ;
#15061 = CARTESIAN_POINT ( 'NONE',  ( 10.88627897289999957, -36.00000000000000000, -22.06017285100000080 ) ) ;
#15062 = CARTESIAN_POINT ( 'NONE',  ( -27.19238942870000031, -93.48569568790000517, -0.5495358801190000086 ) ) ;
#15063 = CARTESIAN_POINT ( 'NONE',  ( -19.80901448590000058, -53.80651132049999319, 14.16273143270000112 ) ) ;
#15064 = ORIENTED_EDGE ( 'NONE', *, *, #3244, .F. ) ;
#15065 = CARTESIAN_POINT ( 'NONE',  ( -18.23664321284092082, -97.24405583968645317, -10.03008010378985482 ) ) ;
#15066 = DIRECTION ( 'NONE',  ( -0.09713222731193690840, 0.000000000000000000, -0.9952714857853720565 ) ) ;
#15067 = EDGE_LOOP ( 'NONE', ( #16844, #27803, #2449, #1643 ) ) ;
#15068 = PRESENTATION_LAYER_ASSIGNMENT (  '', '', ( #20699 ) ) ;
#15069 = DIRECTION ( 'NONE',  ( -0.5000000000001884048, 0.000000000000000000, 0.8660254037843300168 ) ) ;
#15070 = ORIENTED_EDGE ( 'NONE', *, *, #22012, .T. ) ;
#15071 = ADVANCED_FACE ( 'NONE', ( #26297 ), #18975, .T. ) ;
#15072 = CARTESIAN_POINT ( 'NONE',  ( -37.29988270759999835, -74.00000000000000000, -26.69328098980000163 ) ) ;
#15073 = AXIS2_PLACEMENT_3D ( 'NONE', #26128, #28445, #16961 ) ;
#15074 = CARTESIAN_POINT ( 'NONE',  ( 40.70731707320000226, -74.50000000000000000, 7.215414233289999757 ) ) ;
#15075 = ADVANCED_FACE ( 'NONE', ( #2551 ), #15926, .F. ) ;
#15076 = CARTESIAN_POINT ( 'NONE',  ( 22.32094435669999655, -18.62259217289999924, 9.382461709760001156 ) ) ;
#15077 = CARTESIAN_POINT ( 'NONE',  ( -32.71776494810505653, -74.25643782585186159, -22.20071764928750468 ) ) ;
#15078 = CARTESIAN_POINT ( 'NONE',  ( 11.44042105559999989, -101.2530993000000024, -9.998588429619998053 ) ) ;
#15079 = VERTEX_POINT ( 'NONE', #9522 ) ;
#15080 = AXIS2_PLACEMENT_3D ( 'NONE', #10069, #5303, #25688 ) ;
#15081 = CARTESIAN_POINT ( 'NONE',  ( -36.23922253580000330, -80.00000000000000000, -26.33972759919999973 ) ) ;
#15082 = CARTESIAN_POINT ( 'NONE',  ( -11.93759739729999936, -100.7707614970000094, -10.43389714689999970 ) ) ;
#15083 = CARTESIAN_POINT ( 'NONE',  ( 1.678657213230000024E-14, -74.00000000000000000, 7.838174553849999450E-15 ) ) ;
#15084 = CARTESIAN_POINT ( 'NONE',  ( -15.55828293390000105, -111.0000000000000000, 3.733608462140000306 ) ) ;
#15085 = ORIENTED_EDGE ( 'NONE', *, *, #11467, .T. ) ;
#15086 = FACE_BOUND ( 'NONE', #16765, .T. ) ;
#15087 = CARTESIAN_POINT ( 'NONE',  ( -22.59314464595784955, -79.98715482475118677, -32.67653664314131845 ) ) ;
#15088 = VERTEX_POINT ( 'NONE', #13600 ) ;
#15089 = AXIS2_PLACEMENT_3D ( 'NONE', #16634, #7189, #18695 ) ;
#15090 = CARTESIAN_POINT ( 'NONE',  ( 6.663412416092679535, -100.9364580247760301, 15.15463700478743014 ) ) ;
#15091 = CARTESIAN_POINT ( 'NONE',  ( 27.49607050420000220, -67.46050995630001523, 1.934818144049999855 ) ) ;
#15092 = EDGE_LOOP ( 'NONE', ( #26621, #27335, #17658, #667 ) ) ;
#15093 = CARTESIAN_POINT ( 'NONE',  ( -12.47289874709933244, -69.87861895799714773, -24.46965691794827791 ) ) ;
#15094 = CARTESIAN_POINT ( 'NONE',  ( -20.15691507911455105, -95.46331366771129012, 10.39344740093203612 ) ) ;
#15095 = ORIENTED_EDGE ( 'NONE', *, *, #23777, .T. ) ;
#15096 = CARTESIAN_POINT ( 'NONE',  ( 46.12101806169999918, -73.64067649049998465, -3.912894910599999942 ) ) ;
#15097 = ORIENTED_EDGE ( 'NONE', *, *, #1032, .F. ) ;
#15098 = DIRECTION ( 'NONE',  ( 0.000000000000000000, -1.000000000000000000, 0.000000000000000000 ) ) ;
#15099 = CARTESIAN_POINT ( 'NONE',  ( 19.54737287369999876, -35.65078480380000059, -9.004240688089998557 ) ) ;
#15100 = ADVANCED_FACE ( 'NONE', ( #5005 ), #231, .F. ) ;
#15101 = DIRECTION ( 'NONE',  ( 0.4794255386042059475, 0.000000000000000000, 0.8775825618903710934 ) ) ;
#15102 = CARTESIAN_POINT ( 'NONE',  ( -29.79635530287253786, -92.50000267096076811, -0.5908530661228191816 ) ) ;
#15103 = CARTESIAN_POINT ( 'NONE',  ( -20.35840514350000063, -92.54807930229999613, -20.35479784810000226 ) ) ;
#15104 = CARTESIAN_POINT ( 'NONE',  ( 4.426600958609999879E-15, -84.50000000000000000, 43.75000000000000000 ) ) ;
#15105 = ORIENTED_EDGE ( 'NONE', *, *, #27519, .T. ) ;
#15106 = CARTESIAN_POINT ( 'NONE',  ( -22.25450292370000227, -94.89196973819998959, -8.089822570579999095 ) ) ;
#15107 = CARTESIAN_POINT ( 'NONE',  ( 12.12202371060000061, -101.1402801299999936, -9.401285809570000040 ) ) ;
#15108 = DIRECTION ( 'NONE',  ( 0.000000000000000000, -1.000000000000000000, 0.000000000000000000 ) ) ;
#15109 = FACE_OUTER_BOUND ( 'NONE', #4235, .T. ) ;
#15110 = CARTESIAN_POINT ( 'NONE',  ( 29.78875618293655592, -92.66191076884391009, 6.548591290742901805 ) ) ;
#15111 = CARTESIAN_POINT ( 'NONE',  ( -2.572593885869999930, -45.95049971630000130, -24.95132982360000184 ) ) ;
#15112 = VERTEX_POINT ( 'NONE', #20610 ) ;
#15113 = DIRECTION ( 'NONE',  ( 0.000000000000000000, -1.000000000000000000, 0.000000000000000000 ) ) ;
#15114 = FACE_OUTER_BOUND ( 'NONE', #20169, .T. ) ;
#15115 = CARTESIAN_POINT ( 'NONE',  ( -23.78934072751362550, -92.89593097426853774, -19.08709831229086618 ) ) ;
#15116 = CARTESIAN_POINT ( 'NONE',  ( -38.25000000000000000, -65.49083508809999898, 1.947031612740000028 ) ) ;
#15117 = CARTESIAN_POINT ( 'NONE',  ( -0.3895212963913376458, -92.61393927543522864, -30.49754768368999081 ) ) ;
#15118 = CARTESIAN_POINT ( 'NONE',  ( -40.00000000000000000, -69.50000000000000000, 2.464695114669999848E-15 ) ) ;
#15119 = ADVANCED_FACE ( 'NONE', ( #4869 ), #525, .T. ) ;
#15120 = APPLICATION_PROTOCOL_DEFINITION ( 'draft international standard', 'automotive_design', 1998, #23920 ) ;
#15121 = CARTESIAN_POINT ( 'NONE',  ( -11.35954001540000036, -79.50000000000000000, 46.75000000000000000 ) ) ;
#15122 = CARTESIAN_POINT ( 'NONE',  ( -11.64049821129999884, -94.65528426899999204, -20.66308976129999664 ) ) ;
#15123 = ORIENTED_EDGE ( 'NONE', *, *, #24434, .F. ) ;
#15124 = CARTESIAN_POINT ( 'NONE',  ( 4.500000000000000000, 0.000000000000000000, -31.00000000000000000 ) ) ;
#15125 = CARTESIAN_POINT ( 'NONE',  ( 20.85398878019999813, -96.96081042859999854, -2.285143478920000248 ) ) ;
#15126 = ORIENTED_EDGE ( 'NONE', *, *, #6296, .F. ) ;
#15127 = CARTESIAN_POINT ( 'NONE',  ( 21.43682400119999798, -36.68968512050000186, -8.001561263239999278 ) ) ;
#15128 = B_SPLINE_CURVE_WITH_KNOTS ( 'NONE', 3,
 ( #4906, #22241, #13786, #2733, #11587, #20495, #567, #27208, #16112, #9411, #10984 ),
 .UNSPECIFIED., .F., .F.,
 ( 4, 2, 1, 2, 2, 4 ),
 ( 0.000000000000000000, 0.2500000000000506262, 0.3750000000000652256, 0.4375000000000724976, 0.5000000000000797140, 1.000000000000000000 ),
 .UNSPECIFIED. ) ;
#15129 = CARTESIAN_POINT ( 'NONE',  ( -42.71188834620000563, -65.41419836839999391, -0.4550164754569999692 ) ) ;
#15130 = EDGE_LOOP ( 'NONE', ( #25173, #28661, #18209, #16445, #2934 ) ) ;
#15131 = CARTESIAN_POINT ( 'NONE',  ( 13.56355163350000126, -96.34709473579999894, 17.13339730549999729 ) ) ;
#15132 = ADVANCED_FACE ( 'NONE', ( #9372 ), #9407, .T. ) ;
#15133 = CARTESIAN_POINT ( 'NONE',  ( -3.105596691226790274, -66.68383445268185028, -27.13055080113027628 ) ) ;
#15134 = DIRECTION ( 'NONE',  ( 0.3687499999999814260, 0.000000000000000000, -0.9295286103719527793 ) ) ;
#15135 = CARTESIAN_POINT ( 'NONE',  ( -13.17786140689999819, -69.76368794990000310, -23.89400643789999990 ) ) ;
#15136 = CARTESIAN_POINT ( 'NONE',  ( 0.000000000000000000, -16.00000000000000000, 0.000000000000000000 ) ) ;
#15137 = CARTESIAN_POINT ( 'NONE',  ( -10.93050817210000147, -18.61782386119999799, -18.68920581670000303 ) ) ;
#15138 = CIRCLE ( 'NONE', #4950, 8.099999999999999645 ) ;
#15139 = CARTESIAN_POINT ( 'NONE',  ( -40.50000000000000000, -65.63577453799999262, 2.309401076760000393 ) ) ;
#15140 = ORIENTED_EDGE ( 'NONE', *, *, #5783, .F. ) ;
#15141 = DIRECTION ( 'NONE',  ( 0.000000000000000000, -1.000000000000000000, 0.000000000000000000 ) ) ;
#15142 = CARTESIAN_POINT ( 'NONE',  ( 24.95344409500000182, -42.20269670429999564, 1.384270800949999991 ) ) ;
#15143 = CARTESIAN_POINT ( 'NONE',  ( 24.47298445130000033, -67.79480919600000277, 11.04024604620000005 ) ) ;
#15144 = CARTESIAN_POINT ( 'NONE',  ( 9.397459034720000659, -94.89420189139998740, -22.59846365579999983 ) ) ;
#15145 = ORIENTED_EDGE ( 'NONE', *, *, #11672, .T. ) ;
#15146 = CARTESIAN_POINT ( 'NONE',  ( -38.68350751799999898, -73.93831497249999529, 7.318372426699999878 ) ) ;
#15147 = CARTESIAN_POINT ( 'NONE',  ( -10.20110288159999890, -74.50000000000000000, -41.00000000000000000 ) ) ;
#15148 = CARTESIAN_POINT ( 'NONE',  ( -15.61541000649999944, -92.60278524039999581, 23.76968555679999895 ) ) ;
#15149 = DIRECTION ( 'NONE',  ( 1.000000000000000000, 0.000000000000000000, 0.000000000000000000 ) ) ;
#15150 = EDGE_LOOP ( 'NONE', ( #20816, #21433, #13119, #18684 ) ) ;
#15151 = CARTESIAN_POINT ( 'NONE',  ( -38.62788659690000515, -74.00000000000000000, 7.627568735119999666 ) ) ;
#15152 = CARTESIAN_POINT ( 'NONE',  ( 0.2341557092330000256, -101.3878691800000098, -16.10116432410000087 ) ) ;
#15153 = CARTESIAN_POINT ( 'NONE',  ( 8.756289919979998615, -61.98517989029999598, -22.88741420530000070 ) ) ;
#15154 = CARTESIAN_POINT ( 'NONE',  ( 15.70072831049999706, -101.2995922080000071, 2.645407579260000031 ) ) ;
#15155 = CARTESIAN_POINT ( 'NONE',  ( 20.87897399470000082, -58.35063071660000134, 10.71952971249999997 ) ) ;
#15156 = CARTESIAN_POINT ( 'NONE',  ( -11.46863446409999909, -57.40875703270000230, -22.62382275130000053 ) ) ;
#15157 = ORIENTED_EDGE ( 'NONE', *, *, #19056, .T. ) ;
#15158 = ADVANCED_FACE ( 'NONE', ( #18859 ), #819, .T. ) ;
#15159 = CARTESIAN_POINT ( 'NONE',  ( 6.693343950099999162, -101.2251655520000071, 14.77790851379999992 ) ) ;
#15160 = CARTESIAN_POINT ( 'NONE',  ( 14.84965784370000108, -101.2530993010000060, 3.216001622850000352 ) ) ;
#15161 = ORIENTED_EDGE ( 'NONE', *, *, #1413, .T. ) ;
#15162 = CARTESIAN_POINT ( 'NONE',  ( -39.74899213917685614, -65.71745250375693104, -2.207370884887611684 ) ) ;
#15163 = CARTESIAN_POINT ( 'NONE',  ( 21.05681896020000110, -18.50000000000000000, -0.02359534709730000054 ) ) ;
#15164 = ADVANCED_FACE ( 'NONE', ( #12130, #28016 ), #21312, .T. ) ;
#15165 = CARTESIAN_POINT ( 'NONE',  ( 4.123059632000000363, -17.00000000000000000, 7.547210032260000645 ) ) ;
#15166 = ORIENTED_EDGE ( 'NONE', *, *, #3216, .F. ) ;
#15167 = CARTESIAN_POINT ( 'NONE',  ( 3.402843465410000157, -92.87863185420000889, -28.93406916660000050 ) ) ;
#15168 = B_SPLINE_SURFACE_WITH_KNOTS ( 'NONE', 5, 5, ( 
 ( #1788, #12407, #6287, #12546, #1657, #10632, #10359, #23786, #14614 ),
 ( #28160, #21319, #5997, #25842, #5864, #28289, #8321, #12972, #1375 ),
 ( #19546, #10222, #19134, #14878, #15153, #3825, #8061, #24063, #4102 ),
 ( #3966, #8193, #21885, #28434, #16951, #1936, #3683, #21461, #1515 ),
 ( #17223, #26114, #6141, #15014, #23928, #8468, #49, #28578, #22477 ),
 ( #17663, #8894, #9190, #4689, #19688, #26547, #4251, #20130, #2083 ) ),
 .UNSPECIFIED., .F., .F., .F.,
 ( 6, 6 ),
 ( 6, 3, 6 ),
 ( 54.79316133020000024, 65.31895168009999963 ),
 ( 0.000000000000000000, 1.000000000000000000, 2.000000000000000000 ),
 .UNSPECIFIED. ) ;
#15169 = CARTESIAN_POINT ( 'NONE',  ( 6.718680988475624005, -101.3846248971873223, 14.74555885599285432 ) ) ;
#15170 = CARTESIAN_POINT ( 'NONE',  ( 0.000000000000000000, -107.1975888269999899, 0.000000000000000000 ) ) ;
#15171 = PRESENTATION_STYLE_ASSIGNMENT (( #12425 ) ) ;
#15172 = CARTESIAN_POINT ( 'NONE',  ( -5.890277023240000354, -101.2306315440000049, 15.10563561669999899 ) ) ;
#15173 = ORIENTED_EDGE ( 'NONE', *, *, #7173, .T. ) ;
#15174 = CARTESIAN_POINT ( 'NONE',  ( 12.77500156440000012, -92.50000000000000000, 27.05403395929999988 ) ) ;
#15175 = DIRECTION ( 'NONE',  ( 0.4794255386042041156, 0.000000000000000000, 0.8775825618903720926 ) ) ;
#15176 = DIRECTION ( 'NONE',  ( 0.000000000000000000, 1.000000000000000000, 0.000000000000000000 ) ) ;
#15177 = FACE_OUTER_BOUND ( 'NONE', #9609, .T. ) ;
#15178 = CARTESIAN_POINT ( 'NONE',  ( 23.71521856880000101, -60.21977178070000036, -9.629174062080000596 ) ) ;
#15179 = VERTEX_POINT ( 'NONE', #18715 ) ;
#15180 = DIRECTION ( 'NONE',  ( 0.9382669785645009197, 0.000000000000000000, -0.3459119496858159559 ) ) ;
#15181 = CARTESIAN_POINT ( 'NONE',  ( 18.85230044170000241, -18.50000000000000000, -8.028472989549999994 ) ) ;
#15182 = CARTESIAN_POINT ( 'NONE',  ( -36.69998480316156275, -65.09473604209287600, 0.03967052571942218664 ) ) ;
#15183 = CARTESIAN_POINT ( 'NONE',  ( 0.000000000000000000, -10.50000000000000000, 0.000000000000000000 ) ) ;
#15184 = CYLINDRICAL_SURFACE ( 'NONE', #19142, 0.7999999999999998224 ) ;
#15185 = CARTESIAN_POINT ( 'NONE',  ( 7.923301502570000210, -34.91901258349999893, -21.18066442289999785 ) ) ;
#15186 = DIRECTION ( 'NONE',  ( 0.000000000000000000, 1.000000000000000000, 0.000000000000000000 ) ) ;
#15187 = VERTEX_POINT ( 'NONE', #9944 ) ;
#15188 = CARTESIAN_POINT ( 'NONE',  ( 0.1200718050890000055, -93.00000000000000000, -30.49976365090000030 ) ) ;
#15189 = EDGE_CURVE ( 'NONE', #23053, #14525, #9805, .T. ) ;
#15190 = VECTOR ( 'NONE', #18192, 1000.000000000000000 ) ;
#15191 = EDGE_CURVE ( 'NONE', #20122, #5395, #1401, .T. ) ;
#15192 = CIRCLE ( 'NONE', #4046, 4.499999999999997335 ) ;
#15193 = EDGE_LOOP ( 'NONE', ( #1991, #5750, #9044, #22531 ) ) ;
#15194 = CARTESIAN_POINT ( 'NONE',  ( -0.5459402786740000790, -58.79569603810000444, -23.43709083150000083 ) ) ;
#15195 = ADVANCED_FACE ( 'NONE', ( #5448 ), #16654, .T. ) ;
#15196 = CARTESIAN_POINT ( 'NONE',  ( -27.18449005399999763, -93.39359504729999628, -0.5638341530459999307 ) ) ;
#15197 = CARTESIAN_POINT ( 'NONE',  ( -3.835404308829999831, -1.000000000000000000, -7.020660495120000455 ) ) ;
#15198 = EDGE_CURVE ( 'NONE', #23834, #15494, #15797, .T. ) ;
#15199 = CARTESIAN_POINT ( 'NONE',  ( -19.96385611919999903, -52.58489974430013802, 14.40794232450000045 ) ) ;
#15200 = DIRECTION ( 'NONE',  ( 1.000000000000000000, 0.000000000000000000, 0.000000000000000000 ) ) ;
#15201 = CARTESIAN_POINT ( 'NONE',  ( 15.74738730109999807, -100.5717442099999914, 4.327233316820001008 ) ) ;
#15202 = ORIENTED_EDGE ( 'NONE', *, *, #14064, .T. ) ;
#15203 = B_SPLINE_CURVE_WITH_KNOTS ( 'NONE', 5,
 ( #5467, #5609, #9832, #840, #25718, #12012 ),
 .UNSPECIFIED., .F., .F.,
 ( 6, 6 ),
 ( 0.000000000000000000, 1.000000000000000000 ),
 .UNSPECIFIED. ) ;
#15204 = CARTESIAN_POINT ( 'NONE',  ( 21.29161486119999580, -35.09212000590000002, -7.585065879760000129 ) ) ;
#15205 = AXIS2_PLACEMENT_3D ( 'NONE', #25936, #21422, #16911 ) ;
#15206 = CARTESIAN_POINT ( 'NONE',  ( 7.256982118339999843, -74.37144044059999715, -40.28438195579999359 ) ) ;
#15207 = ORIENTED_EDGE ( 'NONE', *, *, #19214, .F. ) ;
#15208 = CARTESIAN_POINT ( 'NONE',  ( -38.25000000000000000, -65.63577453799999262, 1.587713240270000048 ) ) ;
#15209 = ORIENTED_EDGE ( 'NONE', *, *, #1721, .T. ) ;
#15210 = CARTESIAN_POINT ( 'NONE',  ( -9.593141833260000695, -18.50000000000000000, -19.59102626760000376 ) ) ;
#15211 = AXIS2_PLACEMENT_3D ( 'NONE', #133, #2302, #4035 ) ;
#15212 = CARTESIAN_POINT ( 'NONE',  ( 20.87089110420000182, -18.61940624680000056, 9.000567795900000334 ) ) ;
#15213 = DIRECTION ( 'NONE',  ( 1.000000000000000000, 0.000000000000000000, 0.000000000000000000 ) ) ;
#15214 = CARTESIAN_POINT ( 'NONE',  ( -13.36314309979999848, -101.1461874320000049, -9.085681040479999027 ) ) ;
#15215 = ORIENTED_EDGE ( 'NONE', *, *, #16888, .T. ) ;
#15216 = CARTESIAN_POINT ( 'NONE',  ( -15.42268960139999834, -101.6484611540000031, 4.259183661159999801 ) ) ;
#15217 = CARTESIAN_POINT ( 'NONE',  ( -12.51189201029999865, -101.4121386959999995, -9.936042548820001485 ) ) ;
#15218 = CARTESIAN_POINT ( 'NONE',  ( -7.197231212906468834, -73.55557714109660594, 39.12476203138809439 ) ) ;
#15219 = CARTESIAN_POINT ( 'NONE',  ( -7.503851937626710544, -101.2111896144690348, 14.51426051703312048 ) ) ;
#15220 = ORIENTED_EDGE ( 'NONE', *, *, #27116, .F. ) ;
#15221 = CARTESIAN_POINT ( 'NONE',  ( -0.9041074512197031510, -101.6174239712916574, -15.99763876592702161 ) ) ;
#15222 = AXIS2_PLACEMENT_3D ( 'NONE', #17519, #6593, #4544 ) ;
#15223 = CARTESIAN_POINT ( 'NONE',  ( -32.32657687519999712, -74.05570514439999386, -21.80503578329999925 ) ) ;
#15224 = FACE_OUTER_BOUND ( 'NONE', #26888, .T. ) ;
#15225 = ORIENTED_EDGE ( 'NONE', *, *, #19369, .F. ) ;
#15226 = ADVANCED_FACE ( 'NONE', ( #14043 ), #967, .F. ) ;
#15227 = CARTESIAN_POINT ( 'NONE',  ( 19.54973049059999823, -35.76277645470000266, -9.056828148970000214 ) ) ;
#15228 = CARTESIAN_POINT ( 'NONE',  ( -22.53893512686634537, -80.06168502835437550, -32.36019063177454314 ) ) ;
#15229 = EDGE_CURVE ( 'NONE', #10466, #14636, #13944, .T. ) ;
#15230 = EDGE_LOOP ( 'NONE', ( #6564, #10701, #18593, #15018 ) ) ;
#15231 = CIRCLE ( 'NONE', #4088, 11.00000000000000000 ) ;
#15232 = DIRECTION ( 'NONE',  ( 1.000000000000000000, 0.000000000000000000, 0.000000000000000000 ) ) ;
#15233 = FACE_OUTER_BOUND ( 'NONE', #10892, .T. ) ;
#15234 = ORIENTED_EDGE ( 'NONE', *, *, #9895, .F. ) ;
#15235 = CARTESIAN_POINT ( 'NONE',  ( 24.18669557090000310, -93.21603318719999720, 12.26615263310000081 ) ) ;
#15236 = CARTESIAN_POINT ( 'NONE',  ( 46.33376634150000228, -73.97423400449999065, -4.091715457210000295 ) ) ;
#15237 = ORIENTED_EDGE ( 'NONE', *, *, #10481, .F. ) ;
#15238 = FACE_OUTER_BOUND ( 'NONE', #17823, .T. ) ;
#15239 = DIRECTION ( 'NONE',  ( 0.000000000000000000, -1.000000000000000000, 0.000000000000000000 ) ) ;
#15240 = DIRECTION ( 'NONE',  ( 0.000000000000000000, -1.000000000000000000, 0.000000000000000000 ) ) ;
#15241 = CARTESIAN_POINT ( 'NONE',  ( 8.637923669450000119, -37.95659433029999974, -21.89902260000000211 ) ) ;
#15242 = CARTESIAN_POINT ( 'NONE',  ( -11.69905354509999995, -15.49681045920000066, -21.41497386989999896 ) ) ;
#15243 = CARTESIAN_POINT ( 'NONE',  ( -3.383950074269999941, -18.50000000000000000, -22.79034367919999937 ) ) ;
#15244 = VERTEX_POINT ( 'NONE', #4922 ) ;
#15245 = CARTESIAN_POINT ( 'NONE',  ( -26.69328098980000163, -80.00000000000000000, -35.88566914520000495 ) ) ;
#15246 = CARTESIAN_POINT ( 'NONE',  ( 12.77836120849999801, -101.4829589650000088, -9.840357337720000430 ) ) ;
#15247 = CARTESIAN_POINT ( 'NONE',  ( 23.61566649627895487, -60.59571579695727195, -0.5691236615726964487 ) ) ;
#15248 = LINE ( 'NONE', #15400, #23974 ) ;
#15249 = CARTESIAN_POINT ( 'NONE',  ( 27.49607050420000220, -67.46050995630001523, 1.934818144049999855 ) ) ;
#15250 = CARTESIAN_POINT ( 'NONE',  ( 29.91848600129237923, -92.52249206700025752, 5.927436511634884830 ) ) ;
#15251 = DIRECTION ( 'NONE',  ( 0.000000000000000000, -1.000000000000000000, 0.000000000000000000 ) ) ;
#15252 = ORIENTED_EDGE ( 'NONE', *, *, #19596, .F. ) ;
#15253 = VECTOR ( 'NONE', #4575, 1000.000000000000000 ) ;
#15254 = CARTESIAN_POINT ( 'NONE',  ( 10.08508256729999886, -64.24504434620000382, -24.78974309399999854 ) ) ;
#15255 = AXIS2_PLACEMENT_3D ( 'NONE', #3057, #11912, #5369 ) ;
#15256 = DIRECTION ( 'NONE',  ( 0.000000000000000000, 1.000000000000000000, 0.000000000000000000 ) ) ;
#15257 = CARTESIAN_POINT ( 'NONE',  ( -38.25000000000000000, -65.14977478849999670, 2.684678751729999480 ) ) ;
#15258 = CARTESIAN_POINT ( 'NONE',  ( -0.07760674669443720641, -92.74292563041224469, -30.49990831637531841 ) ) ;
#15259 = DIRECTION ( 'NONE',  ( 1.000000000000000000, 0.000000000000000000, 0.000000000000000000 ) ) ;
#15260 = EDGE_CURVE ( 'NONE', #21937, #8977, #21385, .T. ) ;
#15261 = DIRECTION ( 'NONE',  ( 1.000000000000000000, 0.000000000000000000, 0.000000000000000000 ) ) ;
#15262 = B_SPLINE_CURVE_WITH_KNOTS ( 'NONE', 3,
 ( #7954, #10112, #21221, #14506, #5622, #9985, #5203, #1273, #27653, #23544 ),
 .UNSPECIFIED., .F., .F.,
 ( 4, 2, 2, 2, 4 ),
 ( 0.000000000000000000, 0.2500000000000000000, 0.5000000000000000000, 0.7500000000000000000, 1.000000000000000000 ),
 .UNSPECIFIED. ) ;
#15263 = ADVANCED_FACE ( 'NONE', ( #7119 ), #11454, .F. ) ;
#15264 = CARTESIAN_POINT ( 'NONE',  ( 7.120909764619999412E-15, -73.00000000000000000, 40.00000000000000000 ) ) ;
#15265 = EDGE_CURVE ( 'NONE', #8148, #23453, #14567, .T. ) ;
#15266 = ORIENTED_EDGE ( 'NONE', *, *, #2484, .F. ) ;
#15267 = CARTESIAN_POINT ( 'NONE',  ( 17.52693722629999939, -99.56347590660000435, 0.9950084100439999801 ) ) ;
#15268 = ORIENTED_EDGE ( 'NONE', *, *, #26160, .F. ) ;
#15269 = CARTESIAN_POINT ( 'NONE',  ( 20.42801697140000172, -35.85629042629999219, -8.882126403010001781 ) ) ;
#15270 = CARTESIAN_POINT ( 'NONE',  ( 7.685455900877268931, -18.85523520683459964, -20.50116745598906220 ) ) ;
#15271 = ORIENTED_EDGE ( 'NONE', *, *, #18934, .T. ) ;
#15272 = DIRECTION ( 'NONE',  ( 1.000000000000000000, 0.000000000000000000, 0.000000000000000000 ) ) ;
#15273 = CIRCLE ( 'NONE', #24635, 7.250000000000000000 ) ;
#15274 = AXIS2_PLACEMENT_3D ( 'NONE', #18450, #7377, #16241 ) ;
#15275 = DIRECTION ( 'NONE',  ( 1.000000000000000000, 0.000000000000000000, 0.000000000000000000 ) ) ;
#15276 = DIRECTION ( 'NONE',  ( 0.7071067811865475727, 0.000000000000000000, -0.7071067811865475727 ) ) ;
#15277 = CARTESIAN_POINT ( 'NONE',  ( -20.34966500099999820, -94.63958447440001009, 12.21934330610000075 ) ) ;
#15278 = CARTESIAN_POINT ( 'NONE',  ( -29.61792381641411609, -92.58347372262699082, 7.282077114717079525 ) ) ;
#15279 = CARTESIAN_POINT ( 'NONE',  ( 11.86655840719999944, -101.3150700380000018, -11.10431293650000129 ) ) ;
#15280 = EDGE_LOOP ( 'NONE', ( #28039, #16262, #22942, #18403 ) ) ;
#15281 = CARTESIAN_POINT ( 'NONE',  ( 8.799313986089998707, -92.58502644590001296, -27.24229809290000048 ) ) ;
#15282 = CARTESIAN_POINT ( 'NONE',  ( 23.04132486059999962, -42.26701801500000499, 0.3804478350989999869 ) ) ;
#15283 = CARTESIAN_POINT ( 'NONE',  ( 23.84115441240000166, -68.12125821070000598, 11.66698334899999878 ) ) ;
#15284 = CARTESIAN_POINT ( 'NONE',  ( 39.13694367177480160, -73.55869875168333749, 7.198781031945556741 ) ) ;
#15285 = ORIENTED_EDGE ( 'NONE', *, *, #5714, .F. ) ;
#15286 = DIRECTION ( 'NONE',  ( 0.3390050494208429743, 0.7071067811866730279, 0.6205445805637129775 ) ) ;
#15287 = CARTESIAN_POINT ( 'NONE',  ( -13.24502126470000007, -92.50000050830000475, 26.90831906640000071 ) ) ;
#15288 = CARTESIAN_POINT ( 'NONE',  ( 0.000000000000000000, -77.00000000000000000, -40.00000000000000000 ) ) ;
#15289 = ORIENTED_EDGE ( 'NONE', *, *, #16657, .F. ) ;
#15290 = CARTESIAN_POINT ( 'NONE',  ( -26.77683864449999973, -19.40000000000000213, -49.01467436490000296 ) ) ;
#15291 = CIRCLE ( 'NONE', #2785, 1.999999999999998224 ) ;
#15292 = CARTESIAN_POINT ( 'NONE',  ( 0.7146172134730000014, -100.5717442099999914, -16.31546742289999941 ) ) ;
#15293 = CARTESIAN_POINT ( 'NONE',  ( 24.55236475814571406, -74.19409854689706663, -30.49148208431322971 ) ) ;
#15294 = CARTESIAN_POINT ( 'NONE',  ( -41.00000000000000000, -74.50000000000000000, -10.20110288159999890 ) ) ;
#15295 = DIRECTION ( 'NONE',  ( 0.000000000000000000, 1.000000000000000000, 0.000000000000000000 ) ) ;
#15296 = CARTESIAN_POINT ( 'NONE',  ( -11.07869211709999924, -49.85663837269999732, -20.93251907349999641 ) ) ;
#15297 = ORIENTED_EDGE ( 'NONE', *, *, #11780, .F. ) ;
#15298 = AXIS2_PLACEMENT_3D ( 'NONE', #5604, #17092, #7932 ) ;
#15299 = AXIS2_PLACEMENT_3D ( 'NONE', #20821, #7715, #14397 ) ;
#15300 = EDGE_CURVE ( 'NONE', #14266, #14123, #2606, .T. ) ;
#15301 = CARTESIAN_POINT ( 'NONE',  ( 6.946330496749999917, -99.58396362730000817, 15.91260158950000303 ) ) ;
#15302 = CARTESIAN_POINT ( 'NONE',  ( 15.61840456410000044, -101.6484611540000031, 3.474703039729999610 ) ) ;
#15303 = CARTESIAN_POINT ( 'NONE',  ( -4.740443671060163844, -96.36359510251583060, 21.42699769422113576 ) ) ;
#15304 = EDGE_CURVE ( 'NONE', #1181, #914, #25133, .T. ) ;
#15305 = ADVANCED_FACE ( 'NONE', ( #13354 ), #24184, .T. ) ;
#15306 = ORIENTED_EDGE ( 'NONE', *, *, #4377, .F. ) ;
#15307 = CARTESIAN_POINT ( 'NONE',  ( -17.38751286079999758, -93.83676151480000271, 17.80995846940000149 ) ) ;
#15308 = CARTESIAN_POINT ( 'NONE',  ( 22.97338017759999929, -18.50000000000000000, 2.313460506620000245 ) ) ;
#15309 = CARTESIAN_POINT ( 'NONE',  ( 16.08037959500000014, -111.0000000000000000, 2.354223078750000031 ) ) ;
#15310 = CARTESIAN_POINT ( 'NONE',  ( 9.370934950629999705, -94.71481161159999829, -22.48431492339999949 ) ) ;
#15311 = CARTESIAN_POINT ( 'NONE',  ( 19.82451678549999841, -19.46527880160000024, -8.815774675060000121 ) ) ;
#15312 = CARTESIAN_POINT ( 'NONE',  ( -7.318372426699999878, -73.93831497249999529, -38.68350751799999898 ) ) ;
#15313 = CARTESIAN_POINT ( 'NONE',  ( 0.000000000000000000, -11.00000000000000000, 0.000000000000000000 ) ) ;
#15314 = ORIENTED_EDGE ( 'NONE', *, *, #21014, .T. ) ;
#15315 = CARTESIAN_POINT ( 'NONE',  ( 27.26688910437447433, -72.05982473802319532, -11.73839635661862779 ) ) ;
#15316 = DIRECTION ( 'NONE',  ( 0.000000000000000000, 1.000000000000000000, 0.000000000000000000 ) ) ;
#15317 = ORIENTED_EDGE ( 'NONE', *, *, #21706, .T. ) ;
#15318 = FACE_OUTER_BOUND ( 'NONE', #10990, .T. ) ;
#15319 = CARTESIAN_POINT ( 'NONE',  ( 26.62516505820000035, -92.99999854809999533, -10.15609451739999969 ) ) ;
#15320 = CONICAL_SURFACE ( 'NONE', #27483, 21.99999999999999645, 0.03490658503990158590 ) ;
#15321 = AXIS2_PLACEMENT_3D ( 'NONE', #16272, #12043, #25609 ) ;
#15322 = CARTESIAN_POINT ( 'NONE',  ( -1.025805314019999859, -101.2459394079999981, -15.92129411310000009 ) ) ;
#15323 = EDGE_CURVE ( 'NONE', #5628, #22108, #20833, .T. ) ;
#15324 = CARTESIAN_POINT ( 'NONE',  ( 22.85308509809999933, -18.50000000000000000, 2.011281980869999764 ) ) ;
#15325 = DIRECTION ( 'NONE',  ( 0.000000000000000000, -1.000000000000000000, 0.000000000000000000 ) ) ;
#15326 = CARTESIAN_POINT ( 'NONE',  ( -20.26146926273735005, -92.62800705144270808, -22.79754751928403067 ) ) ;
#15327 = VERTEX_POINT ( 'NONE', #22999 ) ;
#15328 = CARTESIAN_POINT ( 'NONE',  ( -15.16614058569999912, -101.1716787529999948, 4.188334258429999402 ) ) ;
#15329 = CARTESIAN_POINT ( 'NONE',  ( -13.60716892229999964, -18.50000000000000000, 19.16900036430000043 ) ) ;
#15330 = DIRECTION ( 'NONE',  ( 0.4794255386042040601, 0.000000000000000000, 0.8775825618903720926 ) ) ;
#15331 = B_SPLINE_CURVE_WITH_KNOTS ( 'NONE', 3,
 ( #9351, #1087, #20742, #13730, #9639, #18253, #25261, #18546, #27442, #14177, #23071, #3116, #11968, #20886, #10597, #8033, #8438, #5968, #23757, #21163, #5702, #27850, #14584, #23486, #23343, #18970, #10465, #7900, #16777, #6112, #3799, #23615 ),
 .UNSPECIFIED., .F., .F.,
 ( 4, 2, 1, 1, 1, 2, 2, 2, 1, 1, 1, 2, 2, 2, 1, 1, 1, 1, 2, 2, 4 ),
 ( 0.000000000000000000, 0.1249999999999596434, 0.1874999999999354128, 0.2187499999999232558, 0.2343749999999195366, 0.2421874999999176770, 0.2499999999999158173, 0.3749999999999181211, 0.4374999999999232281, 0.4687499999999258371, 0.4843749999999192868, 0.4921874999999237277, 0.4999999999999282796, 0.6249999999999982236, 0.6875000000000333067, 0.7187500000000596190, 0.7343750000000742739, 0.7421875000000782707, 0.7460937500000784928, 0.7500000000000788258, 1.000000000000000000 ),
 .UNSPECIFIED. ) ;
#15332 = CARTESIAN_POINT ( 'NONE',  ( 11.86655840719999944, -101.3150700380000018, -11.10431293650000129 ) ) ;
#15333 = CARTESIAN_POINT ( 'NONE',  ( -12.02996277529999958, -67.03347986180000362, -24.13052248920000054 ) ) ;
#15334 = FACE_OUTER_BOUND ( 'NONE', #6064, .T. ) ;
#15335 = CARTESIAN_POINT ( 'NONE',  ( 7.585065630090000788, -35.09211962219999492, -21.29161487800000074 ) ) ;
#15336 = CARTESIAN_POINT ( 'NONE',  ( 26.70978129881138230, -93.15741110562996141, 10.33020051488120750 ) ) ;
#15337 = EDGE_LOOP ( 'NONE', ( #19855, #26371, #18389, #18841 ) ) ;
#15338 = CARTESIAN_POINT ( 'NONE',  ( -10.37349633357829148, -18.49999964046208945, -22.33837851017446852 ) ) ;
#15340 = CARTESIAN_POINT ( 'NONE',  ( -39.23121085047505829, -63.24880261863123820, 2.464586564592250895 ) ) ;
#15339 = APPLICATION_CONTEXT ( 'automotive_design' ) ;
#15341 = AXIS2_PLACEMENT_3D ( 'NONE', #9508, #18411, #27299 ) ;
#15342 = ORIENTED_EDGE ( 'NONE', *, *, #1713, .T. ) ;
#15343 = CIRCLE ( 'NONE', #27509, 57.73884739369999863 ) ;
#15344 = CARTESIAN_POINT ( 'NONE',  ( -13.85849003780000110, -57.40875665010000262, 21.24403944460000204 ) ) ;
#15345 = CARTESIAN_POINT ( 'NONE',  ( -25.36533297769999962, -93.60790942680000626, -2.267491459940000009 ) ) ;
#15346 = CARTESIAN_POINT ( 'NONE',  ( -19.57724474209999954, -53.84184168659999870, 12.63913840070000028 ) ) ;
#15347 = FACE_OUTER_BOUND ( 'NONE', #5812, .T. ) ;
#15348 = CARTESIAN_POINT ( 'NONE',  ( 16.30510774900000115, -100.5229262450000078, 4.375467603060000599 ) ) ;
#15349 = ORIENTED_EDGE ( 'NONE', *, *, #25882, .F. ) ;
#15350 = CARTESIAN_POINT ( 'NONE',  ( 21.45961748159999871, -35.74888769769999897, -7.120077148630000075 ) ) ;
#15351 = CARTESIAN_POINT ( 'NONE',  ( 7.440489808669999761, -74.12477399289998914, -39.45579440659999904 ) ) ;
#15352 = VERTEX_POINT ( 'NONE', #25466 ) ;
#15353 = CARTESIAN_POINT ( 'NONE',  ( -10.20110288159999890, -74.00000000000000000, 41.00000000000000000 ) ) ;
#15354 = DIRECTION ( 'NONE',  ( -1.000000000000000000, 0.000000000000000000, -2.168404344971021884E-15 ) ) ;
#15355 = ADVANCED_FACE ( 'NONE', ( #25333 ), #9291, .T. ) ;
#15356 = CARTESIAN_POINT ( 'NONE',  ( 19.94171510720000029, -39.36519097769999576, 10.90497833400000083 ) ) ;
#15357 = AXIS2_PLACEMENT_3D ( 'NONE', #15440, #22466, #22614 ) ;
#15358 = FACE_BOUND ( 'NONE', #2339, .T. ) ;
#15360 = EDGE_CURVE ( 'NONE', #2790, #27403, #6197, .T. ) ;
#15359 = AXIS2_PLACEMENT_3D ( 'NONE', #18656, #25364, #27254 ) ;
#15361 = VECTOR ( 'NONE', #1360, 1000.000000000000000 ) ;
#15362 = CARTESIAN_POINT ( 'NONE',  ( -2.876553231629999985, -91.50000000000000000, -5.265495371340000119 ) ) ;
#15363 = CARTESIAN_POINT ( 'NONE',  ( -26.60903970598167589, -26.59999999999999787, -48.70752046822583736 ) ) ;
#15364 = CARTESIAN_POINT ( 'NONE',  ( 19.97576656849999921, -36.00000000000000000, -19.97576656849999921 ) ) ;
#15365 = ORIENTED_EDGE ( 'NONE', *, *, #976, .F. ) ;
#15366 = FACE_OUTER_BOUND ( 'NONE', #3811, .T. ) ;
#15367 = CARTESIAN_POINT ( 'NONE',  ( -11.90690755189999983, -100.8685038539999965, -10.28167538419999971 ) ) ;
#15368 = EDGE_CURVE ( 'NONE', #21532, #16418, #21851, .T. ) ;
#15369 = CARTESIAN_POINT ( 'NONE',  ( -7.218759893172350672, -73.62114148037002792, 39.32637163715104833 ) ) ;
#15370 = CARTESIAN_POINT ( 'NONE',  ( -40.70731707320000226, -74.50000000000000000, -7.215414233289999757 ) ) ;
#15371 = ORIENTED_EDGE ( 'NONE', *, *, #22553, .F. ) ;
#15372 = ADVANCED_FACE ( 'NONE', ( #21101 ), #13000, .F. ) ;
#15373 = FACE_OUTER_BOUND ( 'NONE', #9054, .T. ) ;
#15374 = CARTESIAN_POINT ( 'NONE',  ( -22.22906643760000023, -79.50000000000000000, -32.83566815539999340 ) ) ;
#15375 = VERTEX_POINT ( 'NONE', #18910 ) ;
#15376 = DIRECTION ( 'NONE',  ( 1.000000000000000000, 0.000000000000000000, 0.000000000000000000 ) ) ;
#15377 = FACE_OUTER_BOUND ( 'NONE', #6495, .T. ) ;
#15378 = AXIS2_PLACEMENT_3D ( 'NONE', #17803, #11662, #11217 ) ;
#15379 = DIRECTION ( 'NONE',  ( 0.4794255386042041156, 0.000000000000000000, 0.8775825618903722036 ) ) ;
#15380 = AXIS2_PLACEMENT_3D ( 'NONE', #24590, #20215, #28797 ) ;
#15381 = ORIENTED_EDGE ( 'NONE', *, *, #26512, .T. ) ;
#15382 = AXIS2_PLACEMENT_3D ( 'NONE', #23033, #25365, #11637 ) ;
#15383 = CARTESIAN_POINT ( 'NONE',  ( -19.23676770128301072, -97.09204376972030559, 7.281157557458501906 ) ) ;
#15384 = ORIENTED_EDGE ( 'NONE', *, *, #3504, .F. ) ;
#15385 = CARTESIAN_POINT ( 'NONE',  ( 19.58568502800000033, -94.54719310899999130, 13.61987657130000073 ) ) ;
#15386 = CARTESIAN_POINT ( 'NONE',  ( -4.500000000000000000, -11.00000000000000000, -40.50000000000000000 ) ) ;
#15387 = ORIENTED_EDGE ( 'NONE', *, *, #28312, .F. ) ;
#15388 = CARTESIAN_POINT ( 'NONE',  ( -42.06204301354549102, -65.70971443686121916, 0.8617459228010823091 ) ) ;
#15389 = CARTESIAN_POINT ( 'NONE',  ( -42.83545581620172271, -63.17361819572899151, -0.3836747634055225897 ) ) ;
#15390 = EDGE_LOOP ( 'NONE', ( #13495, #23648, #17785, #19918, #292, #19491 ) ) ;
#15391 = DIRECTION ( 'NONE',  ( 0.000000000000000000, 1.000000000000000000, 0.000000000000000000 ) ) ;
#15392 = CARTESIAN_POINT ( 'NONE',  ( 12.52134826220000186, -101.6311724339999927, -9.982697054739999132 ) ) ;
#15393 = EDGE_CURVE ( 'NONE', #20440, #7086, #16711, .T. ) ;
#15394 = CARTESIAN_POINT ( 'NONE',  ( -16.52453304470000006, -93.48569568799999274, -21.60249615600000084 ) ) ;
#15395 = VERTEX_POINT ( 'NONE', #27790 ) ;
#15396 = EDGE_CURVE ( 'NONE', #22021, #3254, #12453, .T. ) ;
#15397 = CARTESIAN_POINT ( 'NONE',  ( -1.229530056899999835, -101.0685849509999912, -16.04536266459999894 ) ) ;
#15398 = CARTESIAN_POINT ( 'NONE',  ( 12.91798634669999934, -101.2251655520000071, -9.813921847190000491 ) ) ;
#15399 = DIRECTION ( 'NONE',  ( 1.000000000000000000, 0.000000000000000000, 0.000000000000000000 ) ) ;
#15400 = CARTESIAN_POINT ( 'NONE',  ( 7.181689689069999716, -101.1889999979999999, 15.80535034289999885 ) ) ;
#15401 = AXIS2_PLACEMENT_3D ( 'NONE', #19292, #8209, #6447 ) ;
#15402 = DIRECTION ( 'NONE',  ( 0.000000000000000000, 1.000000000000000000, 0.000000000000000000 ) ) ;
#15403 = ADVANCED_FACE ( 'NONE', ( #5218 ), #7831, .F. ) ;
#15404 = TOROIDAL_SURFACE ( 'NONE', #9380, 30.50381168839999901, 2.000000000000000000 ) ;
#15405 = CARTESIAN_POINT ( 'NONE',  ( 6.717799458580000049, -84.50000000000000000, -40.65853658540000026 ) ) ;
#15406 = CARTESIAN_POINT ( 'NONE',  ( -18.03086174180000256, -18.61827554290000108, 12.74382289080000064 ) ) ;
#15407 = ORIENTED_EDGE ( 'NONE', *, *, #3689, .T. ) ;
#15408 = VECTOR ( 'NONE', #2186, 1000.000000000000114 ) ;
#15409 = ADVANCED_FACE ( 'NONE', ( #9714 ), #12326, .T. ) ;
#15410 = DIRECTION ( 'NONE',  ( 1.000000000000000000, 0.000000000000000000, 0.000000000000000000 ) ) ;
#15411 = CARTESIAN_POINT ( 'NONE',  ( 9.099148368520435071, -57.44066836785145114, -22.71963871380157585 ) ) ;
#15412 = CARTESIAN_POINT ( 'NONE',  ( -24.38380614478478847, -92.52249206704190954, -18.32158033856656942 ) ) ;
#15413 = CARTESIAN_POINT ( 'NONE',  ( 22.04985193179999925, -18.50000000000000000, 8.586826782579999318 ) ) ;
#15414 = CYLINDRICAL_SURFACE ( 'NONE', #10341, 7.250000000000004441 ) ;
#15415 = B_SPLINE_SURFACE_WITH_KNOTS ( 'NONE', 5, 5, ( 
 ( #511, #8909, #9357, #15616, #4702, #10935 ),
 ( #22336, #9061, #24819, #17675, #4858, #2382 ),
 ( #6602, #13737, #24669, #11239, #24372, #20146 ),
 ( #11073, #22637, #2676, #26415, #22189, #13583 ),
 ( #2230, #62, #17820, #215, #17965, #6898 ),
 ( #15763, #22936, #11833, #4991, #20594, #5145 ) ),
 .UNSPECIFIED., .F., .F., .F.,
 ( 6, 6 ),
 ( 6, 6 ),
 ( 7.179431123180000540, 23.44689954740000104 ),
 ( 0.000000000000000000, 0.5000000000000000000 ),
 .UNSPECIFIED. ) ;
#15416 = DIRECTION ( 'NONE',  ( 1.000000000000000000, 0.000000000000000000, 0.000000000000000000 ) ) ;
#15417 = DIRECTION ( 'NONE',  ( 0.000000000000000000, -1.000000000000000000, 0.000000000000000000 ) ) ;
#15418 = ORIENTED_EDGE ( 'NONE', *, *, #26851, .F. ) ;
#15419 = ADVANCED_BREP_SHAPE_REPRESENTATION ( '', ( #25670, #26433 ), #17143 ) ;
#15420 = DIRECTION ( 'NONE',  ( 0.000000000000000000, -1.000000000000000000, 0.000000000000000000 ) ) ;
#15421 = CARTESIAN_POINT ( 'NONE',  ( 15.98190521330000102, -101.1461869959999973, 2.387867047529999898 ) ) ;
#15422 = ORIENTED_EDGE ( 'NONE', *, *, #11303, .T. ) ;
#15423 = CARTESIAN_POINT ( 'NONE',  ( -13.46276276162894625, -19.23820061190542319, 20.39865906485581704 ) ) ;
#15424 = DIRECTION ( 'NONE',  ( 1.000000000000000000, 0.000000000000000000, 0.000000000000000000 ) ) ;
#15425 = EDGE_LOOP ( 'NONE', ( #5217, #5611, #9464, #15365, #14006, #24694 ) ) ;
#15426 = AXIS2_PLACEMENT_3D ( 'NONE', #1342, #27587, #16769 ) ;
#15427 = CARTESIAN_POINT ( 'NONE',  ( 15.64667777420000050, -100.8816835080000089, 2.154424203329999621 ) ) ;
#15428 = ORIENTED_EDGE ( 'NONE', *, *, #18963, .F. ) ;
#15429 = CARTESIAN_POINT ( 'NONE',  ( -8.825292394359999903, -96.19637846910001144, -20.90069174230000115 ) ) ;
#15430 = ADVANCED_FACE ( 'NONE', ( #7566 ), #9860, .F. ) ;
#15431 = CARTESIAN_POINT ( 'NONE',  ( 4.500000000000000000, -12.50000000000000000, -40.50000000000000000 ) ) ;
#15432 = CARTESIAN_POINT ( 'NONE',  ( -16.97615606580000147, -99.73367829289999520, 3.380302814300000236 ) ) ;
#15433 = CARTESIAN_POINT ( 'NONE',  ( -10.73461461720000010, -18.50000000000000000, -18.44891755279999757 ) ) ;
#15434 = CARTESIAN_POINT ( 'NONE',  ( 25.04292896270000313, -70.80052042889998631, 11.98325363630000062 ) ) ;
#15435 = ORIENTED_EDGE ( 'NONE', *, *, #26924, .T. ) ;
#15436 = ADVANCED_FACE ( 'NONE', ( #25749 ), #21367, .T. ) ;
#15437 = CARTESIAN_POINT ( 'NONE',  ( 10.37782365410000018, -92.68419354089999729, -25.56315968380000214 ) ) ;
#15438 = CARTESIAN_POINT ( 'NONE',  ( 24.82569795559999903, -49.81670839440000265, 1.385523269080000119 ) ) ;
#15439 = CARTESIAN_POINT ( 'NONE',  ( 23.84247938200000050, -66.23852357979998828, 10.90989094220000055 ) ) ;
#15440 = CARTESIAN_POINT ( 'NONE',  ( 0.000000000000000000, -26.29689110869999880, 0.000000000000000000 ) ) ;
#15441 = EDGE_LOOP ( 'NONE', ( #22174, #12942, #26162, #11081 ) ) ;
#15442 = DIRECTION ( 'NONE',  ( 0.000000000000000000, 1.000000000000000000, 0.000000000000000000 ) ) ;
#15443 = CARTESIAN_POINT ( 'NONE',  ( -15.13518098839999837, -92.64783192670000744, 25.02785625110000112 ) ) ;
#15444 = CARTESIAN_POINT ( 'NONE',  ( -40.00000000000000000, -74.00000000000000000, 3.466919520389999841E-15 ) ) ;
#15445 = ORIENTED_EDGE ( 'NONE', *, *, #25096, .F. ) ;
#15446 = ADVANCED_FACE ( 'NONE', ( #26172, #6340 ), #23693, .T. ) ;
#15447 = CARTESIAN_POINT ( 'NONE',  ( 27.57043804909999807, -69.70329313409999372, 1.768595993289999946 ) ) ;
#15448 = PRESENTATION_LAYER_ASSIGNMENT (  '', '', ( #28040 ) ) ;
#15449 = CARTESIAN_POINT ( 'NONE',  ( 0.4780712722559999905, -101.0403179300000005, -15.46279129750000081 ) ) ;
#15450 = DIRECTION ( 'NONE',  ( 0.09756097560976997873, 0.000000000000000000, -0.9952295494196653491 ) ) ;
#15451 = CARTESIAN_POINT ( 'NONE',  ( -12.41806785860000062, -68.06111301600000729, -23.59935346929999866 ) ) ;
#15452 = CIRCLE ( 'NONE', #19194, 52.20000000000000284 ) ;
#15453 = VERTEX_POINT ( 'NONE', #17129 ) ;
#15454 = CARTESIAN_POINT ( 'NONE',  ( 28.31887119405866216, -72.09394576601212634, 1.343104835225076066 ) ) ;
#15455 = FACE_OUTER_BOUND ( 'NONE', #8312, .T. ) ;
#15456 = ORIENTED_EDGE ( 'NONE', *, *, #5933, .T. ) ;
#15457 = CARTESIAN_POINT ( 'NONE',  ( -13.18661234450000030, -92.50000000000000000, 26.85581265420000108 ) ) ;
#15458 = DIRECTION ( 'NONE',  ( 0.000000000000000000, -1.000000000000000000, 0.000000000000000000 ) ) ;
#15459 = CARTESIAN_POINT ( 'NONE',  ( -4.643934244949999623, -95.55433883409999396, 22.13027033890000084 ) ) ;
#15460 = EDGE_LOOP ( 'NONE', ( #19485, #22565, #15834 ) ) ;
#15461 = FACE_OUTER_BOUND ( 'NONE', #23512, .T. ) ;
#15462 = DIRECTION ( 'NONE',  ( 1.000000000000000000, 0.000000000000000000, 0.000000000000000000 ) ) ;
#15463 = VERTEX_POINT ( 'NONE', #10683 ) ;
#15464 = CARTESIAN_POINT ( 'NONE',  ( 26.81987566912476240, -72.54457018766687781, -10.76610228402119773 ) ) ;
#15465 = VECTOR ( 'NONE', #9169, 1000.000000000000000 ) ;
#15466 = CARTESIAN_POINT ( 'NONE',  ( -12.03978574509999966, -15.50000000000000000, -22.03867997850000293 ) ) ;
#15467 = EDGE_CURVE ( 'NONE', #24004, #19902, #13161, .T. ) ;
#15468 = ORIENTED_EDGE ( 'NONE', *, *, #11016, .T. ) ;
#15469 = CARTESIAN_POINT ( 'NONE',  ( 9.067969494719999801, -35.79825198000000341, -19.85338805880000024 ) ) ;
#15470 = AXIS2_PLACEMENT_3D ( 'NONE', #6611, #10802, #17535 ) ;
#15471 = CARTESIAN_POINT ( 'NONE',  ( -40.00000000000000000, -69.50000000000000000, 0.000000000000000000 ) ) ;
#15472 = EDGE_CURVE ( 'NONE', #914, #28370, #22817, .T. ) ;
#15473 = CARTESIAN_POINT ( 'NONE',  ( 9.385332722619999402, -98.68450614990000247, 16.47661810339999988 ) ) ;
#15474 = FACE_OUTER_BOUND ( 'NONE', #8205, .T. ) ;
#15475 = CARTESIAN_POINT ( 'NONE',  ( -38.71641001238787538, -73.63089972761061119, -7.135467692469587675 ) ) ;
#15476 = CARTESIAN_POINT ( 'NONE',  ( -19.63244573686088046, -92.50638022835023833, -23.34176391067345691 ) ) ;
#15477 = ORIENTED_EDGE ( 'NONE', *, *, #13175, .F. ) ;
#15478 = CARTESIAN_POINT ( 'NONE',  ( -15.38823321699999980, -101.6484610359999863, 4.383952149800000697 ) ) ;
#15479 = CARTESIAN_POINT ( 'NONE',  ( 28.70651795192725686, -71.31133772027507689, 2.849249339242819090 ) ) ;
#15480 = FACE_OUTER_BOUND ( 'NONE', #6183, .T. ) ;
#15481 = EDGE_CURVE ( 'NONE', #20759, #26341, #26458, .T. ) ;
#15482 = CARTESIAN_POINT ( 'NONE',  ( -36.74089255422700262, -65.11704020643968249, 0.1219423816524388415 ) ) ;
#15483 = B_SPLINE_SURFACE_WITH_KNOTS ( 'NONE', 5, 5, ( 
 ( #560, #9404, #24274, #26611, #19893, #4313 ),
 ( #22097, #8812, #11290, #2285, #20050, #113 ),
 ( #20197, #27870, #1236, #1651, #7240, #21184 ),
 ( #10487, #12683, #16802, #23637, #10353, #11733 ),
 ( #3676, #16253, #27342, #14738, #7917, #25006 ),
 ( #707, #5196, #5041, #9559, #23778, #25695 ),
 ( #5722, #22832, #10075, #16106, #13931, #25835 ),
 ( #1510, #14604, #5990, #23509, #3546, #21592 ),
 ( #5857, #14870, #25966, #19264, #28153, #12537 ),
 ( #2877, #21455, #12401, #19400, #18990, #20649 ),
 ( #23365, #21313, #8186, #3819, #18458, #1367 ),
 ( #7388, #25163, #3409, #14078, #12274, #10214 ) ),
 .UNSPECIFIED., .F., .F., .F.,
 ( 6, 3, 3, 6 ),
 ( 6, 6 ),
 ( 1.565586965149999839E-10, 0.8942904027689999591, 1.389395125490000105, 1.857837794129999942 ),
 ( 0.000000000000000000, 0.5000000000000000000 ),
 .UNSPECIFIED. ) ;
#15484 = AXIS2_PLACEMENT_3D ( 'NONE', #1379, #10225, #28026 ) ;
#15485 = CARTESIAN_POINT ( 'NONE',  ( 13.80626276613105929, -99.96200787833144830, -10.48157719901313456 ) ) ;
#15486 = CARTESIAN_POINT ( 'NONE',  ( -12.07244877390000148, -67.46051290640001241, -24.77968394139999830 ) ) ;
#15487 = CARTESIAN_POINT ( 'NONE',  ( -38.36731331058076933, -65.09474816371883321, -2.867870865955927329 ) ) ;
#15488 = FACE_OUTER_BOUND ( 'NONE', #10664, .T. ) ;
#15489 = CARTESIAN_POINT ( 'NONE',  ( 22.52953341510427521, -94.00303307112771734, 13.14769211859860576 ) ) ;
#15490 = ORIENTED_EDGE ( 'NONE', *, *, #7161, .T. ) ;
#15491 = FACE_OUTER_BOUND ( 'NONE', #24433, .T. ) ;
#15492 = CARTESIAN_POINT ( 'NONE',  ( 7.932078966940000697, -101.4167270020000018, 13.98634163589999879 ) ) ;
#15493 = TOROIDAL_SURFACE ( 'NONE', #24354, 38.75000000000000000, 0.5000000000000000000 ) ;
#15494 = VERTEX_POINT ( 'NONE', #19600 ) ;
#15495 = ADVANCED_FACE ( 'NONE', ( #10537 ), #7336, .T. ) ;
#15496 = CARTESIAN_POINT ( 'NONE',  ( -13.70187040939999967, -57.41946935120000006, 20.98050596210000052 ) ) ;
#15497 = CARTESIAN_POINT ( 'NONE',  ( -1.347567224549999887, -65.01950563030000296, -25.09408215860000269 ) ) ;
#15498 = CARTESIAN_POINT ( 'NONE',  ( 6.114061450890000415, -93.00000000000000000, -13.40104985119999981 ) ) ;
#15499 = CARTESIAN_POINT ( 'NONE',  ( -20.08102625940000507, -57.43018266629999857, 14.46712152350000125 ) ) ;
#15500 = DIRECTION ( 'NONE',  ( 0.000000000000000000, -1.000000000000000000, 0.000000000000000000 ) ) ;
#15501 = CARTESIAN_POINT ( 'NONE',  ( 9.385332722619999402, -98.68450614990000247, 16.47661810339999988 ) ) ;
#15502 = VERTEX_POINT ( 'NONE', #17716 ) ;
#15503 = VECTOR ( 'NONE', #404, 1000.000000000000000 ) ;
#15504 = DIRECTION ( 'NONE',  ( -0.8775825618903722036, 0.000000000000000000, 0.4794255386042041156 ) ) ;
#15505 = CARTESIAN_POINT ( 'NONE',  ( -13.36314236379999976, -101.1461869959999973, -9.085682662689999134 ) ) ;
#15506 = EDGE_LOOP ( 'NONE', ( #24288, #26070, #14315, #20382, #13092, #27388, #13599 ) ) ;
#15507 = CARTESIAN_POINT ( 'NONE',  ( 7.929587929925636658, -92.54893169919635909, 29.45117466200463952 ) ) ;
#15508 = EDGE_CURVE ( 'NONE', #5350, #20540, #3728, .T. ) ;
#15509 = CARTESIAN_POINT ( 'NONE',  ( 0.000000000000000000, -19.40000000000000213, 0.000000000000000000 ) ) ;
#15510 = CARTESIAN_POINT ( 'NONE',  ( 22.61645189879999762, -32.66150190460000147, 10.07608658779999899 ) ) ;
#15511 = TOROIDAL_SURFACE ( 'NONE', #3005, 7.000000000000000000, 1.000000000000000000 ) ;
#15512 = DIRECTION ( 'NONE',  ( 1.000000000000000000, 0.000000000000000000, 0.000000000000000000 ) ) ;
#15513 = CARTESIAN_POINT ( 'NONE',  ( 24.47773556059999933, -92.99999932709999939, -17.01937738950000067 ) ) ;
#15514 = CARTESIAN_POINT ( 'NONE',  ( 19.45586016849999922, -18.85467989400000022, 10.05010111100000003 ) ) ;
#15515 = CARTESIAN_POINT ( 'NONE',  ( -32.71604765022082972, -79.95000206843607771, -22.50489820171189592 ) ) ;
#15516 = CARTESIAN_POINT ( 'NONE',  ( -16.09756696615421134, -99.27923575797652234, 7.463221687748802680 ) ) ;
#15517 = EDGE_LOOP ( 'NONE', ( #3501, #25677, #12998, #10536 ) ) ;
#15518 = CARTESIAN_POINT ( 'NONE',  ( -41.00000000000000000, -84.00000000000000000, -10.20110288159999890 ) ) ;
#15519 = CARTESIAN_POINT ( 'NONE',  ( 8.988996100299999625, -34.66800400750000222, -19.43643858049999906 ) ) ;
#15520 = CARTESIAN_POINT ( 'NONE',  ( -12.37368733949999999, -100.1512121650000040, -11.12496841619999977 ) ) ;
#15521 = CARTESIAN_POINT ( 'NONE',  ( 22.20230814393099550, -19.49660179756074996, 9.763414323654941995 ) ) ;
#15522 = CARTESIAN_POINT ( 'NONE',  ( -40.70731707320000226, -74.50000000000000000, -7.215414233289999757 ) ) ;
#15523 = ORIENTED_EDGE ( 'NONE', *, *, #8956, .F. ) ;
#15524 = AXIS2_PLACEMENT_3D ( 'NONE', #26005, #14910, #23677 ) ;
#15525 = VECTOR ( 'NONE', #4608, 1000.000000000000114 ) ;
#15526 = DIRECTION ( 'NONE',  ( 0.000000000000000000, -1.000000000000000000, 0.000000000000000000 ) ) ;
#15527 = ORIENTED_EDGE ( 'NONE', *, *, #19523, .T. ) ;
#15528 = MANIFOLD_SOLID_BREP ( 'O-Ring Seal', #20743 ) ;
#15529 = EDGE_CURVE ( 'NONE', #26111, #813, #4746, .T. ) ;
#15530 = CARTESIAN_POINT ( 'NONE',  ( -6.665307709260000379, -101.1889999979999999, -13.13558364449999871 ) ) ;
#15531 = EDGE_CURVE ( 'NONE', #5075, #3752, #23731, .T. ) ;
#15532 = CARTESIAN_POINT ( 'NONE',  ( 24.87134706483404401, -38.85105898717574036, 1.395915593889689665 ) ) ;
#15533 = MECHANICAL_DESIGN_GEOMETRIC_PRESENTATION_REPRESENTATION (  '', ( #20699 ), #9977 ) ;
#15534 = CARTESIAN_POINT ( 'NONE',  ( 12.80177023699999950, -92.76842269019999776, 27.50696703210000038 ) ) ;
#15535 = ORIENTED_EDGE ( 'NONE', *, *, #22960, .T. ) ;
#15536 = CARTESIAN_POINT ( 'NONE',  ( 0.000000000000000000, -92.50000000000000000, 0.000000000000000000 ) ) ;
#15537 = CARTESIAN_POINT ( 'NONE',  ( -19.96511697432906374, -95.86227943297046750, 9.608863210890680406 ) ) ;
#15538 = CIRCLE ( 'NONE', #1618, 0.3500000000000003664 ) ;
#15539 = ORIENTED_EDGE ( 'NONE', *, *, #9610, .T. ) ;
#15540 = CARTESIAN_POINT ( 'NONE',  ( -25.25510951461192732, -94.35876167706931028, -2.968759144345000323 ) ) ;
#15541 = CARTESIAN_POINT ( 'NONE',  ( 21.82349187340000185, -93.59856831130001353, 12.95706236810000078 ) ) ;
#15542 = CARTESIAN_POINT ( 'NONE',  ( 46.52944179779999700, -74.00708935479998729, -3.668904617159999937 ) ) ;
#15543 = EDGE_CURVE ( 'NONE', #18513, #22875, #18, .T. ) ;
#15544 = ORIENTED_EDGE ( 'NONE', *, *, #6241, .T. ) ;
#15545 = CARTESIAN_POINT ( 'NONE',  ( 16.44117558850142302, -94.63960343439929090, 17.12038290499986459 ) ) ;
#15546 = FACE_OUTER_BOUND ( 'NONE', #23437, .T. ) ;
#15547 = TOROIDAL_SURFACE ( 'NONE', #27681, 55.85192378860000417, 0.3499999999999999778 ) ;
#15548 = LINE ( 'NONE', #17756, #14594 ) ;
#15549 = CARTESIAN_POINT ( 'NONE',  ( -14.18321254710000012, -94.09272382180000704, -21.64669162210000053 ) ) ;
#15550 = DIRECTION ( 'NONE',  ( 0.4794255386042036715, 0.000000000000000000, 0.8775825618903724257 ) ) ;
#15551 = ORIENTED_EDGE ( 'NONE', *, *, #16222, .F. ) ;
#15552 = CARTESIAN_POINT ( 'NONE',  ( -41.76420911575942796, -63.33604893236084621, -1.392788587596942351 ) ) ;
#15553 = CARTESIAN_POINT ( 'NONE',  ( 14.01704999690000086, -99.70407914540000149, -9.961568965490000593 ) ) ;
#15554 = CARTESIAN_POINT ( 'NONE',  ( -21.73289126959999962, -74.33689811570000927, -32.66619185449999918 ) ) ;
#15555 = CARTESIAN_POINT ( 'NONE',  ( 0.000000000000000000, -10.50000000000000000, 0.000000000000000000 ) ) ;
#15556 = DIRECTION ( 'NONE',  ( 1.000000000000000000, 0.000000000000000000, 0.000000000000000000 ) ) ;
#15557 = CARTESIAN_POINT ( 'NONE',  ( -38.25000000000000000, -65.11307468787711628, 2.760557608143826780 ) ) ;
#15558 = CARTESIAN_POINT ( 'NONE',  ( 7.315281843798212336, -74.28334043001960652, -40.00441865863449209 ) ) ;
#15559 = VERTEX_POINT ( 'NONE', #17861 ) ;
#15560 = CARTESIAN_POINT ( 'NONE',  ( -7.325370793560000315, -19.50000000000000000, -24.94672208400000102 ) ) ;
#15561 = CIRCLE ( 'NONE', #13732, 30.50000000000000000 ) ;
#15562 = CARTESIAN_POINT ( 'NONE',  ( 7.066909182079999852, -57.47855601759999900, -22.26662627820000040 ) ) ;
#15563 = DIRECTION ( 'NONE',  ( 0.000000000000000000, 1.000000000000000000, 0.000000000000000000 ) ) ;
#15564 = DIRECTION ( 'NONE',  ( 0.000000000000000000, 0.000000000000000000, 1.000000000000000000 ) ) ;
#15565 = CARTESIAN_POINT ( 'NONE',  ( 27.68682485439999752, -20.89999999999999858, 50.68039294919999804 ) ) ;
#15566 = CARTESIAN_POINT ( 'NONE',  ( 27.68682485439999752, -36.20000000000000284, 50.68039294919999804 ) ) ;
#15567 = PRODUCT_DEFINITION_CONTEXT ( 'detailed design', #16306, 'design' ) ;
#15568 = B_SPLINE_CURVE_WITH_KNOTS ( 'NONE', 5,
 ( #22648, #2690, #14868, #3544, #25965, #3272, #12272, #966, #16943, #25546, #5989, #10211 ),
 .UNSPECIFIED., .F., .F.,
 ( 6, 3, 3, 6 ),
 ( 0.000000000000000000, 0.2521440085671421416, 0.5186391376505576911, 1.000000000000000000 ),
 .UNSPECIFIED. ) ;
#15569 = PRODUCT_CONTEXT ( 'NONE', #12005, 'mechanical' ) ;
#15570 = CIRCLE ( 'NONE', #4418, 6.749999999999999112 ) ;
#15571 = EDGE_CURVE ( 'NONE', #10144, #2030, #26023, .T. ) ;
#15572 = DIRECTION ( 'NONE',  ( 0.000000000000000000, -1.000000000000000000, 0.000000000000000000 ) ) ;
#15573 = ADVANCED_FACE ( 'NONE', ( #19016 ), #25439, .F. ) ;
#15574 = ORIENTED_EDGE ( 'NONE', *, *, #17899, .F. ) ;
#15575 = CARTESIAN_POINT ( 'NONE',  ( 16.58537890990000108, -94.98812477769999418, 16.93952572510000110 ) ) ;
#15576 = CARTESIAN_POINT ( 'NONE',  ( 16.03761577559999907, -101.2306310700000012, 2.381277126570000569 ) ) ;
#15577 = ORIENTED_EDGE ( 'NONE', *, *, #13034, .F. ) ;
#15578 = DIRECTION ( 'NONE',  ( 1.000000000000000000, 0.000000000000000000, 0.000000000000000000 ) ) ;
#15579 = DIRECTION ( 'NONE',  ( 1.000000000000000000, 0.000000000000000000, 0.000000000000000000 ) ) ;
#15580 = EDGE_CURVE ( 'NONE', #8526, #15179, #12421, .T. ) ;
#15581 = VERTEX_POINT ( 'NONE', #18881 ) ;
#15582 = CARTESIAN_POINT ( 'NONE',  ( 15.58784579500000156, -100.8733988930000010, 2.070706579690000382 ) ) ;
#15583 = EDGE_CURVE ( 'NONE', #6867, #25460, #15203, .T. ) ;
#15584 = ORIENTED_EDGE ( 'NONE', *, *, #13110, .F. ) ;
#15585 = CARTESIAN_POINT ( 'NONE',  ( -11.21687034500000024, -94.79905218150000223, -20.68493743190000345 ) ) ;
#15586 = B_SPLINE_CURVE_WITH_KNOTS ( 'NONE', 3,
 ( #13671, #15697, #2318, #15552, #13074, #22132 ),
 .UNSPECIFIED., .F., .F.,
 ( 4, 2, 4 ),
 ( 0.000000000000000000, 0.5000000000000000000, 1.000000000000000000 ),
 .UNSPECIFIED. ) ;
#15587 = CARTESIAN_POINT ( 'NONE',  ( 23.35417726369999869, -57.47855601759999900, -0.5711878298099999363 ) ) ;
#15588 = DIRECTION ( 'NONE',  ( 0.4794255386042036715, 0.000000000000000000, 0.8775825618903723147 ) ) ;
#15589 = DIRECTION ( 'NONE',  ( 1.000000000000000000, 0.000000000000000000, 0.000000000000000000 ) ) ;
#15590 = CARTESIAN_POINT ( 'NONE',  ( -11.34376786329999831, -18.85523522049999912, -18.72653253400000040 ) ) ;
#15591 = CARTESIAN_POINT ( 'NONE',  ( -12.09704001540000107, -74.50000000000000000, 47.10905722069999513 ) ) ;
#15592 = ORIENTED_EDGE ( 'NONE', *, *, #23468, .T. ) ;
#15593 = DIRECTION ( 'NONE',  ( 0.000000000000000000, -1.000000000000000000, 0.000000000000000000 ) ) ;
#15594 = LINE ( 'NONE', #15735, #27527 ) ;
#15595 = CARTESIAN_POINT ( 'NONE',  ( 0.000000000000000000, -65.07443093669999712, 0.000000000000000000 ) ) ;
#15596 = CARTESIAN_POINT ( 'NONE',  ( -12.82502785340713025, -92.59735406121865253, 27.67253584333921879 ) ) ;
#15597 = ORIENTED_EDGE ( 'NONE', *, *, #16653, .T. ) ;
#15598 = CARTESIAN_POINT ( 'NONE',  ( -20.45998242170000125, -52.56313962710000709, 14.78974999389999923 ) ) ;
#15599 = CARTESIAN_POINT ( 'NONE',  ( -14.04679603149999956, -92.49999866209999766, 25.86342652180000101 ) ) ;
#15600 = DIRECTION ( 'NONE',  ( 0.4794255386042040601, 0.000000000000000000, 0.8775825618903719816 ) ) ;
#15601 = ORIENTED_EDGE ( 'NONE', *, *, #11336, .T. ) ;
#15602 = CARTESIAN_POINT ( 'NONE',  ( 27.81679767680000026, -70.78636603370000557, 1.651879667569999821 ) ) ;
#15603 = CARTESIAN_POINT ( 'NONE',  ( 0.4195603051590000021, -100.9364576079999978, -15.94533468339999871 ) ) ;
#15604 = CARTESIAN_POINT ( 'NONE',  ( 26.46383138103869470, -74.36567512596400320, -28.96817324696392859 ) ) ;
#15605 = CARTESIAN_POINT ( 'NONE',  ( 21.58746088380000216, -36.00000000000000000, -10.99658662490000083 ) ) ;
#15606 = CARTESIAN_POINT ( 'NONE',  ( -11.05123306399999983, -49.83808240359999786, -21.57293782270000193 ) ) ;
#15607 = DIRECTION ( 'NONE',  ( -1.135974695539999883E-15, 0.000000000000000000, -1.000000000000000000 ) ) ;
#15608 = DIRECTION ( 'NONE',  ( -0.9952295494196657932, 0.000000000000000000, -0.09756097560976527416 ) ) ;
#15609 = EDGE_CURVE ( 'NONE', #11090, #1612, #14228, .T. ) ;
#15610 = CARTESIAN_POINT ( 'NONE',  ( 28.44652200260433972, -92.82529299094275643, 11.00206337811066959 ) ) ;
#15611 = CARTESIAN_POINT ( 'NONE',  ( 8.630545616070000037, -99.09990215500000943, 16.29201985859999624 ) ) ;
#15612 = CARTESIAN_POINT ( 'NONE',  ( 7.315286554507971495, -74.28332971671856910, 40.00438978216653396 ) ) ;
#15613 = EDGE_LOOP ( 'NONE', ( #17320, #9414 ) ) ;
#15614 = AXIS2_PLACEMENT_3D ( 'NONE', #27651, #11889, #855 ) ;
#15615 = LINE ( 'NONE', #4990, #14371 ) ;
#15616 = CARTESIAN_POINT ( 'NONE',  ( 26.48196640509999966, -92.56168957700000988, 13.31191097970000037 ) ) ;
#15617 = EDGE_CURVE ( 'NONE', #20540, #24483, #24638, .T. ) ;
#15618 = CARTESIAN_POINT ( 'NONE',  ( 23.24501621210006874, -19.48040731474316445, 1.335160801108107309 ) ) ;
#15619 = CARTESIAN_POINT ( 'NONE',  ( -7.515932239300000539, -100.7707614970000094, 13.96005744500000034 ) ) ;
#15620 = VERTEX_POINT ( 'NONE', #22821 ) ;
#15621 = CARTESIAN_POINT ( 'NONE',  ( 26.81408956065956062, -72.66570736699186739, -10.40602720322819508 ) ) ;
#15622 = CARTESIAN_POINT ( 'NONE',  ( 9.115928523210000023, -35.98566164980000082, -20.35866484339999616 ) ) ;
#15623 = CARTESIAN_POINT ( 'NONE',  ( 21.21808891099999883, -34.59820414320000026, -7.670974023059999425 ) ) ;
#15624 = ORIENTED_EDGE ( 'NONE', *, *, #27264, .F. ) ;
#15625 = CARTESIAN_POINT ( 'NONE',  ( 7.609509498830000496, -99.68121713349998458, 15.96225029060000011 ) ) ;
#15626 = FACE_OUTER_BOUND ( 'NONE', #462, .T. ) ;
#15627 = CARTESIAN_POINT ( 'NONE',  ( -12.22851712105154220, -19.47229981159569334, 19.17184709748261540 ) ) ;
#15628 = CARTESIAN_POINT ( 'NONE',  ( -5.703789389510000696, -95.94970068800000718, -21.79542136019999887 ) ) ;
#15629 = CARTESIAN_POINT ( 'NONE',  ( -19.92269764396411347, -92.54893169919635909, -23.09407223288071620 ) ) ;
#15630 = ORIENTED_EDGE ( 'NONE', *, *, #24442, .F. ) ;
#15631 = CARTESIAN_POINT ( 'NONE',  ( -15.48258886210000185, -101.2306315829999903, 4.813006563600000121 ) ) ;
#15632 = CARTESIAN_POINT ( 'NONE',  ( 28.53389931306142913, -70.75059817112114047, 2.680123202356653245 ) ) ;
#15633 = CARTESIAN_POINT ( 'NONE',  ( 15.04667461659597016, -95.25682781127063947, 17.31483459787338575 ) ) ;
#15634 = DIRECTION ( 'NONE',  ( 0.000000000000000000, -1.000000000000000000, 0.000000000000000000 ) ) ;
#15635 = DIRECTION ( 'NONE',  ( -0.2287893768880245038, 0.000000000000000000, 0.9734759478401042720 ) ) ;
#15636 = CARTESIAN_POINT ( 'NONE',  ( -38.52200237161242313, -65.13413837704243292, -2.874048270801004890 ) ) ;
#15637 = CARTESIAN_POINT ( 'NONE',  ( 24.70277711335754844, -93.45279863401688658, -11.97073514444795173 ) ) ;
#15638 = CARTESIAN_POINT ( 'NONE',  ( -14.25726283530000060, -18.50000000000000000, 19.69500409140000130 ) ) ;
#15639 = ORIENTED_EDGE ( 'NONE', *, *, #21358, .F. ) ;
#15640 = CARTESIAN_POINT ( 'NONE',  ( 36.29172713509999681, -75.00000018049999539, -14.94947828099999931 ) ) ;
#15641 = CARTESIAN_POINT ( 'NONE',  ( 8.185346603670000221, -101.3150705270000032, 14.03998133939999882 ) ) ;
#15642 = EDGE_CURVE ( 'NONE', #26855, #25651, #10094, .T. ) ;
#15643 = CARTESIAN_POINT ( 'NONE',  ( -14.36794459300000071, -65.11374573150000344, 21.98892381860000000 ) ) ;
#15644 = CARTESIAN_POINT ( 'NONE',  ( -0.7543003842240000312, -101.1889999979999999, -16.73300722909999649 ) ) ;
#15645 = CARTESIAN_POINT ( 'NONE',  ( 30.00028607799999847, -92.50000000000000000, 5.498439345520000465 ) ) ;
#15646 = B_SPLINE_CURVE_WITH_KNOTS ( 'NONE', 5,
 ( #13938, #20347, #5049, #416, #9266, #9412 ),
 .UNSPECIFIED., .F., .F.,
 ( 6, 6 ),
 ( 0.000000000000000000, 1.000000000000000000 ),
 .UNSPECIFIED. ) ;
#15647 = CARTESIAN_POINT ( 'NONE',  ( -26.83792192550000166, -92.99570653130000153, -0.4343255661159999836 ) ) ;
#15648 = CARTESIAN_POINT ( 'NONE',  ( -19.88433733760000166, -55.05574748869999979, 12.10004687989999894 ) ) ;
#15649 = EDGE_CURVE ( 'NONE', #12485, #19902, #11724, .T. ) ;
#15650 = DIRECTION ( 'NONE',  ( 0.000000000000000000, -1.000000000000000000, 0.000000000000000000 ) ) ;
#15651 = CARTESIAN_POINT ( 'NONE',  ( 16.51865411080000001, -99.74726900420000675, 4.630948717549999927 ) ) ;
#15652 = EDGE_LOOP ( 'NONE', ( #12924, #20510, #17780, #22239 ) ) ;
#15653 = CARTESIAN_POINT ( 'NONE',  ( -7.318372426699999878, -73.93831497249999529, -38.68350751799999898 ) ) ;
#15654 = CARTESIAN_POINT ( 'NONE',  ( 29.28066344122883535, -74.33029147470158193, -26.09360328796791961 ) ) ;
#15655 = CARTESIAN_POINT ( 'NONE',  ( 7.268564243840000216, -74.08838618790001362, -39.96405812909999611 ) ) ;
#15656 = ORIENTED_EDGE ( 'NONE', *, *, #157, .T. ) ;
#15657 = CARTESIAN_POINT ( 'NONE',  ( 8.472395020760000506, -37.95144078679999922, -21.79230213740000011 ) ) ;
#15658 = CARTESIAN_POINT ( 'NONE',  ( 28.69894246159999796, -72.00000000000000000, -10.33698060819999931 ) ) ;
#15659 = LINE ( 'NONE', #11429, #21426 ) ;
#15660 = CARTESIAN_POINT ( 'NONE',  ( 22.47717647029999810, -39.30675845300000049, 9.993032863299999846 ) ) ;
#15661 = DIRECTION ( 'NONE',  ( -0.000000000000000000, 1.000000000000000000, 0.000000000000000000 ) ) ;
#15662 = CARTESIAN_POINT ( 'NONE',  ( 23.68384408339999680, -92.51542729400000553, -18.51872027609999805 ) ) ;
#15663 = CARTESIAN_POINT ( 'NONE',  ( 20.16274462490000019, -18.85622860559999836, 9.471810047709999125 ) ) ;
#15664 = CARTESIAN_POINT ( 'NONE',  ( 8.888943361349999961, -68.13650396850000845, -25.01879546389999831 ) ) ;
#15665 = CARTESIAN_POINT ( 'NONE',  ( -16.23097981328315953, -99.08289723854821318, 7.775255002977575991 ) ) ;
#15666 = B_SPLINE_SURFACE_WITH_KNOTS ( 'NONE', 5, 5, ( 
 ( #16254, #25164, #5197, #13781, #20650, #18159 ),
 ( #16406, #2727, #5482, #9560, #11884, #849 ),
 ( #27058, #561, #7100, #24867, #11582, #18314 ),
 ( #5042, #22833, #18608, #2878, #708, #5758 ),
 ( #21771, #1546, #14644, #23541, #12720, #26152 ),
 ( #8088, #8219, #10522, #21348, #3577, #21632 ),
 ( #6175, #9979, #26000, #1682, #12437, #28187 ),
 ( #10389, #1407, #17111, #7814, #28323, #12308 ),
 ( #19436, #18893, #17255, #19028, #5893, #8354 ) ),
 .UNSPECIFIED., .F., .F., .F.,
 ( 6, 3, 6 ),
 ( 6, 6 ),
 ( 5.946593705439999766, 13.87007241820000125, 18.04675716799999918 ),
 ( 0.000000000000000000, 2.000000000000000000 ),
 .UNSPECIFIED. ) ;
#15667 = VERTEX_POINT ( 'NONE', #22972 ) ;
#15668 = CARTESIAN_POINT ( 'NONE',  ( 8.185346967789998374, -101.3150701389999995, 14.03998109830000018 ) ) ;
#15669 = DIRECTION ( 'NONE',  ( -0.9704142011833034598, 0.000000000000000000, 0.2414462220490750932 ) ) ;
#15670 = CARTESIAN_POINT ( 'NONE',  ( -12.08161827610000039, -100.4808658609999981, -10.82458641699999902 ) ) ;
#15671 = CARTESIAN_POINT ( 'NONE',  ( 9.475766568499999210, -36.00000000000000000, -19.97576656850000276 ) ) ;
#15672 = CARTESIAN_POINT ( 'NONE',  ( 23.08464880861777146, -62.66433083247308389, -7.365532055905221753 ) ) ;
#15673 = VERTEX_POINT ( 'NONE', #9682 ) ;
#15674 = CARTESIAN_POINT ( 'NONE',  ( 26.64643508839107255, -92.66777315148785021, -14.83972869400399652 ) ) ;
#15675 = ORIENTED_EDGE ( 'NONE', *, *, #18102, .T. ) ;
#15676 = EDGE_CURVE ( 'NONE', #7443, #13918, #1679, .T. ) ;
#15677 = CYLINDRICAL_SURFACE ( 'NONE', #16039, 20.64285714289998452 ) ;
#15678 = AXIS2_PLACEMENT_3D ( 'NONE', #9917, #27720, #16767 ) ;
#15679 = DIRECTION ( 'NONE',  ( 0.000000000000000000, -1.000000000000000000, 0.000000000000000000 ) ) ;
#15680 = CARTESIAN_POINT ( 'NONE',  ( 24.70618715508873109, -32.10667435201317943, 1.410068405398430924 ) ) ;
#15681 = CARTESIAN_POINT ( 'NONE',  ( 12.80359094900000017, -92.84292109160000450, 27.53777204920000088 ) ) ;
#15682 = B_SPLINE_CURVE_WITH_KNOTS ( 'NONE', 3,
 ( #12456, #25469, #5500, #28073, #21369, #14392, #10270, #19183, #5911, #14793, #23695, #21943, #17569, #24121, #19743, #15657 ),
 .UNSPECIFIED., .F., .F.,
 ( 4, 2, 2, 1, 1, 1, 1, 2, 2, 4 ),
 ( 0.000000000000000000, 0.2500000000001303402, 0.3750000000002007838, 0.4375000000002303158, 0.4687500000002451372, 0.4843750000002524647, 0.4921875000002564615, 0.4960937500002529088, 0.5000000000002493561, 1.000000000000000000 ),
 .UNSPECIFIED. ) ;
#15683 = ORIENTED_EDGE ( 'NONE', *, *, #22711, .T. ) ;
#15684 = VERTEX_POINT ( 'NONE', #1260 ) ;
#15685 = CARTESIAN_POINT ( 'NONE',  ( -27.01692611455537829, -93.59825775049449703, -0.6446940546961127394 ) ) ;
#15686 = CARTESIAN_POINT ( 'NONE',  ( -13.12175661516558911, -71.04369398208616815, -24.58936394580375406 ) ) ;
#15687 = DIRECTION ( 'NONE',  ( 0.000000000000000000, -1.000000000000000000, 0.000000000000000000 ) ) ;
#15688 = VERTEX_POINT ( 'NONE', #21070 ) ;
#15689 = CARTESIAN_POINT ( 'NONE',  ( -38.55000000000000426, -63.07912966450000880, -2.857883832489999776 ) ) ;
#15690 = CARTESIAN_POINT ( 'NONE',  ( -22.48295016580000194, -80.00863955980000242, -32.56379889600000155 ) ) ;
#15691 = CIRCLE ( 'NONE', #3174, 10.00000000000000000 ) ;
#15692 = AXIS2_PLACEMENT_3D ( 'NONE', #4708, #11537, #26718 ) ;
#15693 = FACE_OUTER_BOUND ( 'NONE', #22294, .T. ) ;
#15694 = DIRECTION ( 'NONE',  ( 0.000000000000000000, -1.000000000000000000, 0.000000000000000000 ) ) ;
#15695 = CARTESIAN_POINT ( 'NONE',  ( -26.69293917519999937, -16.10310889129999623, -48.86109741659999628 ) ) ;
#15696 = ORIENTED_EDGE ( 'NONE', *, *, #12267, .T. ) ;
#15697 = CARTESIAN_POINT ( 'NONE',  ( -41.85858414364702185, -63.35633004489629627, -1.124464781979226613 ) ) ;
#15698 = CARTESIAN_POINT ( 'NONE',  ( -2.617290931510000362, -61.32329206099999652, -25.60467908629999911 ) ) ;
#15699 = CARTESIAN_POINT ( 'NONE',  ( -39.18053445169999804, -73.62955962630000784, 7.219524535890000649 ) ) ;
#15700 = CARTESIAN_POINT ( 'NONE',  ( -22.13232332860000184, -74.41849501830000690, -32.73892504640000567 ) ) ;
#15701 = CARTESIAN_POINT ( 'NONE',  ( -0.8479692466189999722, -57.47815920199999340, -23.34776748810000058 ) ) ;
#15702 = AXIS2_PLACEMENT_3D ( 'NONE', #19694, #8898, #8617 ) ;
#15703 = CARTESIAN_POINT ( 'NONE',  ( 7.426814492070000107, -35.28814190290000141, -21.34788074219999743 ) ) ;
#15704 = FACE_OUTER_BOUND ( 'NONE', #15193, .T. ) ;
#15705 = CARTESIAN_POINT ( 'NONE',  ( -18.59146871949999991, -19.47458110719999880, 13.41216391400000063 ) ) ;
#15706 = VERTEX_POINT ( 'NONE', #10096 ) ;
#15707 = CARTESIAN_POINT ( 'NONE',  ( -11.98151724899999948, -93.50556391630000519, -23.51195765390000147 ) ) ;
#15708 = B_SPLINE_CURVE_WITH_KNOTS ( 'NONE', 3,
 ( #16890, #19208, #12220, #21130, #1188, #5807, #17022, #18938, #27822, #25909, #25640, #5669, #14548, #14687, #23582, #5936, #4184, #28650, #24444, #16091, #15383, #28798, #6227, #1870, #21968, #4338, #6672, #10566, #4479, #2019, #28517, #10858, #20474, #15537, #1726, #19910, #545, #24993, #4039, #15094, #24152, #24294, #21678, #13059 ),
 .UNSPECIFIED., .F., .F.,
 ( 4, 2, 2, 1, 1, 1, 1, 2, 2, 2, 2, 1, 1, 1, 1, 1, 2, 2, 2, 2, 1, 1, 1, 1, 1, 2, 2, 2, 4 ),
 ( 0.000000000000000000, 0.1250000000000717204, 0.1875000000001076916, 0.2187500000001266487, 0.2343750000001371681, 0.2421875000001423583, 0.2460937500001457723, 0.2480468750001485201, 0.2500000000001512679, 0.3750000000003486100, 0.4375000000004475309, 0.4687500000004961587, 0.4843750000005205281, 0.4921875000005318523, 0.4960937500005382361, 0.4980468750005404011, 0.4990234375005415668, 0.5000000000005426770, 0.6250000000004817258, 0.6875000000004524159, 0.7187500000004385381, 0.7343750000004307665, 0.7421875000004278800, 0.7460937500004269918, 0.7480468750004258816, 0.7490234375004246603, 0.7500000000004234391, 0.8750000000002117195, 1.000000000000000000 ),
 .UNSPECIFIED. ) ;
#15709 = CARTESIAN_POINT ( 'NONE',  ( 20.36016146999999776, -74.00000000000000000, -32.97008227039999895 ) ) ;
#15710 = CARTESIAN_POINT ( 'NONE',  ( -24.12489041853968885, -92.59735406125496127, -18.66119614963135120 ) ) ;
#15711 = CARTESIAN_POINT ( 'NONE',  ( -50.00000000000000000, -15.00000000000000000, 4.500000000000000000 ) ) ;
#15712 = CARTESIAN_POINT ( 'NONE',  ( 0.000000000000000000, -19.09689110869999951, 0.000000000000000000 ) ) ;
#15713 = CARTESIAN_POINT ( 'NONE',  ( -14.60468409838225234, -101.1900861939869429, 4.477069939566454160 ) ) ;
#15714 = AXIS2_PLACEMENT_3D ( 'NONE', #24992, #544, #18588 ) ;
#15715 = DIRECTION ( 'NONE',  ( 0.1884548733085491812, -2.775557561562891351E-17, 0.9820818503191364179 ) ) ;
#15716 = LINE ( 'NONE', #26967, #23333 ) ;
#15717 = ORIENTED_EDGE ( 'NONE', *, *, #10853, .F. ) ;
#15718 = CARTESIAN_POINT ( 'NONE',  ( 15.64667784240000081, -100.8816831189999874, 2.154425576790000019 ) ) ;
#15719 = EDGE_LOOP ( 'NONE', ( #20602, #21225, #21789, #9546 ) ) ;
#15720 = DIRECTION ( 'NONE',  ( 1.000000000000000000, 0.000000000000000000, 0.000000000000000000 ) ) ;
#15721 = CARTESIAN_POINT ( 'NONE',  ( 9.024080808563812894, -19.23820059856630138, -18.94592219493823038 ) ) ;
#15722 = MANIFOLD_SOLID_BREP ( 'Body', #14679 ) ;
#15723 = VERTEX_POINT ( 'NONE', #8489 ) ;
#15724 = CARTESIAN_POINT ( 'NONE',  ( 30.51745573710000059, -72.51545259190000081, -23.74117753099999817 ) ) ;
#15725 = B_SPLINE_SURFACE_WITH_KNOTS ( 'NONE', 5, 5, ( 
 ( #19462, #14799, #5916, #28350, #8381, #17286 ),
 ( #13039, #26178, #15076, #23985, #17002, #21950 ),
 ( #19610, #12607, #23699, #1853, #4019, #21516 ),
 ( #1575, #10415, #19333, #12881, #21797, #28493 ),
 ( #8531, #6348, #15212, #1997, #13189, #4759 ),
 ( #9259, #6802, #13780, #15663, #24566, #20489 ),
 ( #26911, #17871, #18158, #2587, #11434, #2140 ),
 ( #27201, #20337, #6651, #15514, #270, #27057 ),
 ( #15962, #11131, #22681, #9112, #7099, #4461 ) ),
 .UNSPECIFIED., .F., .F., .F.,
 ( 6, 3, 6 ),
 ( 6, 6 ),
 ( 0.000000000000000000, 2.252774941560000244, 5.576981603820000188 ),
 ( 0.000000000000000000, 1.000000000000000000 ),
 .UNSPECIFIED. ) ;
#15726 = B_SPLINE_CURVE_WITH_KNOTS ( 'NONE', 3,
 ( #26662, #6704, #6849, #2332, #20099, #13689, #164, #15713, #13532, #15865, #19172, #13831 ),
 .UNSPECIFIED., .F., .F.,
 ( 4, 2, 2, 2, 2, 4 ),
 ( 0.000000000000000000, 0.2499999999999875100, 0.3749999999999895639, 0.4999999999999916733, 0.7499999999999957812, 1.000000000000000000 ),
 .UNSPECIFIED. ) ;
#15727 = CARTESIAN_POINT ( 'NONE',  ( 5.725409811050989894, -93.38817447844444075, -27.06492380005755649 ) ) ;
#15728 = DIRECTION ( 'NONE',  ( 0.000000000000000000, 1.000000000000000000, 0.000000000000000000 ) ) ;
#15729 = DIRECTION ( 'NONE',  ( 1.000000000000000000, 0.000000000000000000, 0.000000000000000000 ) ) ;
#15730 = CARTESIAN_POINT ( 'NONE',  ( -10.93437420129999893, -19.18584095090000119, -21.85842446839999909 ) ) ;
#15731 = CARTESIAN_POINT ( 'NONE',  ( 21.59599020914462386, -37.77569117438354596, -8.026336239905948133 ) ) ;
#15732 = ORIENTED_EDGE ( 'NONE', *, *, #21387, .F. ) ;
#15733 = AXIS2_PLACEMENT_3D ( 'NONE', #2858, #6932, #11275 ) ;
#15734 = DIRECTION ( 'NONE',  ( 0.000000000000000000, 1.000000000000000000, 0.000000000000000000 ) ) ;
#15735 = CARTESIAN_POINT ( 'NONE',  ( -26.72663706610000034, -37.96100227850000408, -48.92278099219999632 ) ) ;
#15736 = ADVANCED_FACE ( 'NONE', ( #10650 ), #11873, .T. ) ;
#15737 = CARTESIAN_POINT ( 'NONE',  ( -12.41862539467342508, -92.52048598158050652, 27.85727924331794725 ) ) ;
#15738 = ORIENTED_EDGE ( 'NONE', *, *, #12834, .F. ) ;
#15739 = CARTESIAN_POINT ( 'NONE',  ( 13.12744653600000078, -94.59276292389999696, -19.84842857619999990 ) ) ;
#15740 = DIRECTION ( 'NONE',  ( 0.4794255386042036715, 0.000000000000000000, 0.8775825618903724257 ) ) ;
#15741 = CARTESIAN_POINT ( 'NONE',  ( 15.74335372269999844, -101.6484611540000031, 2.854262350110000401 ) ) ;
#15742 = EDGE_LOOP ( 'NONE', ( #16947, #5815 ) ) ;
#15743 = EDGE_CURVE ( 'NONE', #15688, #3752, #19567, .T. ) ;
#15744 = CARTESIAN_POINT ( 'NONE',  ( -14.86197364899999940, -100.8869795979999964, 4.957594172660000353 ) ) ;
#15745 = CARTESIAN_POINT ( 'NONE',  ( -12.94585355975605445, -101.5555610555526869, -9.402386697501409429 ) ) ;
#15746 = CARTESIAN_POINT ( 'NONE',  ( 0.6332782371249999764, -100.6809449770000100, -16.42402731589999831 ) ) ;
#15747 = DIRECTION ( 'NONE',  ( 0.000000000000000000, -1.000000000000000000, 0.000000000000000000 ) ) ;
#15748 = CARTESIAN_POINT ( 'NONE',  ( 4.534235129290000123E-15, -69.00000000000000000, -36.25000000000000000 ) ) ;
#15749 = EDGE_CURVE ( 'NONE', #18911, #19124, #23609, .T. ) ;
#15750 = EDGE_CURVE ( 'NONE', #4330, #27046, #6888, .T. ) ;
#15751 = DIRECTION ( 'NONE',  ( 1.000000000000000000, 0.000000000000000000, 0.000000000000000000 ) ) ;
#15752 = DIRECTION ( 'NONE',  ( 0.000000000000000000, 1.000000000000000000, 0.000000000000000000 ) ) ;
#15753 = AXIS2_PLACEMENT_3D ( 'NONE', #6527, #19913, #4042 ) ;
#15754 = AXIS2_PLACEMENT_3D ( 'NONE', #15993, #15845, #12165 ) ;
#15755 = AXIS2_PLACEMENT_3D ( 'NONE', #17006, #21248, #23438 ) ;
#15756 = VERTEX_POINT ( 'NONE', #28307 ) ;
#15757 = AXIS2_PLACEMENT_3D ( 'NONE', #28417, #8452, #19256 ) ;
#15758 = CARTESIAN_POINT ( 'NONE',  ( -39.50000000000000000, -65.63577453799999262, -2.309401076760000393 ) ) ;
#15759 = AXIS2_PLACEMENT_3D ( 'NONE', #6163, #4420, #10939 ) ;
#15760 = CARTESIAN_POINT ( 'NONE',  ( 8.137532908689999900, -101.2306311739999956, 14.02341457380000023 ) ) ;
#15761 = ORIENTED_EDGE ( 'NONE', *, *, #18871, .F. ) ;
#15762 = CARTESIAN_POINT ( 'NONE',  ( 7.472970580910000216, -74.00000000000000000, 38.65569705749999940 ) ) ;
#15763 = CARTESIAN_POINT ( 'NONE',  ( 16.58537991969999936, -94.98812656900000206, 16.93952948469999953 ) ) ;
#15764 = CARTESIAN_POINT ( 'NONE',  ( 22.05085473011402186, -19.46454039567884564, -0.1739277095649396365 ) ) ;
#15765 = ORIENTED_EDGE ( 'NONE', *, *, #12301, .F. ) ;
#15766 = DIRECTION ( 'NONE',  ( 0.000000000000000000, -1.000000000000000000, 0.000000000000000000 ) ) ;
#15767 = FACE_OUTER_BOUND ( 'NONE', #3885, .T. ) ;
#15768 = CARTESIAN_POINT ( 'NONE',  ( 8.470925167420000790, -36.97944905069999777, -21.53314064279999940 ) ) ;
#15769 = CARTESIAN_POINT ( 'NONE',  ( 21.31604162444098804, -34.85188264325164198, -7.422259252942775554 ) ) ;
#15770 = DIRECTION ( 'NONE',  ( 0.000000000000000000, -1.000000000000000000, 0.000000000000000000 ) ) ;
#15771 = CARTESIAN_POINT ( 'NONE',  ( 23.98860504829999840, -18.86819686409999974, 1.664881634730000171 ) ) ;
#15772 = CARTESIAN_POINT ( 'NONE',  ( -2.288843675430000335, -97.83383802270000729, -19.83674288659999974 ) ) ;
#15773 = AXIS2_PLACEMENT_3D ( 'NONE', #4974, #13717, #16183 ) ;
#15774 = CARTESIAN_POINT ( 'NONE',  ( 0.000000000000000000, -101.1889999979999999, 0.000000000000000000 ) ) ;
#15775 = EDGE_LOOP ( 'NONE', ( #25010, #19118, #9970, #3458 ) ) ;
#15776 = CARTESIAN_POINT ( 'NONE',  ( -15.15665000090000092, -101.0314213319999936, 4.653947536529999596 ) ) ;
#15777 = FACE_OUTER_BOUND ( 'NONE', #11847, .T. ) ;
#15779 = EDGE_CURVE ( 'NONE', #8106, #13332, #16950, .T. ) ;
#15778 = VECTOR ( 'NONE', #26311, 1000.000000000000000 ) ;
#15780 = AXIS2_PLACEMENT_3D ( 'NONE', #22309, #17943, #9178 ) ;
#15781 = AXIS2_PLACEMENT_3D ( 'NONE', #13327, #26608, #20334 ) ;
#15782 = DIRECTION ( 'NONE',  ( 1.000000000000000000, 0.000000000000000000, 0.000000000000000000 ) ) ;
#15783 = CARTESIAN_POINT ( 'NONE',  ( 21.88811475929999872, -37.33710342420000217, -8.645795876960001181 ) ) ;
#15784 = CARTESIAN_POINT ( 'NONE',  ( -12.05825490610000195, -67.66818692689999182, -24.37625710889999908 ) ) ;
#15785 = CARTESIAN_POINT ( 'NONE',  ( 15.34608781240000042, -101.0356131030000029, 1.995616791270000023 ) ) ;
#15786 = CARTESIAN_POINT ( 'NONE',  ( 25.92294088882810499, -93.25521311087592835, 11.00152434285968361 ) ) ;
#15787 = ORIENTED_EDGE ( 'NONE', *, *, #27291, .T. ) ;
#15788 = EDGE_CURVE ( 'NONE', #26473, #1175, #10239, .T. ) ;
#15789 = CARTESIAN_POINT ( 'NONE',  ( -1.865174681369999824E-14, -11.00000000000000000, 31.00000000000000000 ) ) ;
#15790 = CARTESIAN_POINT ( 'NONE',  ( 8.023929893669999203, -101.0253300669999987, 13.24802822849999906 ) ) ;
#15791 = CARTESIAN_POINT ( 'NONE',  ( -13.58047762579999862, -66.16285484500001246, 21.97899781390000129 ) ) ;
#15792 = CARTESIAN_POINT ( 'NONE',  ( -13.44714549129999881, -61.83339493489999938, 20.99574822410000152 ) ) ;
#15793 = CARTESIAN_POINT ( 'NONE',  ( 7.247546674742445738, -74.11886065931342671, 40.20585889373907662 ) ) ;
#15794 = FACE_OUTER_BOUND ( 'NONE', #27542, .T. ) ;
#15795 = DIRECTION ( 'NONE',  ( 0.000000000000000000, 1.000000000000000000, 0.000000000000000000 ) ) ;
#15796 = CIRCLE ( 'NONE', #21850, 55.67692378859999991 ) ;
#15797 = CIRCLE ( 'NONE', #20477, 29.91857981989999971 ) ;
#15798 = B_SPLINE_CURVE_WITH_KNOTS ( 'NONE', 5,
 ( #823, #11552, #7209, #9666, #13899, #18573, #12134, #25421, #9950 ),
 .UNSPECIFIED., .F., .F.,
 ( 6, 3, 6 ),
 ( 0.000000000000000000, 0.5000000000000000000, 1.000000000000000000 ),
 .UNSPECIFIED. ) ;
#15799 = CARTESIAN_POINT ( 'NONE',  ( -40.00000000000000000, -69.50000000000000000, 0.000000000000000000 ) ) ;
#15800 = CARTESIAN_POINT ( 'NONE',  ( 16.48292494720000079, -100.3063911739999980, 4.382887648540000569 ) ) ;
#15801 = EDGE_LOOP ( 'NONE', ( #8263, #23458, #6370, #9870 ) ) ;
#15802 = CARTESIAN_POINT ( 'NONE',  ( -7.279135155890000597, -73.90050421709999284, -39.59102417159999021 ) ) ;
#15803 = CARTESIAN_POINT ( 'NONE',  ( -22.29259858720000054, -96.16784750930000314, -5.870011727330000539 ) ) ;
#15804 = EDGE_LOOP ( 'NONE', ( #9942, #21272, #1316, #27901 ) ) ;
#15805 = CARTESIAN_POINT ( 'NONE',  ( 0.000000000000000000, -72.82938648530000592, 0.000000000000000000 ) ) ;
#15806 = ORIENTED_EDGE ( 'NONE', *, *, #26685, .F. ) ;
#15807 = DIRECTION ( 'NONE',  ( 0.000000000000000000, 1.000000000000000000, 0.000000000000000000 ) ) ;
#15808 = CARTESIAN_POINT ( 'NONE',  ( 21.75855414729999993, -19.41837863929999841, 9.513576305009999956 ) ) ;
#15809 = ADVANCED_FACE ( 'NONE', ( #12708 ), #26397, .T. ) ;
#15810 = DIRECTION ( 'NONE',  ( 0.000000000000000000, -1.000000000000000000, 0.000000000000000000 ) ) ;
#15811 = CARTESIAN_POINT ( 'NONE',  ( 22.95300118209999951, -94.52293239719999463, -6.773262432920000187 ) ) ;
#15812 = EDGE_CURVE ( 'NONE', #28497, #9424, #26887, .T. ) ;
#15813 = CARTESIAN_POINT ( 'NONE',  ( 20.57008778049999975, -58.79569913830000161, 11.24574759670000113 ) ) ;
#15814 = CARTESIAN_POINT ( 'NONE',  ( 10.72517777600000066, -69.13421244780001018, -25.99822748240000081 ) ) ;
#15815 = CARTESIAN_POINT ( 'NONE',  ( -16.61661837067523351, -98.46254901739948195, 8.790168390964289813 ) ) ;
#15816 = ORIENTED_EDGE ( 'NONE', *, *, #15360, .T. ) ;
#15817 = CARTESIAN_POINT ( 'NONE',  ( -10.20110288159999890, -84.00000000000000000, 41.00000000000000000 ) ) ;
#15818 = CARTESIAN_POINT ( 'NONE',  ( -3.153926688883155194, -98.09459569084205555, 20.20253999486456564 ) ) ;
#15819 = CARTESIAN_POINT ( 'NONE',  ( -12.73014500989999931, -100.0496341300000154, -11.13483849640000045 ) ) ;
#15820 = CARTESIAN_POINT ( 'NONE',  ( 20.74876991574076968, -19.47341637985504192, 9.495871454077789764 ) ) ;
#15821 = CIRCLE ( 'NONE', #2828, 5.499999999999998224 ) ;
#15822 = CARTESIAN_POINT ( 'NONE',  ( -40.70731707320000226, -74.50000000000000000, -7.215414233289999757 ) ) ;
#15823 = ORIENTED_EDGE ( 'NONE', *, *, #13339, .F. ) ;
#15824 = VECTOR ( 'NONE', #5570, 1000.000000000000114 ) ;
#15825 = EDGE_CURVE ( 'NONE', #178, #7860, #3601, .T. ) ;
#15826 = CARTESIAN_POINT ( 'NONE',  ( 26.26892325874138123, -92.86276748829368444, -15.49872433666240745 ) ) ;
#15827 = ORIENTED_EDGE ( 'NONE', *, *, #24145, .T. ) ;
#15828 = CYLINDRICAL_SURFACE ( 'NONE', #16963, 61.34999999999998721 ) ;
#15829 = DIRECTION ( 'NONE',  ( 1.000000000000000000, 0.000000000000000000, 0.000000000000000000 ) ) ;
#15830 = CARTESIAN_POINT ( 'NONE',  ( 0.000000000000000000, -77.00000000000000000, -40.00000000000000000 ) ) ;
#15831 = CARTESIAN_POINT ( 'NONE',  ( 11.26686242699999951, -92.77082804750000378, 27.55452589829999965 ) ) ;
#15832 = EDGE_LOOP ( 'NONE', ( #11145, #587, #2700, #2973, #24136, #6744, #24699 ) ) ;
#15833 = CYLINDRICAL_SURFACE ( 'NONE', #14933, 7.250000000000004441 ) ;
#15834 = ORIENTED_EDGE ( 'NONE', *, *, #21022, .F. ) ;
#15835 = CARTESIAN_POINT ( 'NONE',  ( -23.03458422004786854, -71.75398255365567479, 16.25737041499285951 ) ) ;
#15836 = CARTESIAN_POINT ( 'NONE',  ( 23.88581173909999933, -92.98481359359999487, 11.87508144250000086 ) ) ;
#15837 = CARTESIAN_POINT ( 'NONE',  ( 47.03569028360000459, -74.19054636589999063, -1.774065497670000102 ) ) ;
#15838 = EDGE_LOOP ( 'NONE', ( #13656, #25332, #15624, #8375 ) ) ;
#15839 = TOROIDAL_SURFACE ( 'NONE', #6529, 53.85000000000000142, 0.5000000000000000000 ) ;
#15840 = DIRECTION ( 'NONE',  ( 0.000000000000000000, 1.000000000000000000, 0.000000000000000000 ) ) ;
#15841 = CARTESIAN_POINT ( 'NONE',  ( -22.46797589350000024, -80.18584073460000639, -32.25831116089999995 ) ) ;
#15842 = AXIS2_PLACEMENT_3D ( 'NONE', #25116, #9063, #16360 ) ;
#15843 = AXIS2_PLACEMENT_3D ( 'NONE', #23573, #3614, #3481 ) ;
#15844 = CARTESIAN_POINT ( 'NONE',  ( 8.514971421829999443, -37.95267571699999820, -21.81705067669999920 ) ) ;
#15845 = DIRECTION ( 'NONE',  ( 0.000000000000000000, 1.000000000000000000, 0.000000000000000000 ) ) ;
#15846 = DIRECTION ( 'NONE',  ( 0.000000000000000000, 1.000000000000000000, 0.000000000000000000 ) ) ;
#15847 = ORIENTED_EDGE ( 'NONE', *, *, #12318, .T. ) ;
#15848 = CARTESIAN_POINT ( 'NONE',  ( 0.000000000000000000, -2.000000000000000000, 0.000000000000000000 ) ) ;
#15849 = EDGE_CURVE ( 'NONE', #22782, #25354, #1955, .T. ) ;
#15850 = CARTESIAN_POINT ( 'NONE',  ( -16.89186647220000026, -100.0262800969999972, 3.317271451419999906 ) ) ;
#15851 = DIRECTION ( 'NONE',  ( 0.000000000000000000, 1.000000000000000000, 0.000000000000000000 ) ) ;
#15852 = CARTESIAN_POINT ( 'NONE',  ( -21.60034937969999902, -74.39508596250000494, -32.77174707999999725 ) ) ;
#15853 = FACE_OUTER_BOUND ( 'NONE', #26086, .T. ) ;
#15854 = DIRECTION ( 'NONE',  ( 0.000000000000000000, 1.000000000000000000, 0.000000000000000000 ) ) ;
#15855 = CARTESIAN_POINT ( 'NONE',  ( -7.521798597035361134, -73.99983172279489452, 38.87042118007536118 ) ) ;
#15856 = CARTESIAN_POINT ( 'NONE',  ( -18.44071070329999884, -19.46458168459999882, 12.28140447959999904 ) ) ;
#15857 = ORIENTED_EDGE ( 'NONE', *, *, #27023, .F. ) ;
#15858 = CARTESIAN_POINT ( 'NONE',  ( -9.636993756300000769, -93.95774545369999942, -23.10706980140000155 ) ) ;
#15859 = DIRECTION ( 'NONE',  ( 0.000000000000000000, -1.000000000000000000, 0.000000000000000000 ) ) ;
#15860 = CARTESIAN_POINT ( 'NONE',  ( 8.408939714870001580, -35.33620304669999257, -20.95510900379999697 ) ) ;
#15861 = CARTESIAN_POINT ( 'NONE',  ( 15.98533867912071216, -100.9616911410360984, 4.227991388196914890 ) ) ;
#15862 = DIRECTION ( 'NONE',  ( 0.000000000000000000, 1.000000000000000000, 0.000000000000000000 ) ) ;
#15863 = CARTESIAN_POINT ( 'NONE',  ( 22.45957212889999965, -52.58489974409999945, 10.08523539449999973 ) ) ;
#15864 = CIRCLE ( 'NONE', #2850, 3.000000000000000888 ) ;
#15865 = CARTESIAN_POINT ( 'NONE',  ( -14.60853884240962408, -101.2450099480301020, 4.215530974001670650 ) ) ;
#15866 = CIRCLE ( 'NONE', #13533, 0.3500000000000003664 ) ;
#15867 = AXIS2_PLACEMENT_3D ( 'NONE', #17944, #6728, #7021 ) ;
#15868 = SHAPE_DEFINITION_REPRESENTATION ( #24339, #24690 ) ;
#15869 = CARTESIAN_POINT ( 'NONE',  ( 24.42476877459999685, -57.44036991850000362, 1.191907264949999989 ) ) ;
#15870 = CIRCLE ( 'NONE', #7053, 3.750000000000000000 ) ;
#15871 = DIRECTION ( 'NONE',  ( 0.000000000000000000, -1.000000000000000000, 0.000000000000000000 ) ) ;
#15872 = VERTEX_POINT ( 'NONE', #14633 ) ;
#15873 = EDGE_CURVE ( 'NONE', #12424, #4784, #16629, .T. ) ;
#15874 = DIRECTION ( 'NONE',  ( 0.000000000000000000, -1.000000000000000000, 0.000000000000000000 ) ) ;
#15875 = ORIENTED_EDGE ( 'NONE', *, *, #12125, .T. ) ;
#15876 = CARTESIAN_POINT ( 'NONE',  ( 28.91458899939999938, -72.00000000000000000, 3.086557976320000396 ) ) ;
#15877 = CARTESIAN_POINT ( 'NONE',  ( 9.165534020747788446, -98.33329995119029832, 16.60371393490449421 ) ) ;
#15878 = ORIENTED_EDGE ( 'NONE', *, *, #21606, .F. ) ;
#15879 = CARTESIAN_POINT ( 'NONE',  ( 27.75394116159999669, -74.50000000000000000, -27.75394116159999669 ) ) ;
#15880 = CARTESIAN_POINT ( 'NONE',  ( 4.340170735955752868, -93.18010901074717367, -28.18556222814888912 ) ) ;
#15881 = CARTESIAN_POINT ( 'NONE',  ( 1.563021348000000144, -94.54719592040000009, 23.80457129850000086 ) ) ;
#15882 = CARTESIAN_POINT ( 'NONE',  ( -19.56140538540000051, -96.65247697220000589, 8.334726878210000578 ) ) ;
#15883 = CARTESIAN_POINT ( 'NONE',  ( 15.50925563669999896, -100.9197081840000010, 1.894558565230000102 ) ) ;
#15884 = AXIS2_PLACEMENT_3D ( 'NONE', #17510, #26395, #8188 ) ;
#15885 = CARTESIAN_POINT ( 'NONE',  ( 21.74745445608735039, -37.94920488029457317, -8.395240280012213674 ) ) ;
#15886 = ORIENTED_EDGE ( 'NONE', *, *, #21882, .T. ) ;
#15887 = CIRCLE ( 'NONE', #3349, 20.64285714290000229 ) ;
#15888 = DIRECTION ( 'NONE',  ( 1.000000000000000000, 0.000000000000000000, 0.000000000000000000 ) ) ;
#15889 = EDGE_CURVE ( 'NONE', #11169, #25860, #15192, .T. ) ;
#15890 = CARTESIAN_POINT ( 'NONE',  ( -38.22863009216007413, -65.70299785168744222, -1.381847430537364030 ) ) ;
#15891 = CARTESIAN_POINT ( 'NONE',  ( -13.26438106576386744, -92.82709422631874929, 27.46463547702218122 ) ) ;
#15892 = ORIENTED_EDGE ( 'NONE', *, *, #3932, .F. ) ;
#15893 = DIRECTION ( 'NONE',  ( 0.000000000000000000, -1.000000000000000000, 0.000000000000000000 ) ) ;
#15894 = DIRECTION ( 'NONE',  ( 0.000000000000000000, 1.000000000000000000, 0.000000000000000000 ) ) ;
#15895 = DIRECTION ( 'NONE',  ( 0.4238361315509043825, 0.000000000000000000, -0.9057388881967940453 ) ) ;
#15896 = ORIENTED_EDGE ( 'NONE', *, *, #1331, .T. ) ;
#15897 = CARTESIAN_POINT ( 'NONE',  ( -18.05296423140000073, -94.57749571930000343, 16.11415966959999935 ) ) ;
#15898 = EDGE_CURVE ( 'NONE', #4998, #22563, #859, .T. ) ;
#15899 = CARTESIAN_POINT ( 'NONE',  ( -18.48358769389999878, -19.46501104080000033, 12.15083731070000184 ) ) ;
#15900 = CARTESIAN_POINT ( 'NONE',  ( 26.06532122270797203, -74.32759098968446665, -29.30452812900732340 ) ) ;
#15901 = CARTESIAN_POINT ( 'NONE',  ( 20.33566493080000015, -36.00000000000000000, -9.885503730140001721 ) ) ;
#15902 = CARTESIAN_POINT ( 'NONE',  ( -14.80839208230898407, -74.26929999394664605, 36.28872789036408619 ) ) ;
#15903 = CARTESIAN_POINT ( 'NONE',  ( 7.130058149629999953, -99.83167681540000160, 15.79461927190000203 ) ) ;
#15904 = AXIS2_PLACEMENT_3D ( 'NONE', #1335, #14299, #7885 ) ;
#15905 = EDGE_LOOP ( 'NONE', ( #4305, #22127, #1163, #26199, #27685 ) ) ;
#15906 = ADVANCED_FACE ( 'NONE', ( #28727 ), #27355, .T. ) ;
#15907 = CARTESIAN_POINT ( 'NONE',  ( 28.21054109043858915, -92.66455718075739867, 11.59376651551000315 ) ) ;
#15908 = CARTESIAN_POINT ( 'NONE',  ( 23.98460332450000010, -18.50000000000000000, 2.503291441710000065 ) ) ;
#15909 = EDGE_CURVE ( 'NONE', #23006, #23088, #8915, .T. ) ;
#15910 = CARTESIAN_POINT ( 'NONE',  ( 14.78896428320000034, -96.97547306780001009, 14.66850198189999865 ) ) ;
#15911 = ORIENTED_EDGE ( 'NONE', *, *, #15368, .T. ) ;
#15912 = CARTESIAN_POINT ( 'NONE',  ( 7.268571389559999929, -74.08839659379999887, 39.96417052329999819 ) ) ;
#15913 = CARTESIAN_POINT ( 'NONE',  ( 6.258798239620000814, -92.50000000000000000, -29.85092033080000107 ) ) ;
#15914 = B_SPLINE_SURFACE_WITH_KNOTS ( 'NONE', 5, 5, ( 
 ( #6570, #184, #26249, #15590, #28562, #8597 ),
 ( #21867, #15433, #15137, #28415, #24489, #24047 ),
 ( #4386, #4085, #17792, #17499, #24345, #26385 ),
 ( #13255, #26682, #4523, #6413, #12811, #22306 ),
 ( #9034, #21721, #12954, #1918, #2504, #332 ),
 ( #25236, #2944, #16325, #5119, #778, #24792 ),
 ( #4830, #3094, #482, #26834, #18383, #16174 ),
 ( #6866, #27270, #24937, #7166, #16032, #24643 ),
 ( #11359, #18523, #11504, #2652, #15730, #22905 ) ),
 .UNSPECIFIED., .F., .F., .F.,
 ( 6, 3, 6 ),
 ( 6, 6 ),
 ( 5.892872301239999241E-16, 2.251105814059999766, 5.576980695549999645 ),
 ( 0.000000000000000000, 1.000000000000000000 ),
 .UNSPECIFIED. ) ;
#15915 = CARTESIAN_POINT ( 'NONE',  ( 21.44286899589999962, -36.30033507760000333, -7.882324037790000126 ) ) ;
#15916 = CARTESIAN_POINT ( 'NONE',  ( 26.83947876876618821, -72.50065199416241057, -10.87728020417079833 ) ) ;
#15917 = CARTESIAN_POINT ( 'NONE',  ( 7.799278058849999695, -37.54433185199999912, -21.53604737210000053 ) ) ;
#15918 = ADVANCED_FACE ( 'NONE', ( #2538 ), #17678, .T. ) ;
#15919 = DIRECTION ( 'NONE',  ( -0.4751828347227322613, 0.1327433628319252545, -0.8698163445285104212 ) ) ;
#15920 = CARTESIAN_POINT ( 'NONE',  ( 7.132709192110000096, -99.83167692499999646, 15.78738634319999967 ) ) ;
#15921 = AXIS2_PLACEMENT_3D ( 'NONE', #3159, #21209, #1916 ) ;
#15922 = CARTESIAN_POINT ( 'NONE',  ( 23.97709848270000066, -18.50000000000000000, 2.237158816650000048 ) ) ;
#15923 = CARTESIAN_POINT ( 'NONE',  ( 0.4235579524470000634, -99.83167544280000527, -17.31869659160000197 ) ) ;
#15924 = DIRECTION ( 'NONE',  ( 1.000000000000000000, 0.000000000000000000, 0.000000000000000000 ) ) ;
#15925 = ORIENTED_EDGE ( 'NONE', *, *, #26947, .F. ) ;
#15926 = CYLINDRICAL_SURFACE ( 'NONE', #3711, 0.4999999999999982236 ) ;
#15927 = AXIS2_PLACEMENT_3D ( 'NONE', #8905, #9352, #11527 ) ;
#15928 = CARTESIAN_POINT ( 'NONE',  ( 27.49607050420000220, -67.46050995630001523, 1.934818144049999855 ) ) ;
#15929 = CARTESIAN_POINT ( 'NONE',  ( -24.15516222759999820, -94.98812477599999227, -4.102682929219999330 ) ) ;
#15930 = DIRECTION ( 'NONE',  ( 1.000000000000000000, 0.000000000000000000, 0.000000000000000000 ) ) ;
#15931 = CARTESIAN_POINT ( 'NONE',  ( 26.46310988749999993, -64.24504445130001784, 1.532420830840000026 ) ) ;
#15932 = CARTESIAN_POINT ( 'NONE',  ( 40.00000000000000000, -84.50000000000000000, 4.463096558990000197E-15 ) ) ;
#15933 = FACE_OUTER_BOUND ( 'NONE', #11893, .T. ) ;
#15934 = ORIENTED_EDGE ( 'NONE', *, *, #10541, .F. ) ;
#15935 = CARTESIAN_POINT ( 'NONE',  ( 36.29172688410000092, -74.90632999339999287, -14.94947910089999965 ) ) ;
#15936 = CARTESIAN_POINT ( 'NONE',  ( -22.41809188630069727, -79.89426907611134254, -32.75488367496921427 ) ) ;
#15937 = CARTESIAN_POINT ( 'NONE',  ( -14.25684790429999893, -62.95263723189999183, 21.84526217519999847 ) ) ;
#15938 = CARTESIAN_POINT ( 'NONE',  ( 0.000000000000000000, -32.30000000000000426, 0.000000000000000000 ) ) ;
#15939 = CARTESIAN_POINT ( 'NONE',  ( -12.03461033140000147, -62.10472517099999834, 20.80665457679999975 ) ) ;
#15940 = DIRECTION ( 'NONE',  ( 1.000000000000000000, 0.000000000000000000, 0.000000000000000000 ) ) ;
#15941 = CIRCLE ( 'NONE', #10799, 29.91857981989999971 ) ;
#15942 = CARTESIAN_POINT ( 'NONE',  ( 26.85539570426266920, -72.18744871742090652, 10.61487170321338347 ) ) ;
#15943 = PRODUCT_RELATED_PRODUCT_CATEGORY ( 'part', '', ( #14772 ) ) ;
#15944 = CIRCLE ( 'NONE', #3408, 10.00000000000000000 ) ;
#15945 = CARTESIAN_POINT ( 'NONE',  ( 20.27618985420000186, -36.00000000000000000, -9.807089787700000727 ) ) ;
#15946 = B_SPLINE_CURVE_WITH_KNOTS ( 'NONE', 5,
 ( #9980, #18894, #25592, #23122, #20797, #2879 ),
 .UNSPECIFIED., .F., .F.,
 ( 6, 6 ),
 ( 0.000000000000000000, 1.000000000000000000 ),
 .UNSPECIFIED. ) ;
#15947 = EDGE_CURVE ( 'NONE', #11019, #5336, #369, .T. ) ;
#15948 = CARTESIAN_POINT ( 'NONE',  ( -13.34153245340000105, -91.50000000000000000, 27.42724032409999779 ) ) ;
#15949 = EDGE_LOOP ( 'NONE', ( #11567, #28332, #17639 ) ) ;
#15950 = CARTESIAN_POINT ( 'NONE',  ( -7.215414233289999757, -74.50000000000000000, -40.70731707320000226 ) ) ;
#15951 =( NAMED_UNIT ( * ) SI_UNIT ( $, .STERADIAN. ) SOLID_ANGLE_UNIT ( ) );
#15952 = CARTESIAN_POINT ( 'NONE',  ( -17.58990901810000196, -98.24904979049999554, -7.931573376680000287 ) ) ;
#15953 = ORIENTED_EDGE ( 'NONE', *, *, #14628, .T. ) ;
#15954 = EDGE_CURVE ( 'NONE', #4525, #6019, #24955, .T. ) ;
#15955 = CARTESIAN_POINT ( 'NONE',  ( 9.264753623212678590, -92.86276748881633125, 29.05909712188475780 ) ) ;
#15956 = EDGE_CURVE ( 'NONE', #18344, #14992, #7800, .T. ) ;
#15957 = DIRECTION ( 'NONE',  ( 0.000000000000000000, 1.000000000000000000, 0.000000000000000000 ) ) ;
#15958 = CARTESIAN_POINT ( 'NONE',  ( -7.639087602144537748, -98.53908159008453538, 17.12000419490125580 ) ) ;
#15959 = CIRCLE ( 'NONE', #2013, 30.50000000000000000 ) ;
#15960 = CARTESIAN_POINT ( 'NONE',  ( -16.67828388959999941, -74.50000000000000000, 44.75374114529999758 ) ) ;
#15961 = DIRECTION ( 'NONE',  ( 1.000000000000000000, 0.000000000000000000, 0.000000000000000000 ) ) ;
#15962 = CARTESIAN_POINT ( 'NONE',  ( 18.48933855830000184, -18.50000000000000000, 10.02928721039999971 ) ) ;
#15963 = CARTESIAN_POINT ( 'NONE',  ( -8.929965488379998817, -95.98352844290000974, -20.19091974539999867 ) ) ;
#15964 = CARTESIAN_POINT ( 'NONE',  ( -17.02803783414526961, -97.66783633811731136, 10.15242468662800412 ) ) ;
#15965 = ORIENTED_EDGE ( 'NONE', *, *, #17367, .T. ) ;
#15966 = CIRCLE ( 'NONE', #10746, 2.000000000000000888 ) ;
#15967 = DIRECTION ( 'NONE',  ( 0.000000000000000000, 0.000000000000000000, -1.000000000000000000 ) ) ;
#15968 = CARTESIAN_POINT ( 'NONE',  ( -13.15237738589999950, -99.55609327400000552, -11.37038234410000115 ) ) ;
#15969 = AXIS2_PLACEMENT_3D ( 'NONE', #24791, #13254, #15729 ) ;
#15970 = CARTESIAN_POINT ( 'NONE',  ( 20.88115893480090790, -19.47504441211762227, 9.474803371222611403 ) ) ;
#15971 = CARTESIAN_POINT ( 'NONE',  ( 22.75601413952083263, -61.35865215156498920, -7.240038726238430478 ) ) ;
#15972 = ORIENTED_EDGE ( 'NONE', *, *, #23619, .F. ) ;
#15973 = DIRECTION ( 'NONE',  ( 0.000000000000000000, 1.000000000000000000, 0.000000000000000000 ) ) ;
#15974 = VERTEX_POINT ( 'NONE', #4269 ) ;
#15975 = LINE ( 'NONE', #22559, #13715 ) ;
#15976 = CIRCLE ( 'NONE', #17840, 2.000000000000001776 ) ;
#15977 = FACE_OUTER_BOUND ( 'NONE', #18481, .T. ) ;
#15978 = CARTESIAN_POINT ( 'NONE',  ( 2.731422428999999763, -93.80378326950000201, 24.76396224019999792 ) ) ;
#15979 = ORIENTED_EDGE ( 'NONE', *, *, #5439, .T. ) ;
#15980 = EDGE_CURVE ( 'NONE', #300, #26675, #23174, .T. ) ;
#15981 = DIRECTION ( 'NONE',  ( 0.000000000000000000, 1.000000000000000000, 0.000000000000000000 ) ) ;
#15982 = ORIENTED_EDGE ( 'NONE', *, *, #21876, .T. ) ;
#15983 = CARTESIAN_POINT ( 'NONE',  ( -22.55319281656417729, -69.29687318610271518, 14.97856516669103399 ) ) ;
#15984 = CARTESIAN_POINT ( 'NONE',  ( 21.06416788030000120, -36.18018306559999786, -9.332951880679999590 ) ) ;
#15985 = CARTESIAN_POINT ( 'NONE',  ( 47.13359351679999776, -74.47757638999999585, -1.343551159269999795 ) ) ;
#15986 = ORIENTED_EDGE ( 'NONE', *, *, #1470, .F. ) ;
#15987 = CONICAL_SURFACE ( 'NONE', #20194, 57.74999999999999289, 1.224257462359999549 ) ;
#15988 = DIRECTION ( 'NONE',  ( 0.000000000000000000, -1.000000000000000000, 0.000000000000000000 ) ) ;
#15989 = CARTESIAN_POINT ( 'NONE',  ( -11.66011925523032922, -62.65979579072126882, 21.24220495570105882 ) ) ;
#15990 = ADVANCED_FACE ( 'NONE', ( #13436 ), #18966, .T. ) ;
#15991 = SPHERICAL_SURFACE ( 'NONE', #1964, 1.000000000000000000 ) ;
#15992 = DIRECTION ( 'NONE',  ( 0.000000000000000000, -1.000000000000000000, 0.000000000000000000 ) ) ;
#15993 = CARTESIAN_POINT ( 'NONE',  ( 0.000000000000000000, -26.59999999999999787, 0.000000000000000000 ) ) ;
#15994 = DIRECTION ( 'NONE',  ( 0.000000000000000000, 1.000000000000000000, 0.000000000000000000 ) ) ;
#15995 = ORIENTED_EDGE ( 'NONE', *, *, #15393, .F. ) ;
#15996 = CARTESIAN_POINT ( 'NONE',  ( 36.39554599249999711, -74.16575166410000008, -14.53417042330000086 ) ) ;
#15997 = CIRCLE ( 'NONE', #14609, 0.4999999999999987232 ) ;
#15998 = CARTESIAN_POINT ( 'NONE',  ( 13.78129364559999814, -99.94751438429999268, -10.21817317360000210 ) ) ;
#15999 = CARTESIAN_POINT ( 'NONE',  ( -39.89387480210000092, -74.19145785139998850, 7.305170733980000719 ) ) ;
#16000 = B_SPLINE_CURVE_WITH_KNOTS ( 'NONE', 5,
 ( #17482, #17922, #23894, #6394, #26661, #3930, #163, #4212, #10739 ),
 .UNSPECIFIED., .F., .F.,
 ( 6, 3, 6 ),
 ( 0.000000000000000000, 1.237573681330000008, 1.566718891460000096 ),
 .UNSPECIFIED. ) ;
#16001 = CARTESIAN_POINT ( 'NONE',  ( -21.99985828019999801, -74.00000000000000000, -31.89935321680000158 ) ) ;
#16002 = EDGE_LOOP ( 'NONE', ( #59, #10135, #14823, #5748 ) ) ;
#16003 = DIRECTION ( 'NONE',  ( 0.000000000000000000, 1.000000000000000000, 0.000000000000000000 ) ) ;
#16004 = CARTESIAN_POINT ( 'NONE',  ( -0.1689899845689999958, -101.2530993010000060, -15.19297360289999865 ) ) ;
#16005 = CARTESIAN_POINT ( 'NONE',  ( -17.41808129929999893, -18.50000000000000000, 12.13953735139999957 ) ) ;
#16006 = ORIENTED_EDGE ( 'NONE', *, *, #4464, .T. ) ;
#16007 = CARTESIAN_POINT ( 'NONE',  ( -13.09440877569999984, -92.84550106799999014, -23.96917193350000019 ) ) ;
#16008 = CARTESIAN_POINT ( 'NONE',  ( 23.22783021959999772, -61.45046333410000017, 10.43375156039999929 ) ) ;
#16009 = CARTESIAN_POINT ( 'NONE',  ( 7.670972941899999675, -34.59820487809999889, -21.21808928440000130 ) ) ;
#16010 = CARTESIAN_POINT ( 'NONE',  ( 16.37130097589949784, -100.4507315479511078, 4.354834957207184054 ) ) ;
#16011 = FACE_OUTER_BOUND ( 'NONE', #9629, .T. ) ;
#16012 = ORIENTED_EDGE ( 'NONE', *, *, #4842, .F. ) ;
#16013 = DIRECTION ( 'NONE',  ( 1.000000000000000000, 0.000000000000000000, 0.000000000000000000 ) ) ;
#16014 = AXIS2_PLACEMENT_3D ( 'NONE', #6659, #20058, #24574 ) ;
#16015 = ITEM_DEFINED_TRANSFORMATION ( 'NONE', 'NONE', #5515,  #26433 ) ;
#16016 = CARTESIAN_POINT ( 'NONE',  ( -11.84271430029999905, -64.58097566740001128, -22.96390433080000193 ) ) ;
#16017 = CARTESIAN_POINT ( 'NONE',  ( 36.91823499837838085, -79.75463803037827404, -14.40641522487323023 ) ) ;
#16018 = DIRECTION ( 'NONE',  ( 1.000000000000000000, 0.000000000000000000, 0.000000000000000000 ) ) ;
#16019 = CARTESIAN_POINT ( 'NONE',  ( 10.60935311512664647, -93.02766005061967292, 27.57871627749636545 ) ) ;
#16020 = ORIENTED_EDGE ( 'NONE', *, *, #8123, .F. ) ;
#16021 = EDGE_CURVE ( 'NONE', #7301, #7043, #14174, .T. ) ;
#16022 = FACE_OUTER_BOUND ( 'NONE', #14224, .T. ) ;
#16023 = ORIENTED_EDGE ( 'NONE', *, *, #18844, .F. ) ;
#16024 = CIRCLE ( 'NONE', #24407, 0.3500000000000003664 ) ;
#16025 = CARTESIAN_POINT ( 'NONE',  ( -4.794255386040000566, -90.50000000000000000, -8.775825618900000791 ) ) ;
#16026 = VERTEX_POINT ( 'NONE', #16509 ) ;
#16027 = CARTESIAN_POINT ( 'NONE',  ( -18.09292965979135914, -92.55388824293693517, -23.53605431443747520 ) ) ;
#16028 = ADVANCED_FACE ( 'NONE', ( #11687 ), #2215, .F. ) ;
#16029 = CARTESIAN_POINT ( 'NONE',  ( -29.91144828099999842, -92.50000000000000000, -0.6532076026720000650 ) ) ;
#16030 = DIRECTION ( 'NONE',  ( 0.000000000000000000, -1.000000000000000000, 0.000000000000000000 ) ) ;
#16031 = CARTESIAN_POINT ( 'NONE',  ( -19.97010144720000113, -95.85316701180001075, 10.36429926879999996 ) ) ;
#16032 = CARTESIAN_POINT ( 'NONE',  ( -10.66364198750000014, -19.17999199609999650, -21.54557793210000227 ) ) ;
#16033 = CARTESIAN_POINT ( 'NONE',  ( 21.52462730065835572, -37.46071944955636468, -7.740090088892075393 ) ) ;
#16034 = VERTEX_POINT ( 'NONE', #11978 ) ;
#16035 = CARTESIAN_POINT ( 'NONE',  ( 12.33671740429999986, -93.75379239689999622, -21.67807059210000276 ) ) ;
#16036 = CARTESIAN_POINT ( 'NONE',  ( -37.97905434469389263, -65.72207046438377631, -0.9031576581934117609 ) ) ;
#16037 = CARTESIAN_POINT ( 'NONE',  ( 40.21639064484389081, -74.12723354410567822, 7.246819345891047703 ) ) ;
#16038 = VERTEX_POINT ( 'NONE', #956 ) ;
#16039 = AXIS2_PLACEMENT_3D ( 'NONE', #15530, #24437, #24738 ) ;
#16040 = CARTESIAN_POINT ( 'NONE',  ( 38.08875739639999836, -82.25000000000000000, -9.476764215410000247 ) ) ;
#16041 = FACE_OUTER_BOUND ( 'NONE', #26630, .T. ) ;
#16042 = FACE_OUTER_BOUND ( 'NONE', #8891, .T. ) ;
#16043 = ORIENTED_EDGE ( 'NONE', *, *, #8427, .F. ) ;
#16044 = CARTESIAN_POINT ( 'NONE',  ( -17.52609522539999887, -98.43713976429998525, 8.802680806179999706 ) ) ;
#16045 = EDGE_CURVE ( 'NONE', #26105, #5689, #1322, .T. ) ;
#16046 = AXIS2_PLACEMENT_3D ( 'NONE', #11405, #13898, #25285 ) ;
#16047 = CARTESIAN_POINT ( 'NONE',  ( 0.5239533329500000169, -99.69348480060000384, -17.31365208049999893 ) ) ;
#16048 = CARTESIAN_POINT ( 'NONE',  ( 25.26718046270000073, -19.50000000000000000, 6.129403842640000377 ) ) ;
#16049 = LINE ( 'NONE', #24951, #577 ) ;
#16050 = CARTESIAN_POINT ( 'NONE',  ( -14.61005163810492391, -74.14612126337357267, 36.27173304699432066 ) ) ;
#16051 = CARTESIAN_POINT ( 'NONE',  ( -19.35716652280000005, -18.50000000000000000, 15.34467299940000018 ) ) ;
#16053 = VERTEX_POINT ( 'NONE', #23080 ) ;
#16052 = ADVANCED_FACE ( 'NONE', ( #809 ), #7641, .T. ) ;
#16054 = ADVANCED_FACE ( 'NONE', ( #1093 ), #4999, .T. ) ;
#16055 = PLANE ( 'NONE',  #8593 ) ;
#16056 = TOROIDAL_SURFACE ( 'NONE', #13233, 60.85000000000000142, 0.5000000000000000000 ) ;
#16057 = CARTESIAN_POINT ( 'NONE',  ( -10.20110288159999890, -80.50000000000000000, 41.00000000000000000 ) ) ;
#16058 = ORIENTED_EDGE ( 'NONE', *, *, #5318, .T. ) ;
#16059 = CARTESIAN_POINT ( 'NONE',  ( 23.53235809685696367, -92.58608763741389680, -19.40304636274978378 ) ) ;
#16060 = CARTESIAN_POINT ( 'NONE',  ( 7.732662040940000203, -18.50000000000000000, -19.49253883449999947 ) ) ;
#16061 = CARTESIAN_POINT ( 'NONE',  ( 19.55068592539999983, -35.72724453810000256, -9.038647860560001135 ) ) ;
#16062 = DIRECTION ( 'NONE',  ( 0.000000000000000000, 1.000000000000000000, 0.000000000000000000 ) ) ;
#16063 = CARTESIAN_POINT ( 'NONE',  ( -5.679770007689999289, -74.50000000000000000, 46.75000000000000000 ) ) ;
#16064 = CARTESIAN_POINT ( 'NONE',  ( 8.724064349480000757, -36.49187789639999835, -21.25496272479999860 ) ) ;
#16065 = LINE ( 'NONE', #11247, #26464 ) ;
#16066 = ORIENTED_EDGE ( 'NONE', *, *, #191, .T. ) ;
#16067 = CARTESIAN_POINT ( 'NONE',  ( 8.316147692919997780, -98.89962500040000748, 16.28909968399999997 ) ) ;
#16068 = DIRECTION ( 'NONE',  ( 0.2414462220490750377, 0.000000000000000000, -0.9704142011833034598 ) ) ;
#16069 = CARTESIAN_POINT ( 'NONE',  ( -2.157875506039999891, -97.64874574800001028, -19.85504165189999881 ) ) ;
#16070 = CARTESIAN_POINT ( 'NONE',  ( 26.75649127029999619, -93.00000000000000000, -13.26822602009999841 ) ) ;
#16071 = MANIFOLD_SOLID_BREP ( 'Screw Set - M6-18mm TorxKey', #5386 ) ;
#16072 = CARTESIAN_POINT ( 'NONE',  ( -15.03193870770000018, -100.8816836399999914, 4.847770938290000053 ) ) ;
#16073 = DIRECTION ( 'NONE',  ( 0.000000000000000000, -1.000000000000000000, 0.000000000000000000 ) ) ;
#16074 = CARTESIAN_POINT ( 'NONE',  ( -18.94876721349164583, -98.12113811964421473, -7.590811461915794034 ) ) ;
#16075 = CARTESIAN_POINT ( 'NONE',  ( -37.98130312831552402, -65.72281103701608629, 0.9050787996994155149 ) ) ;
#16076 = EDGE_CURVE ( 'NONE', #12485, #22153, #20848, .T. ) ;
#16077 = AXIS2_PLACEMENT_3D ( 'NONE', #17937, #7015, #15276 ) ;
#16078 = DIRECTION ( 'NONE',  ( 0.000000000000000000, -1.000000000000000000, 0.000000000000000000 ) ) ;
#16079 = CARTESIAN_POINT ( 'NONE',  ( 22.58640054960000043, -44.88560226349999738, -9.205819528950000219 ) ) ;
#16080 = CARTESIAN_POINT ( 'NONE',  ( 24.72534431299499147, -93.40025063776721481, -12.31560360671905840 ) ) ;
#16081 = CARTESIAN_POINT ( 'NONE',  ( -15.23837145989999797, -101.0223441809999940, 2.799506657709999846 ) ) ;
#16082 = ORIENTED_EDGE ( 'NONE', *, *, #4977, .T. ) ;
#16083 = CARTESIAN_POINT ( 'NONE',  ( 36.47289884999999998, -75.00000018510000643, -14.78463685610000056 ) ) ;
#16084 = CARTESIAN_POINT ( 'NONE',  ( 6.783366714739999637, -101.1848541609999899, 13.69406429940000081 ) ) ;
#16085 = CARTESIAN_POINT ( 'NONE',  ( 7.824897742070000106, -101.4837543189999991, 13.99581122470000061 ) ) ;
#16086 = AXIS2_PLACEMENT_3D ( 'NONE', #7069, #13305, #20462 ) ;
#16087 = CARTESIAN_POINT ( 'NONE',  ( -13.31744303520000017, -66.93384306320000121, 22.33243309759999917 ) ) ;
#16088 = CARTESIAN_POINT ( 'NONE',  ( 9.020398574519999713, -35.69157542760000013, -19.55164510480000217 ) ) ;
#16089 = CARTESIAN_POINT ( 'NONE',  ( 40.00000000000000000, -80.50000000000000000, -7.105427357599999217E-15 ) ) ;
#16090 = CARTESIAN_POINT ( 'NONE',  ( 21.79230218349999859, -37.95144078439999902, -8.472395100330000872 ) ) ;
#16091 = CARTESIAN_POINT ( 'NONE',  ( -19.20225722901159315, -97.14187005060139768, 7.190316099514493686 ) ) ;
#16092 = CARTESIAN_POINT ( 'NONE',  ( -20.54204892785229219, -95.55433702432603127, -9.451947527820101058 ) ) ;
#16093 = CARTESIAN_POINT ( 'NONE',  ( -37.89522944376288649, -63.33487562142549621, 0.8055360949360760303 ) ) ;
#16094 = CARTESIAN_POINT ( 'NONE',  ( 16.79424914329999652, -99.83167681540000160, 4.273280107039999720 ) ) ;
#16095 = VERTEX_POINT ( 'NONE', #22787 ) ;
#16096 = CARTESIAN_POINT ( 'NONE',  ( 27.75394116159999669, -74.50000000000000000, -27.75394116159999669 ) ) ;
#16097 = CARTESIAN_POINT ( 'NONE',  ( -23.69410997499999993, -94.52419709919999491, -3.934991024959999972 ) ) ;
#16098 = EDGE_LOOP ( 'NONE', ( #9681, #14673 ) ) ;
#16099 = DIRECTION ( 'NONE',  ( -2.370544285295434954E-14, -1.000000000000000000, 5.540271532162629942E-15 ) ) ;
#16100 = ORIENTED_EDGE ( 'NONE', *, *, #17324, .F. ) ;
#16101 = CARTESIAN_POINT ( 'NONE',  ( -3.116266000930000057, -91.00000000000000000, -5.704286652290000426 ) ) ;
#16102 = CARTESIAN_POINT ( 'NONE',  ( -38.14141585637982956, -63.35633004489675812, 1.124464782024710674 ) ) ;
#16103 = CARTESIAN_POINT ( 'NONE',  ( -26.69293917519999937, -30.50310889129999836, -48.86109741659999628 ) ) ;
#16104 = AXIS2_PLACEMENT_3D ( 'NONE', #26400, #24807, #15450 ) ;
#16105 = CARTESIAN_POINT ( 'NONE',  ( 23.24434528660000154, -94.16309976680000204, -7.473846836599999932 ) ) ;
#16106 = CARTESIAN_POINT ( 'NONE',  ( -14.47017326849999996, -74.22762369209999633, 36.54526597599999604 ) ) ;
#16107 = FACE_OUTER_BOUND ( 'NONE', #12071, .T. ) ;
#16108 = CARTESIAN_POINT ( 'NONE',  ( -17.02652586798041412, -97.67115222923675333, 10.14659588024298209 ) ) ;
#16109 = ORIENTED_EDGE ( 'NONE', *, *, #3589, .F. ) ;
#16110 = CARTESIAN_POINT ( 'NONE',  ( -12.22686266070000194, -70.24095241330000761, -25.02007459860000083 ) ) ;
#16111 = DIRECTION ( 'NONE',  ( -6.123031769110000420E-17, 0.000000000000000000, 1.000000000000000000 ) ) ;
#16112 = CARTESIAN_POINT ( 'NONE',  ( 8.002080211126466835, -101.4862650398017792, 13.99634146016975755 ) ) ;
#16113 = FACE_OUTER_BOUND ( 'NONE', #20435, .T. ) ;
#16114 = CARTESIAN_POINT ( 'NONE',  ( -39.54203581779999865, -73.97629583739998793, -7.314380513039999698 ) ) ;
#16115 = EDGE_LOOP ( 'NONE', ( #25370, #3735, #24918, #10847 ) ) ;
#16116 = EDGE_CURVE ( 'NONE', #4525, #10505, #21753, .T. ) ;
#16117 = B_SPLINE_CURVE_WITH_KNOTS ( 'NONE', 3,
 ( #10148, #12475, #21389, #10017, #27811, #5521, #16595, #23446, #19069, #23712, #14269, #28088 ),
 .UNSPECIFIED., .F., .F.,
 ( 4, 2, 1, 1, 2, 2, 4 ),
 ( 0.000000000000000000, 0.2499999999999843459, 0.3749999999999700240, 0.4374999999999628630, 0.4687499999999649170, 0.4999999999999670264, 1.000000000000000000 ),
 .UNSPECIFIED. ) ;
#16118 = CARTESIAN_POINT ( 'NONE',  ( 27.03564186867965091, -92.52498922770500656, -14.11841734613871857 ) ) ;
#16119 = EDGE_LOOP ( 'NONE', ( #1845, #2674, #15986, #21128 ) ) ;
#16120 = EDGE_CURVE ( 'NONE', #4490, #4878, #11574, .T. ) ;
#16121 = ADVANCED_FACE ( 'NONE', ( #2825 ), #7816, .F. ) ;
#16122 = DIRECTION ( 'NONE',  ( 1.000000000000000000, 0.000000000000000000, 0.000000000000000000 ) ) ;
#16123 = CARTESIAN_POINT ( 'NONE',  ( 9.571688886909999638, -37.07368284070000186, -22.92823879609999693 ) ) ;
#16124 = CARTESIAN_POINT ( 'NONE',  ( -2.545777994589999871, -97.01677120690000322, 20.99408306970000382 ) ) ;
#16125 = CARTESIAN_POINT ( 'NONE',  ( 4.045673151789999089, -93.38241536079999605, 25.84256226979999838 ) ) ;
#16126 = ORIENTED_EDGE ( 'NONE', *, *, #25804, .F. ) ;
#16127 = CARTESIAN_POINT ( 'NONE',  ( -25.76781702903437221, -94.10917102444695104, -2.365844001559266108 ) ) ;
#16128 = CARTESIAN_POINT ( 'NONE',  ( 23.03829042120000281, -45.73899999920000425, 10.32398954119999956 ) ) ;
#16129 = CARTESIAN_POINT ( 'NONE',  ( 11.06094107680000072, -36.00000000000000000, -21.69991213999999857 ) ) ;
#16130 = ORIENTED_EDGE ( 'NONE', *, *, #23275, .T. ) ;
#16131 = CARTESIAN_POINT ( 'NONE',  ( 7.168130346672493936, -73.50999119020875128, -38.90877162602799189 ) ) ;
#16132 = CARTESIAN_POINT ( 'NONE',  ( -11.18243144779999909, -57.47855601759999900, 20.51090144570000007 ) ) ;
#16133 = CARTESIAN_POINT ( 'NONE',  ( -8.777511001860000661, -95.97839747389998877, -20.67514097709999987 ) ) ;
#16134 = CARTESIAN_POINT ( 'NONE',  ( 7.279457176439408705, -101.1604341890527365, 13.52204713848896311 ) ) ;
#16135 = CARTESIAN_POINT ( 'NONE',  ( -2.791011762119999684, -66.02175891730000501, -26.44799069369999955 ) ) ;
#16136 = CARTESIAN_POINT ( 'NONE',  ( -14.55867152370000106, -64.24504444460001196, 22.15151623919999935 ) ) ;
#16137 = ORIENTED_EDGE ( 'NONE', *, *, #28715, .T. ) ;
#16138 = CARTESIAN_POINT ( 'NONE',  ( 36.32450519430000213, -74.54297176320000062, -14.86961496900000057 ) ) ;
#16139 = B_SPLINE_CURVE_WITH_KNOTS ( 'NONE', 3,
 ( #25712, #9675, #687, #9537, #7528, #20919, #10643, #8620, #26129, #19702, #25851, #6009, #23525, #19556, #3561, #24074, #4114, #12557, #12836 ),
 .UNSPECIFIED., .F., .F.,
 ( 4, 2, 2, 2, 2, 2, 1, 2, 2, 4 ),
 ( 0.000000000000000000, 0.2499999999999938938, 0.3749999999999893419, 0.4374999999999886757, 0.4999999999999878986, 0.6249999999999861222, 0.6874999999999836797, 0.7187499999999837907, 0.7499999999999839018, 1.000000000000000000 ),
 .UNSPECIFIED. ) ;
#16140 = CARTESIAN_POINT ( 'NONE',  ( 13.81414405219999963, -99.85455315880000171, -10.14094832980000049 ) ) ;
#16141 = CARTESIAN_POINT ( 'NONE',  ( 25.78766439909999875, -63.04983560140001231, 1.379138088530000195 ) ) ;
#16142 = CARTESIAN_POINT ( 'NONE',  ( -5.679770007689999289, -74.50000000000000000, 47.25000000000000000 ) ) ;
#16143 = ORIENTED_EDGE ( 'NONE', *, *, #14787, .T. ) ;
#16144 = CARTESIAN_POINT ( 'NONE',  ( -12.42556073345063261, -101.1604341566395107, -9.024505522341051744 ) ) ;
#16145 = FACE_OUTER_BOUND ( 'NONE', #21257, .T. ) ;
#16146 = CARTESIAN_POINT ( 'NONE',  ( 0.2554224435499999890, -101.2010924020000004, -15.25977029010000052 ) ) ;
#16147 = CARTESIAN_POINT ( 'NONE',  ( 23.98651103399999940, -93.13202907830000754, -10.86104031880000065 ) ) ;
#16148 = ORIENTED_EDGE ( 'NONE', *, *, #14699, .F. ) ;
#16149 = ADVANCED_FACE ( 'NONE', ( #3808 ), #5981, .T. ) ;
#16150 = CARTESIAN_POINT ( 'NONE',  ( -7.498699138939999287, -94.79581646409999962, -22.45487619560000070 ) ) ;
#16151 = CARTESIAN_POINT ( 'NONE',  ( 31.00000000000000000, -13.00000000000000000, -4.500000000000000000 ) ) ;
#16152 = CARTESIAN_POINT ( 'NONE',  ( -39.50000000000000000, -65.63577453799999262, -2.309401076760000393 ) ) ;
#16153 = CARTESIAN_POINT ( 'NONE',  ( 16.49344491490923303, -100.3041487037201449, 4.352733011544403396 ) ) ;
#16154 = ORIENTED_EDGE ( 'NONE', *, *, #25951, .F. ) ;
#16155 = CARTESIAN_POINT ( 'NONE',  ( 23.03829042120000281, -52.56313962710000709, 10.32398954119999956 ) ) ;
#16156 = EDGE_CURVE ( 'NONE', #17343, #13209, #9023, .T. ) ;
#16157 = B_SPLINE_SURFACE_WITH_KNOTS ( 'NONE', 5, 5, ( 
 ( #3586, #12181, #12591, #10264, #19175, #1696, #10405, #25880, #14785 ),
 ( #10123, #12321, #3869, #12733, #23686, #17126, #21646, #26014, #6038 ),
 ( #14924, #10532, #19449, #7701, #1154, #9991, #7829, #5493, #14382 ),
 ( #23276, #23416, #3319, #21227, #1281, #19039, #27925, #7962, #16852 ),
 ( #15062, #15196, #11109, #20029, #21783, #15647, #21934, #10965, #95 ),
 ( #4300, #23971, #2128, #28622, #1836, #15345, #6334, #24114, #28756 ),
 ( #22371, #4008, #17273, #13021, #4148, #8796, #26452, #26752, #6484 ),
 ( #22220, #17709, #8654, #2267, #17557, #8944, #17853, #26595, #10826 ),
 ( #6784, #24261, #24550, #13316, #13172, #6636, #4590, #19593, #13465 ) ),
 .UNSPECIFIED., .F., .F., .F.,
 ( 6, 3, 6 ),
 ( 6, 3, 6 ),
 ( 7.186332008689999995, 18.82032538949999889, 25.08217526769999850 ),
 ( 0.000000000000000000, 0.2500000000000000000, 0.5000000000000000000 ),
 .UNSPECIFIED. ) ;
#16158 = CARTESIAN_POINT ( 'NONE',  ( -12.11470824010000058, -19.46971262549999793, 19.05681609440000202 ) ) ;
#16159 = CARTESIAN_POINT ( 'NONE',  ( -11.79008835590000004, -62.95225063429998613, -23.26928841850000040 ) ) ;
#16160 = DIRECTION ( 'NONE',  ( 0.2588190451029837025, 0.000000000000000000, -0.9659258262889443003 ) ) ;
#16161 = DIRECTION ( 'NONE',  ( 3.383536836950000192E-16, 0.000000000000000000, -1.000000000000000000 ) ) ;
#16162 = ORIENTED_EDGE ( 'NONE', *, *, #18345, .T. ) ;
#16163 = VECTOR ( 'NONE', #14489, 1000.000000000000000 ) ;
#16164 = DIRECTION ( 'NONE',  ( -0.7071067811865457964, 0.000000000000000000, -0.7071067811865492381 ) ) ;
#16165 = ORIENTED_EDGE ( 'NONE', *, *, #9439, .F. ) ;
#16166 = CARTESIAN_POINT ( 'NONE',  ( -13.16051759379999986, -19.41822420549999961, 19.76723058829999857 ) ) ;
#16167 = ORIENTED_EDGE ( 'NONE', *, *, #27993, .F. ) ;
#16168 = TOROIDAL_SURFACE ( 'NONE', #23611, 52.20000000000000284, 5.000000000000000000 ) ;
#16169 = LINE ( 'NONE', #5111, #22475 ) ;
#16170 = EDGE_LOOP ( 'NONE', ( #23279, #16883, #28606, #15816, #11348 ) ) ;
#16171 = CARTESIAN_POINT ( 'NONE',  ( 0.4184115225550000261, -93.00000000000000000, -30.38020727889999861 ) ) ;
#16172 = CARTESIAN_POINT ( 'NONE',  ( -10.48904628653374793, -19.47230014276397370, -20.17613036516116409 ) ) ;
#16173 = CARTESIAN_POINT ( 'NONE',  ( -13.12479279440870350, -101.5902664364219135, -9.227018890821359065 ) ) ;
#16174 = CARTESIAN_POINT ( 'NONE',  ( -10.47740691559999959, -19.48537698630000037, -21.16038778040000068 ) ) ;
#16175 = DIRECTION ( 'NONE',  ( 0.000000000000000000, 1.000000000000000000, 0.000000000000000000 ) ) ;
#16176 = EDGE_LOOP ( 'NONE', ( #9587, #1085, #38, #25034 ) ) ;
#16177 = CARTESIAN_POINT ( 'NONE',  ( -32.75733295119999866, -79.93903531290000331, -22.41678657819999998 ) ) ;
#16178 = CARTESIAN_POINT ( 'NONE',  ( 22.78264860270000014, -94.59276292389999696, -6.873201011689999085 ) ) ;
#16179 = FACE_OUTER_BOUND ( 'NONE', #6971, .T. ) ;
#16180 = ORIENTED_EDGE ( 'NONE', *, *, #8631, .T. ) ;
#16181 = EDGE_CURVE ( 'NONE', #1871, #7380, #16024, .T. ) ;
#16182 = CARTESIAN_POINT ( 'NONE',  ( -38.02338021417244107, -63.35089350796872765, -0.9476039871582396801 ) ) ;
#16183 = DIRECTION ( 'NONE',  ( 0.4794255386042040601, 0.000000000000000000, 0.8775825618903719816 ) ) ;
#16184 = DIRECTION ( 'NONE',  ( -0.9037419867099893978, 0.000000000000000000, 0.4280775881279952344 ) ) ;
#16185 = ORIENTED_EDGE ( 'NONE', *, *, #1002, .T. ) ;
#16186 = EDGE_CURVE ( 'NONE', #17262, #21247, #10419, .T. ) ;
#16187 = CIRCLE ( 'NONE', #28274, 0.5000000000000027756 ) ;
#16188 = CARTESIAN_POINT ( 'NONE',  ( -18.19850021250000083, -94.71481160550000311, 16.19177116950000084 ) ) ;
#16189 = CARTESIAN_POINT ( 'NONE',  ( -19.42841453280000152, -39.32886505740000160, 13.99550717529999844 ) ) ;
#16190 = DIRECTION ( 'NONE',  ( 0.4794255386042041156, 0.000000000000000000, 0.8775825618903722036 ) ) ;
#16191 = LINE ( 'NONE', #27142, #13576 ) ;
#16192 = CARTESIAN_POINT ( 'NONE',  ( -14.91714650195326186, -74.40777954432446961, 36.29798897348343445 ) ) ;
#16193 = EDGE_CURVE ( 'NONE', #8180, #9163, #6269, .T. ) ;
#16194 = CARTESIAN_POINT ( 'NONE',  ( 25.14693906469999973, -65.07443093669999712, -0.3759466479219999990 ) ) ;
#16195 = CIRCLE ( 'NONE', #19904, 3.749999999999996447 ) ;
#16196 = VERTEX_POINT ( 'NONE', #12951 ) ;
#16197 = B_SPLINE_CURVE_WITH_KNOTS ( 'NONE', 3,
 ( #26985, #7171, #487, #11364, #9180, #20269, #11052, #22169, #15891, #2208, #337, #37, #2803, #17798, #24942, #17654, #26689, #11657, #17945, #6730, #15596, #13408, #2357, #4835, #11510, #189, #18235, #26839, #6871, #15737, #13713, #11954, #14158 ),
 .UNSPECIFIED., .F., .F.,
 ( 4, 2, 1, 1, 2, 2, 1, 1, 1, 2, 2, 2, 1, 1, 2, 2, 1, 1, 2, 2, 4 ),
 ( 0.000000000000000000, 0.06249999999993549604, 0.09374999999991442956, 0.1093749999999134026, 0.1171874999999128891, 0.1249999999999123756, 0.1874999999998872846, 0.2187499999998759326, 0.2343749999998691325, 0.2421874999998724076, 0.2499999999998757105, 0.3749999999998923084, 0.4374999999998991362, 0.4687499999999059086, 0.4843749999999075739, 0.4999999999999092948, 0.6249999999999331646, 0.6874999999999445999, 0.7187499999999488187, 0.7499999999999531486, 1.000000000000000000 ),
 .UNSPECIFIED. ) ;
#16198 = CARTESIAN_POINT ( 'NONE',  ( 21.65402597960000008, -37.28545205309999488, -8.393872059200001345 ) ) ;
#16199 = CARTESIAN_POINT ( 'NONE',  ( 14.82656590110000039, -97.01677250859999901, 15.07996639799999983 ) ) ;
#16200 = ORIENTED_EDGE ( 'NONE', *, *, #4198, .F. ) ;
#16201 = DIRECTION ( 'NONE',  ( 0.8775825618903724257, 0.000000000000000000, 0.4794255386042037825 ) ) ;
#16202 = CARTESIAN_POINT ( 'NONE',  ( 7.627404847670000265, -18.50000000000000000, -19.58026728520000148 ) ) ;
#16203 = TOROIDAL_SURFACE ( 'NONE', #19909, 10.50000000000000000, 0.5000000000000000000 ) ;
#16204 = CARTESIAN_POINT ( 'NONE',  ( -7.944280978800001058, -100.1981337080000003, 15.01052544650000087 ) ) ;
#16205 = CARTESIAN_POINT ( 'NONE',  ( -18.14849333036523760, -18.49999996075505848, 11.13143091276801044 ) ) ;
#16206 = CARTESIAN_POINT ( 'NONE',  ( 0.000000000000000000, -39.50000000000000000, 0.000000000000000000 ) ) ;
#16207 = CARTESIAN_POINT ( 'NONE',  ( 8.980667191809999395, -36.11584072189999972, -20.70603881730000140 ) ) ;
#16208 = CARTESIAN_POINT ( 'NONE',  ( 7.286238495500000134, -101.2500498790000023, 13.33737010350000141 ) ) ;
#16209 = EDGE_LOOP ( 'NONE', ( #4840, #19447, #24211, #20139 ) ) ;
#16210 = CARTESIAN_POINT ( 'NONE',  ( -39.86740956975740602, -73.89318255927805978, 7.248796347619867575 ) ) ;
#16211 = CARTESIAN_POINT ( 'NONE',  ( -36.79999999999999716, -63.07912966450000880, 0.1732050807570000017 ) ) ;
#16212 = CARTESIAN_POINT ( 'NONE',  ( 11.60189548900000034, -99.55619081909999579, -13.07744430270000002 ) ) ;
#16213 = ORIENTED_EDGE ( 'NONE', *, *, #3350, .T. ) ;
#16214 = CARTESIAN_POINT ( 'NONE',  ( -2.166872423674899739, -19.47370675684711472, -22.73566057691103381 ) ) ;
#16215 = CARTESIAN_POINT ( 'NONE',  ( 11.90107424179999995, -101.3957169669999985, -10.67378013559999950 ) ) ;
#16216 = CARTESIAN_POINT ( 'NONE',  ( -2.041929835609999966, -39.34784663180000308, -23.26788540500000124 ) ) ;
#16217 = CARTESIAN_POINT ( 'NONE',  ( 14.81349357762022478, -95.37019131402171013, 17.32245915622085519 ) ) ;
#16218 = ADVANCED_FACE ( 'NONE', ( #7907 ), #4992, .F. ) ;
#16219 = EDGE_CURVE ( 'NONE', #26789, #15187, #11848, .T. ) ;
#16220 = DIRECTION ( 'NONE',  ( 1.000000000000000000, 0.000000000000000000, 0.000000000000000000 ) ) ;
#16221 = CARTESIAN_POINT ( 'NONE',  ( 22.17287314020000011, -57.47832541620000057, -7.362282719720000479 ) ) ;
#16222 = EDGE_CURVE ( 'NONE', #25027, #13019, #16969, .T. ) ;
#16223 = SPHERICAL_SURFACE ( 'NONE', #24383, 2.000000000000000000 ) ;
#16224 = VERTEX_POINT ( 'NONE', #20521 ) ;
#16225 = CIRCLE ( 'NONE', #25560, 55.50192378860000275 ) ;
#16226 = CARTESIAN_POINT ( 'NONE',  ( 6.901963694340000011, -101.4908759489999994, 14.46911387129999937 ) ) ;
#16227 = CARTESIAN_POINT ( 'NONE',  ( -32.83566817450000030, -79.50000000000000000, -22.22906645670000003 ) ) ;
#16228 = AXIS2_PLACEMENT_3D ( 'NONE', #2104, #6759, #24084 ) ;
#16229 = CARTESIAN_POINT ( 'NONE',  ( 7.640382384829999651, -101.0974005930000033, 13.42254915319999853 ) ) ;
#16230 = CARTESIAN_POINT ( 'NONE',  ( -14.22861622210000121, -68.06112402509999981, 22.55404109870000084 ) ) ;
#16231 = CARTESIAN_POINT ( 'NONE',  ( 7.828355059359999757, -35.91213417740000580, -21.38475576599999783 ) ) ;
#16232 = CARTESIAN_POINT ( 'NONE',  ( 36.32249705850000510, -79.79205832529999043, -14.87545865919999954 ) ) ;
#16233 = CARTESIAN_POINT ( 'NONE',  ( -0.8452062098759994813, -52.63280639819944184, -23.17863372589996729 ) ) ;
#16234 = CARTESIAN_POINT ( 'NONE',  ( 2.412292587909999959E-12, -111.0000000000000000, -5.497824417940001177E-12 ) ) ;
#16235 = DIRECTION ( 'NONE',  ( 0.000000000000000000, -1.000000000000000000, 0.000000000000000000 ) ) ;
#16236 = EDGE_CURVE ( 'NONE', #21652, #1569, #22082, .T. ) ;
#16237 = CARTESIAN_POINT ( 'NONE',  ( 16.78053306740000039, -99.78393592979999482, 4.299646967080000159 ) ) ;
#16238 = ORIENTED_EDGE ( 'NONE', *, *, #4571, .F. ) ;
#16239 = CONICAL_SURFACE ( 'NONE', #10598, 24.40223267850002031, 0.7949521073230001456 ) ;
#16240 = CARTESIAN_POINT ( 'NONE',  ( 8.140397668380000340, -100.8869818179999953, 13.38618156149999905 ) ) ;
#16241 = DIRECTION ( 'NONE',  ( 1.000000000000000000, 0.000000000000000000, 0.000000000000000000 ) ) ;
#16242 = VERTEX_POINT ( 'NONE', #4518 ) ;
#16243 = CARTESIAN_POINT ( 'NONE',  ( 9.127577618711740115, -92.82334897400379248, 29.10218788055306405 ) ) ;
#16244 = ORIENTED_EDGE ( 'NONE', *, *, #18279, .F. ) ;
#16245 = CIRCLE ( 'NONE', #3690, 19.99999999999999645 ) ;
#16246 = CIRCLE ( 'NONE', #22301, 7.000000000000000000 ) ;
#16247 = CARTESIAN_POINT ( 'NONE',  ( 0.6074919593152650066, -100.4872618012716288, -16.90062116310696894 ) ) ;
#16248 = DIRECTION ( 'NONE',  ( 0.4794255386042041156, 0.000000000000000000, 0.8775825618903722036 ) ) ;
#16249 = CIRCLE ( 'NONE', #3694, 25.14975229270000057 ) ;
#16250 = CARTESIAN_POINT ( 'NONE',  ( 47.25000000000000000, -79.00000000000000000, -6.875000000000000000 ) ) ;
#16251 = DIRECTION ( 'NONE',  ( 0.000000000000000000, 1.000000000000000000, 0.000000000000000000 ) ) ;
#16252 = EDGE_CURVE ( 'NONE', #24500, #15581, #3475, .T. ) ;
#16253 = CARTESIAN_POINT ( 'NONE',  ( -14.35888481029999930, -74.08594823550001252, 36.31399993319999453 ) ) ;
#16254 = CARTESIAN_POINT ( 'NONE',  ( -21.35785820959999981, -65.07443093669999712, 13.27974662679999973 ) ) ;
#16255 = CARTESIAN_POINT ( 'NONE',  ( 13.89851760690000049, -96.93384555689999615, -16.12486289770000170 ) ) ;
#16256 = ORIENTED_EDGE ( 'NONE', *, *, #26735, .T. ) ;
#16257 = CARTESIAN_POINT ( 'NONE',  ( -12.12177392010000077, -71.84927287379998972, -25.80509671639999780 ) ) ;
#16258 = CARTESIAN_POINT ( 'NONE',  ( 8.988997220999999982, -34.66800423669999276, -19.43643757559999941 ) ) ;
#16259 = DIRECTION ( 'NONE',  ( 0.5503273727321511544, 0.000000000000000000, 0.8349489701902315097 ) ) ;
#16260 = DIRECTION ( 'NONE',  ( -0.7071067811865474617, 0.000000000000000000, 0.7071067811865474617 ) ) ;
#16261 = CARTESIAN_POINT ( 'NONE',  ( -38.70548920639999579, -73.81415963839999961, -7.196176986149999344 ) ) ;
#16262 = ORIENTED_EDGE ( 'NONE', *, *, #3374, .T. ) ;
#16263 = EDGE_LOOP ( 'NONE', ( #10180, #5712, #15032, #6778 ) ) ;
#16264 = VECTOR ( 'NONE', #19838, 1000.000000000000000 ) ;
#16265 = AXIS2_PLACEMENT_3D ( 'NONE', #27798, #27940, #28465 ) ;
#16266 = CARTESIAN_POINT ( 'NONE',  ( -1.156004284370000024, -57.47571004099999925, -23.39939383540000151 ) ) ;
#16267 = CARTESIAN_POINT ( 'NONE',  ( 6.981684465299999864, -101.1889999979999999, 29.03810821740000137 ) ) ;
#16268 = CARTESIAN_POINT ( 'NONE',  ( -0.8119073803659999644, -95.90105813370000476, 22.89043856289999823 ) ) ;
#16269 = CARTESIAN_POINT ( 'NONE',  ( 5.686419033639999121, -92.95927362729999288, 26.23007088160000322 ) ) ;
#16270 = VERTEX_POINT ( 'NONE', #13397 ) ;
#16271 = EDGE_CURVE ( 'NONE', #13154, #21711, #24578, .T. ) ;
#16272 = CARTESIAN_POINT ( 'NONE',  ( 36.70830968599999977, -79.25000000000000000, -15.25000000000000000 ) ) ;
#16273 = DIRECTION ( 'NONE',  ( 0.000000000000000000, 1.000000000000000000, 0.000000000000000000 ) ) ;
#16274 = CARTESIAN_POINT ( 'NONE',  ( 46.69678069119999719, -74.07637432209999417, -3.237587372219999704 ) ) ;
#16275 = ORIENTED_EDGE ( 'NONE', *, *, #2048, .F. ) ;
#16276 = CARTESIAN_POINT ( 'NONE',  ( 7.244980372382691769, -74.16605908736325148, -40.26982517619838831 ) ) ;
#16277 = CARTESIAN_POINT ( 'NONE',  ( -12.24789267329999909, -65.07443093669999712, 21.96586363990000024 ) ) ;
#16278 = EDGE_CURVE ( 'NONE', #5957, #22342, #16280, .T. ) ;
#16279 = ORIENTED_EDGE ( 'NONE', *, *, #9091, .T. ) ;
#16280 = LINE ( 'NONE', #3329, #22554 ) ;
#16281 = CARTESIAN_POINT ( 'NONE',  ( 46.25000000000000000, -79.00000000000000000, -13.75000000000000000 ) ) ;
#16282 = CARTESIAN_POINT ( 'NONE',  ( -2.417371786180000370, -65.72572872239999242, -25.90137666380000070 ) ) ;
#16283 = EDGE_CURVE ( 'NONE', #12443, #15684, #23551, .T. ) ;
#16284 = AXIS2_PLACEMENT_3D ( 'NONE', #12024, #3444, #7819 ) ;
#16285 = CARTESIAN_POINT ( 'NONE',  ( -15.68772883089999937, -69.50482905820000212, 23.03878850240000276 ) ) ;
#16286 = EDGE_LOOP ( 'NONE', ( #5239, #21823, #10440, #4660 ) ) ;
#16287 = CIRCLE ( 'NONE', #20475, 0.3500000000000003664 ) ;
#16288 = VECTOR ( 'NONE', #8373, 1000.000000000000000 ) ;
#16289 = CARTESIAN_POINT ( 'NONE',  ( -14.59919365920000089, -79.49999999012054275, 36.80099835649999562 ) ) ;
#16290 = CARTESIAN_POINT ( 'NONE',  ( -15.55924707670000018, -101.2720154369999932, 3.463031180029999767 ) ) ;
#16291 = DIRECTION ( 'NONE',  ( 0.000000000000000000, -1.000000000000000000, 0.000000000000000000 ) ) ;
#16292 = CARTESIAN_POINT ( 'NONE',  ( 36.28164458690000060, -74.50000000000000000, -14.97346873880000118 ) ) ;
#16293 = ORIENTED_EDGE ( 'NONE', *, *, #11877, .F. ) ;
#16294 = DIRECTION ( 'NONE',  ( 1.000000000000000000, 0.000000000000000000, 0.000000000000000000 ) ) ;
#16295 = CARTESIAN_POINT ( 'NONE',  ( -1.565549855109999777, -18.61786835250000038, -21.74208210369999961 ) ) ;
#16296 = CARTESIAN_POINT ( 'NONE',  ( 24.12664335590000064, -92.56290624670000966, -15.50499703690000075 ) ) ;
#16297 = VERTEX_POINT ( 'NONE', #20817 ) ;
#16298 = CARTESIAN_POINT ( 'NONE',  ( -8.594687425180000062, -94.47838212999999996, -22.80941933420000112 ) ) ;
#16299 = CARTESIAN_POINT ( 'NONE',  ( 22.94569809939999772, -61.52579421249999569, 10.37789087800000054 ) ) ;
#16300 = CARTESIAN_POINT ( 'NONE',  ( 34.06016921999999880, -74.00000000000000000, -4.978042818679999648 ) ) ;
#16301 = CARTESIAN_POINT ( 'NONE',  ( 16.83483077069999823, -99.92967571559999840, 4.239603657359999112 ) ) ;
#16302 = DIRECTION ( 'NONE',  ( 0.4794255386042040601, 0.000000000000000000, 0.8775825618903720926 ) ) ;
#16303 = ORIENTED_EDGE ( 'NONE', *, *, #20063, .T. ) ;
#16304 = CARTESIAN_POINT ( 'NONE',  ( 47.25000000000000000, -79.00000000000000000, -7.718270467189999824E-13 ) ) ;
#16305 = CARTESIAN_POINT ( 'NONE',  ( -12.11761160510000046, -19.16174953630000033, 19.04753198859999941 ) ) ;
#16306 = APPLICATION_CONTEXT ( 'automotive_design' ) ;
#16307 = AXIS2_PLACEMENT_3D ( 'NONE', #6170, #4278, #19300 ) ;
#16308 = CARTESIAN_POINT ( 'NONE',  ( 23.73263625450000092, -64.92652906329999496, -8.873745374080000303 ) ) ;
#16309 = CARTESIAN_POINT ( 'NONE',  ( 3.812263950998352691, -93.98965247056261774, 25.83266599306846700 ) ) ;
#16310 = CIRCLE ( 'NONE', #13018, 0.5000000000000004441 ) ;
#16311 = ORIENTED_EDGE ( 'NONE', *, *, #27465, .T. ) ;
#16312 = CIRCLE ( 'NONE', #2366, 8.999999999999998224 ) ;
#16313 = DIRECTION ( 'NONE',  ( 0.01673171000360159852, -0.9993908270190947629, 0.03062718972490289376 ) ) ;
#16314 = CARTESIAN_POINT ( 'NONE',  ( 11.70455088819999823, -92.50000000000000000, 8.942783294160001617 ) ) ;
#16315 = ORIENTED_EDGE ( 'NONE', *, *, #18437, .T. ) ;
#16316 = CARTESIAN_POINT ( 'NONE',  ( -5.761619419100000528, -101.1130130960000031, 14.30911249059999868 ) ) ;
#16317 = EDGE_LOOP ( 'NONE', ( #27214, #1424, #9271, #2750 ) ) ;
#16318 = ADVANCED_FACE ( 'NONE', ( #3464 ), #2925, .T. ) ;
#16319 = CARTESIAN_POINT ( 'NONE',  ( 0.000000000000000000, -30.20000000000000284, 0.000000000000000000 ) ) ;
#16320 = ADVANCED_FACE ( 'NONE', ( #21947 ), #21513, .F. ) ;
#16321 = ORIENTED_EDGE ( 'NONE', *, *, #15617, .F. ) ;
#16322 = CARTESIAN_POINT ( 'NONE',  ( 39.23631979950000215, -73.50064222359999633, 7.229366192799999702 ) ) ;
#16323 = CARTESIAN_POINT ( 'NONE',  ( -10.81241633620959774, -19.46574764917406242, -19.41094217333082383 ) ) ;
#16324 = EDGE_CURVE ( 'NONE', #28714, #26809, #12877, .T. ) ;
#16325 = CARTESIAN_POINT ( 'NONE',  ( -10.00361297630000124, -18.62004679909999894, -20.76967538030000071 ) ) ;
#16326 = DIRECTION ( 'NONE',  ( 0.000000000000000000, 0.000000000000000000, 1.000000000000000000 ) ) ;
#16327 = ORIENTED_EDGE ( 'NONE', *, *, #20476, .F. ) ;
#16328 = ADVANCED_FACE ( 'NONE', ( #2135 ), #20709, .T. ) ;
#16329 = DIRECTION ( 'NONE',  ( 1.000000000000000000, 0.000000000000000000, 0.000000000000000000 ) ) ;
#16330 = CARTESIAN_POINT ( 'NONE',  ( 13.12744653600000078, -94.59276292389999696, -19.84842857619999990 ) ) ;
#16331 = CARTESIAN_POINT ( 'NONE',  ( 26.60903970598167589, -15.80000000000000071, 48.70752046822583736 ) ) ;
#16332 = CARTESIAN_POINT ( 'NONE',  ( 46.25000000000000000, -74.00000000000000000, -13.75000000000000000 ) ) ;
#16333 = ORIENTED_EDGE ( 'NONE', *, *, #11904, .T. ) ;
#16334 = CIRCLE ( 'NONE', #14911, 14.25000000000000000 ) ;
#16335 = DIRECTION ( 'NONE',  ( 0.4794255386042036160, 0.000000000000000000, 0.8775825618903723147 ) ) ;
#16336 = CARTESIAN_POINT ( 'NONE',  ( -19.81272040990000249, -52.63293862049999916, 12.05498172269999912 ) ) ;
#16337 = DIRECTION ( 'NONE',  ( -0.3687499999999814260, 0.000000000000000000, 0.9295286103719527793 ) ) ;
#16338 = ORIENTED_EDGE ( 'NONE', *, *, #6470, .T. ) ;
#16339 = AXIS2_PLACEMENT_3D ( 'NONE', #2454, #15679, #4625 ) ;
#16340 = CARTESIAN_POINT ( 'NONE',  ( -18.00116235329999625, -97.01638956499999722, 11.09997051220000053 ) ) ;
#16341 = AXIS2_PLACEMENT_3D ( 'NONE', #18387, #11811, #188 ) ;
#16342 = CARTESIAN_POINT ( 'NONE',  ( -19.29069590680000346, -45.99312545570000310, 12.83330259409999918 ) ) ;
#16343 = FACE_OUTER_BOUND ( 'NONE', #20479, .T. ) ;
#16344 = CARTESIAN_POINT ( 'NONE',  ( -38.14025503984489518, -65.74398723832256053, 1.129426529332413720 ) ) ;
#16345 = CARTESIAN_POINT ( 'NONE',  ( -14.85724926008588120, -74.31785917165720434, 36.29292894000464997 ) ) ;
#16346 = B_SPLINE_CURVE_WITH_KNOTS ( 'NONE', 3,
 ( #25761, #23845, #8248, #12202, #3748, #16729, #19337, #26181, #21379, #27946, #16874, #5790, #14674, #23568, #21522, #1579, #10420 ),
 .UNSPECIFIED., .F., .F.,
 ( 4, 2, 2, 1, 1, 1, 1, 1, 2, 2, 4 ),
 ( 0.000000000000000000, 0.2500000000000119904, 0.3750000000000182077, 0.4375000000000205391, 0.4687500000000224820, 0.4843750000000234812, 0.4921875000000247025, 0.4960937500000253686, 0.4980468750000248690, 0.5000000000000244249, 1.000000000000000000 ),
 .UNSPECIFIED. ) ;
#16347 = CARTESIAN_POINT ( 'NONE',  ( 26.08584741079999958, -65.97406652829999985, 1.199274931579999981 ) ) ;
#16348 = CARTESIAN_POINT ( 'NONE',  ( 8.354902469970001633, -98.70454033420000428, 16.50015517690000166 ) ) ;
#16349 = EDGE_LOOP ( 'NONE', ( #28425, #13934, #3359, #27065 ) ) ;
#16350 = CARTESIAN_POINT ( 'NONE',  ( 36.70830968599999977, -79.25000000000000000, -14.75000000000000000 ) ) ;
#16351 = EDGE_CURVE ( 'NONE', #2153, #3841, #18373, .T. ) ;
#16352 = CARTESIAN_POINT ( 'NONE',  ( 19.58569113819999785, -94.54719592040000009, 13.61988814439999906 ) ) ;
#16353 = EDGE_LOOP ( 'NONE', ( #18335, #23966, #2590, #12398 ) ) ;
#16354 = AXIS2_PLACEMENT_3D ( 'NONE', #10666, #19859, #20010 ) ;
#16355 = CARTESIAN_POINT ( 'NONE',  ( 7.215414233289999757, -74.50000000000000000, 40.70731707320000226 ) ) ;
#16356 = DIRECTION ( 'NONE',  ( 0.000000000000000000, 1.000000000000000000, 0.000000000000000000 ) ) ;
#16357 = CIRCLE ( 'NONE', #24742, 59.04999999999999716 ) ;
#16358 = ADVANCED_FACE ( 'NONE', ( #21792 ), #10835, .F. ) ;
#16359 = AXIS2_PLACEMENT_3D ( 'NONE', #15264, #15572, #24182 ) ;
#16360 = DIRECTION ( 'NONE',  ( 0.4794255386042036715, 0.000000000000000000, 0.8775825618903724257 ) ) ;
#16361 = DIRECTION ( 'NONE',  ( 5.788992577199957397E-17, 0.000000000000000000, -1.000000000000000000 ) ) ;
#16362 = CARTESIAN_POINT ( 'NONE',  ( 7.601924345689999640, -101.4240865590000027, 14.04435494200000001 ) ) ;
#16363 = ORIENTED_EDGE ( 'NONE', *, *, #23619, .T. ) ;
#16364 = EDGE_CURVE ( 'NONE', #7118, #3430, #14514, .T. ) ;
#16365 = CARTESIAN_POINT ( 'NONE',  ( -39.34253424958686907, -73.62781383917049993, 7.220129148632251415 ) ) ;
#16366 = DIRECTION ( 'NONE',  ( 0.000000000000000000, -1.000000000000000000, 0.000000000000000000 ) ) ;
#16367 = CARTESIAN_POINT ( 'NONE',  ( 11.43947858090000125, -98.26007807919999948, -15.36247001880000163 ) ) ;
#16368 = VERTEX_POINT ( 'NONE', #9399 ) ;
#16369 = CARTESIAN_POINT ( 'NONE',  ( -2.442775742550781448, -19.48034373447696765, -23.15154483919690165 ) ) ;
#16370 = CARTESIAN_POINT ( 'NONE',  ( 11.97711149329999891, -101.3256027139999986, -10.46763994119999985 ) ) ;
#16371 = CARTESIAN_POINT ( 'NONE',  ( -2.440432358250000267, -32.69575302460000188, -23.63442551149999815 ) ) ;
#16372 = CARTESIAN_POINT ( 'NONE',  ( -17.05616532261941742, -92.82529299097730302, 25.28511888657223139 ) ) ;
#16373 = CARTESIAN_POINT ( 'NONE',  ( -37.87497158468980274, -65.68892059713630260, 0.8034379168488015033 ) ) ;
#16374 = DIRECTION ( 'NONE',  ( 1.000000000000000000, 0.000000000000000000, 8.881784197000000500E-17 ) ) ;
#16375 = CARTESIAN_POINT ( 'NONE',  ( 23.29174250550000025, -49.04525650219999733, -9.486381418089997908 ) ) ;
#16376 = DIRECTION ( 'NONE',  ( 1.000000000000000000, 0.000000000000000000, 0.000000000000000000 ) ) ;
#16377 = CARTESIAN_POINT ( 'NONE',  ( -1.776356839399999804E-15, -80.50000000000000000, 3.552713678799999214E-14 ) ) ;
#16378 = AXIS2_PLACEMENT_3D ( 'NONE', #25974, #5050, #27210 ) ;
#16379 = ORIENTED_EDGE ( 'NONE', *, *, #2594, .T. ) ;
#16380 = B_SPLINE_CURVE_WITH_KNOTS ( 'NONE', 3,
 ( #19997, #4270, #1956, #70, #6609, #13290, #24236, #10800, #8766, #4121, #19710, #8491, #12994, #8916, #22194, #3845, #2235, #11080, #17679, #26567, #12844, #8625, #17391, #1675, #26285, #28728, #28308, #8342, #21758, #13145, #26423, #24377, #12709, #26719, #28597, #21624, #17247, #17825, #19845, #10512, #17533, #19428, #10651, #19568, #26139, #15034, #17970, #2539, #7052, #20446, #22341, #362, #221, #27010, #20150, #9067, #13741, #22641, #2680, #516 ),
 .UNSPECIFIED., .F., .F.,
 ( 4, 2, 1, 1, 2, 2, 2, 2, 1, 1, 2, 2, 2, 2, 2, 2, 2, 1, 1, 2, 2, 2, 2, 1, 2, 2, 2, 1, 2, 2, 2, 2, 2, 4 ),
 ( 0.000000000000000000, 0.06250000000003833045, 0.09375000000005272172, 0.1093750000000599104, 0.1171875000000641293, 0.1250000000000683342, 0.1875000000000456302, 0.2187500000000350553, 0.2343750000000292821, 0.2421875000000203448, 0.2460937500000166256, 0.2500000000000128786, 0.3124999999999367173, 0.3437499999998986921, 0.3749999999998606115, 0.4374999999997844502, 0.4687499999997468692, 0.4843749999997351008, 0.4921874999997297162, 0.4960937499997356559, 0.4999999999997415956, 0.5624999999997376543, 0.5937499999997348787, 0.6093749999997334355, 0.6171874999997395417, 0.6249999999997456479, 0.6874999999997927214, 0.7187499999998162581, 0.7343749999998224753, 0.7499999999998285816, 0.8124999999998643307, 0.8437499999998877565, 0.8749999999999110711, 1.000000000000000000 ),
 .UNSPECIFIED. ) ;
#16381 = CARTESIAN_POINT ( 'NONE',  ( -32.65351228499999792, -74.41869006989999491, -21.85723935310000243 ) ) ;
#16382 = CARTESIAN_POINT ( 'NONE',  ( -32.69645379630000548, -79.50000000000076739, -21.71458329359999695 ) ) ;
#16383 = CARTESIAN_POINT ( 'NONE',  ( -14.19188855770000046, -80.00000000000000000, 37.13021410070000883 ) ) ;
#16384 = CARTESIAN_POINT ( 'NONE',  ( 20.95510892579999762, -35.33620225780000368, -8.408939989400000314 ) ) ;
#16385 = DIRECTION ( 'NONE',  ( 0.4794255386042000078, 0.000000000000000000, 0.8775825618903743131 ) ) ;
#16386 = DIRECTION ( 'NONE',  ( 1.000000000000000000, 0.000000000000000000, 0.000000000000000000 ) ) ;
#16387 = CARTESIAN_POINT ( 'NONE',  ( 21.24216623919999947, -36.23976085479999654, -9.027383814959998531 ) ) ;
#16388 = FACE_OUTER_BOUND ( 'NONE', #7010, .T. ) ;
#16389 = EDGE_CURVE ( 'NONE', #6476, #26414, #2869, .T. ) ;
#16390 = DIRECTION ( 'NONE',  ( 0.000000000000000000, 1.000000000000000000, 0.000000000000000000 ) ) ;
#16391 = ORIENTED_EDGE ( 'NONE', *, *, #17445, .F. ) ;
#16392 = SURFACE_STYLE_FILL_AREA ( #7535 ) ;
#16393 = B_SPLINE_CURVE_WITH_KNOTS ( 'NONE', 3,
 ( #18672, #10033, #1198, #27570, #7611, #16173, #13999, #18947, #27831, #23464, #5263, #3503 ),
 .UNSPECIFIED., .F., .F.,
 ( 4, 2, 2, 2, 2, 4 ),
 ( 0.000000000000000000, 0.2499999999999856781, 0.3749999999999847344, 0.4374999999999733546, 0.4999999999999619194, 1.000000000000000000 ),
 .UNSPECIFIED. ) ;
#16394 = CARTESIAN_POINT ( 'NONE',  ( -24.07228109569999930, -94.80026829410000744, -4.144186737870000137 ) ) ;
#16395 = ORIENTED_EDGE ( 'NONE', *, *, #25218, .F. ) ;
#16396 = AXIS2_PLACEMENT_3D ( 'NONE', #10458, #6549, #28394 ) ;
#16397 = DIRECTION ( 'NONE',  ( 0.000000000000000000, -1.000000000000000000, 0.000000000000000000 ) ) ;
#16398 = ORIENTED_EDGE ( 'NONE', *, *, #19917, .F. ) ;
#16399 = EDGE_CURVE ( 'NONE', #7945, #3493, #3912, .T. ) ;
#16400 = B_SPLINE_CURVE_WITH_KNOTS ( 'NONE', 3,
 ( #9391, #20473, #253, #7083, #390, #836 ),
 .UNSPECIFIED., .F., .F.,
 ( 4, 2, 4 ),
 ( 0.000000000000000000, 0.5000000000000000000, 1.000000000000000000 ),
 .UNSPECIFIED. ) ;
#16401 = CARTESIAN_POINT ( 'NONE',  ( 0.4381803858471648438, -99.99762666406154210, -17.29986369493340703 ) ) ;
#16402 = B_SPLINE_CURVE_WITH_KNOTS ( 'NONE', 5,
 ( #27265, #625, #5534, #13846, #16469, #20714 ),
 .UNSPECIFIED., .F., .F.,
 ( 6, 6 ),
 ( 0.000000000000000000, 6.855861996820000748 ),
 .UNSPECIFIED. ) ;
#16403 = CARTESIAN_POINT ( 'NONE',  ( -7.250077434679999655, -74.05347990799999991, 40.00006844429999830 ) ) ;
#16404 = CARTESIAN_POINT ( 'NONE',  ( -11.94559458280000008, -100.4792519539999915, -10.93369168340000108 ) ) ;
#16405 = CARTESIAN_POINT ( 'NONE',  ( -7.243843118864345954, -74.18716007590187189, -40.29875214189355859 ) ) ;
#16406 = CARTESIAN_POINT ( 'NONE',  ( -21.69477569840000086, -66.11096492830000670, 13.63249283160000047 ) ) ;
#16407 = CARTESIAN_POINT ( 'NONE',  ( 13.60163640490000070, -95.66919271840001215, -17.93630288140000317 ) ) ;
#16408 = B_SPLINE_SURFACE_WITH_KNOTS ( 'NONE', 4, 5, ( 
 ( #1282, #19040, #28066, #8102, #16991, #8946, #24409, #28758, #8655 ),
 ( #21935, #13317, #15346, #26169, #6193, #15063, #4302, #4445, #19736 ),
 ( #15648, #10827, #8797, #4009, #6785, #23972, #28623, #24551, #12867 ),
 ( #26312, #6335, #26596, #8519, #26453, #21784, #1837, #17710, #22221 ),
 ( #10680, #11111, #24262, #10966, #24115, #17560, #15499, #13022, #2268 ) ),
 .UNSPECIFIED., .F., .F., .F.,
 ( 5, 5 ),
 ( 6, 3, 6 ),
 ( 0.000000000000000000, 6.855861996759999855 ),
 ( 0.000000000000000000, 1.000000000000000000, 2.000000000000000000 ),
 .UNSPECIFIED. ) ;
#16409 = VERTEX_POINT ( 'NONE', #24716 ) ;
#16410 = CARTESIAN_POINT ( 'NONE',  ( 0.000000000000000000, -42.50000000000000000, 0.000000000000000000 ) ) ;
#16411 = CARTESIAN_POINT ( 'NONE',  ( 8.516252544429999460, -25.51643856499999785, -20.42955993270000192 ) ) ;
#16412 = DIRECTION ( 'NONE',  ( 0.000000000000000000, 0.000000000000000000, 1.000000000000000000 ) ) ;
#16413 = DIRECTION ( 'NONE',  ( 1.000000000000000000, 0.000000000000000000, 0.000000000000000000 ) ) ;
#16414 = ORIENTED_EDGE ( 'NONE', *, *, #4334, .F. ) ;
#16415 = CARTESIAN_POINT ( 'NONE',  ( -2.796429754430000392E-12, -111.0000000000000000, -5.314859663490001141E-12 ) ) ;
#16416 = ADVANCED_FACE ( 'NONE', ( #6646 ), #25812, .F. ) ;
#16417 = AXIS2_PLACEMENT_3D ( 'NONE', #18517, #1058, #9756 ) ;
#16418 = VERTEX_POINT ( 'NONE', #22229 ) ;
#16419 = VECTOR ( 'NONE', #27891, 1000.000000000000000 ) ;
#16420 = CARTESIAN_POINT ( 'NONE',  ( -1.450026333500000097, -57.90606206700000058, -23.52488548770000065 ) ) ;
#16421 = CARTESIAN_POINT ( 'NONE',  ( -2.332908480600000001, -96.95622424260000116, 20.76785060539999961 ) ) ;
#16422 = CARTESIAN_POINT ( 'NONE',  ( 11.27141356559999963, -93.01024347330000808, 27.60408353590000274 ) ) ;
#16423 = ORIENTED_EDGE ( 'NONE', *, *, #19109, .T. ) ;
#16424 = EDGE_CURVE ( 'NONE', #2868, #2641, #11723, .T. ) ;
#16425 = CIRCLE ( 'NONE', #5737, 0.4999999999999967804 ) ;
#16426 = CARTESIAN_POINT ( 'NONE',  ( -29.71161737690000137, -93.00000000000000000, 6.352311025380000586 ) ) ;
#16427 = FACE_OUTER_BOUND ( 'NONE', #17782, .T. ) ;
#16428 = FACE_OUTER_BOUND ( 'NONE', #2663, .T. ) ;
#16429 = ORIENTED_EDGE ( 'NONE', *, *, #18744, .T. ) ;
#16430 = CARTESIAN_POINT ( 'NONE',  ( 7.244343739429285556, -74.17816432833343754, -40.28633210784942520 ) ) ;
#16431 = CARTESIAN_POINT ( 'NONE',  ( -11.38279485941639635, -60.73290390095194624, 20.83642922985102075 ) ) ;
#16432 = B_SPLINE_CURVE_WITH_KNOTS ( 'NONE', 5,
 ( #11647, #27703, #771, #5260, #3224, #9616 ),
 .UNSPECIFIED., .F., .F.,
 ( 6, 6 ),
 ( 0.000000000000000000, 1.000000000000000000 ),
 .UNSPECIFIED. ) ;
#16433 = ADVANCED_FACE ( 'NONE', ( #9554 ), #15547, .F. ) ;
#16434 = CARTESIAN_POINT ( 'NONE',  ( -14.60044964929999978, -79.81260323630000642, 36.96978765280000090 ) ) ;
#16435 = DIRECTION ( 'NONE',  ( 0.7887177114147766455, 0.000000000000000000, 0.6147555381618264869 ) ) ;
#16436 = AXIS2_PLACEMENT_3D ( 'NONE', #2275, #8807, #1992 ) ;
#16437 = CARTESIAN_POINT ( 'NONE',  ( -2.513036490069999740, -70.69114014160000181, -27.60015579919999951 ) ) ;
#16438 = AXIS2_PLACEMENT_3D ( 'NONE', #8177, #14996, #10613 ) ;
#16439 = CARTESIAN_POINT ( 'NONE',  ( -14.17294541280000075, -69.11954792669999392, 22.97751744570000199 ) ) ;
#16440 = VERTEX_POINT ( 'NONE', #13325 ) ;
#16441 = CARTESIAN_POINT ( 'NONE',  ( -6.781378104809999030, -101.1889999979999999, 14.49182221120000058 ) ) ;
#16442 = CARTESIAN_POINT ( 'NONE',  ( -16.71474937220000001, -100.0946963879999885, 3.139046040560000250 ) ) ;
#16443 = CARTESIAN_POINT ( 'NONE',  ( 25.32712258629999980, -57.40875702469999453, 1.379782075540000097 ) ) ;
#16444 = CARTESIAN_POINT ( 'NONE',  ( -21.27071965929999564, -64.35840737889999730, 15.42050345319999849 ) ) ;
#16445 = ORIENTED_EDGE ( 'NONE', *, *, #13809, .F. ) ;
#16446 = CARTESIAN_POINT ( 'NONE',  ( 11.70455088819999823, -111.0000000000000000, 8.942783294160001617 ) ) ;
#16447 = CARTESIAN_POINT ( 'NONE',  ( -2.657761925540000014, -19.49504784870000051, -24.02235578410000372 ) ) ;
#16448 = FACE_OUTER_BOUND ( 'NONE', #5085, .T. ) ;
#16449 = ORIENTED_EDGE ( 'NONE', *, *, #22051, .F. ) ;
#16450 = CARTESIAN_POINT ( 'NONE',  ( -13.93182733059999912, -18.50000000000000000, 19.17753782289999975 ) ) ;
#16451 = ADVANCED_FACE ( 'NONE', ( #27197 ), #22537, .T. ) ;
#16452 = VECTOR ( 'NONE', #7915, 999.9999999999998863 ) ;
#16453 = LINE ( 'NONE', #16735, #8380 ) ;
#16454 = CARTESIAN_POINT ( 'NONE',  ( 8.986258411359999698, -35.50000000000000000, -19.49544327779999975 ) ) ;
#16455 = CARTESIAN_POINT ( 'NONE',  ( 16.20256441434644401, -100.6644468685070279, 4.326382415546095039 ) ) ;
#16456 = CARTESIAN_POINT ( 'NONE',  ( -3.669439427402429121, -72.55114739963670445, -28.40640588287540069 ) ) ;
#16457 = ORIENTED_EDGE ( 'NONE', *, *, #4606, .T. ) ;
#16458 = CONTEXT_DEPENDENT_SHAPE_REPRESENTATION ( #1429, #21300 ) ;
#16459 = EDGE_CURVE ( 'NONE', #9851, #1181, #7235, .T. ) ;
#16460 = AXIS2_PLACEMENT_3D ( 'NONE', #23050, #5677, #22904 ) ;
#16461 = DIRECTION ( 'NONE',  ( 1.000000000000000000, 0.000000000000000000, 0.000000000000000000 ) ) ;
#16462 = CARTESIAN_POINT ( 'NONE',  ( 9.334872109610000362E-16, -74.00000000000000000, -2.419703924680000090E-15 ) ) ;
#16463 = EDGE_LOOP ( 'NONE', ( #15004, #11106, #19036, #13516 ) ) ;
#16464 = CARTESIAN_POINT ( 'NONE',  ( -14.71190774867310047, -74.49999999999998579, 36.44656183965725660 ) ) ;
#16465 = CARTESIAN_POINT ( 'NONE',  ( 47.07637643990781129, -74.27648884675060970, -1.578698681290582106 ) ) ;
#16466 = ORIENTED_EDGE ( 'NONE', *, *, #7257, .T. ) ;
#16467 = CARTESIAN_POINT ( 'NONE',  ( -5.909348975229999468, -101.1659666750000071, 14.88340913230000062 ) ) ;
#16468 = ORIENTED_EDGE ( 'NONE', *, *, #22851, .F. ) ;
#16469 = CARTESIAN_POINT ( 'NONE',  ( -2.582553463740000055, -56.43963366239999857, -25.20892743809999814 ) ) ;
#16470 = DIRECTION ( 'NONE',  ( 0.000000000000000000, -1.000000000000000000, 0.000000000000000000 ) ) ;
#16471 = AXIS2_PLACEMENT_3D ( 'NONE', #21698, #22280, #6250 ) ;
#16472 = VECTOR ( 'NONE', #13158, 1000.000000000000000 ) ;
#16473 = CARTESIAN_POINT ( 'NONE',  ( 40.70731707320000226, -74.50000000000000000, 7.215414233289999757 ) ) ;
#16474 = DIRECTION ( 'NONE',  ( 1.000000000000000000, 0.000000000000000000, 0.000000000000000000 ) ) ;
#16475 = CARTESIAN_POINT ( 'NONE',  ( 4.500000000000000000, -11.00000000000000000, 50.00000000000000000 ) ) ;
#16476 = CARTESIAN_POINT ( 'NONE',  ( 7.286238495500000134, -101.2500498790000023, 13.33737010350000141 ) ) ;
#16477 = CARTESIAN_POINT ( 'NONE',  ( 46.81085661582252300, -79.82853832540322969, -3.128125291494992410 ) ) ;
#16478 = ORIENTED_EDGE ( 'NONE', *, *, #16680, .F. ) ;
#16479 = CARTESIAN_POINT ( 'NONE',  ( -32.70621743230000078, -79.83488737980000849, -22.19846261920000074 ) ) ;
#16480 = CARTESIAN_POINT ( 'NONE',  ( 19.91489110990000100, -97.53592492930000901, 2.489640473879999760 ) ) ;
#16481 = CARTESIAN_POINT ( 'NONE',  ( -20.43932690519999795, -94.59275946379999311, 12.18704468149999975 ) ) ;
#16482 = CARTESIAN_POINT ( 'NONE',  ( 24.01308102359999808, -93.00000902169999506, -18.61461954819999676 ) ) ;
#16483 = ORIENTED_EDGE ( 'NONE', *, *, #25330, .T. ) ;
#16484 = AXIS2_PLACEMENT_3D ( 'NONE', #9627, #20728, #787 ) ;
#16485 = DIRECTION ( 'NONE',  ( -0.7414456417930912480, 0.000000000000000000, -0.6710129359900827151 ) ) ;
#16486 = DIRECTION ( 'NONE',  ( 0.000000000000000000, 1.000000000000000000, 0.000000000000000000 ) ) ;
#16487 = ORIENTED_EDGE ( 'NONE', *, *, #6604, .F. ) ;
#16488 = FACE_OUTER_BOUND ( 'NONE', #11986, .T. ) ;
#16489 = CARTESIAN_POINT ( 'NONE',  ( 0.9512194931930000319, -99.70407914540000149, -17.16990763940000164 ) ) ;
#16490 = DIRECTION ( 'NONE',  ( 0.7414456417930908039, 0.000000000000000000, 0.6710129359900831592 ) ) ;
#16491 = CARTESIAN_POINT ( 'NONE',  ( -38.23614497916284449, -65.70026997502627353, 1.401764440867459660 ) ) ;
#16492 = APPLICATION_CONTEXT ( 'automotive_design' ) ;
#16493 = EDGE_CURVE ( 'NONE', #7301, #10820, #717, .T. ) ;
#16494 = CARTESIAN_POINT ( 'NONE',  ( 23.00257633000000013, -58.88644793239999586, -9.320358454550000005 ) ) ;
#16495 = EDGE_CURVE ( 'NONE', #13319, #20241, #264, .T. ) ;
#16496 = AXIS2_PLACEMENT_3D ( 'NONE', #19331, #19887, #1994 ) ;
#16497 = CARTESIAN_POINT ( 'NONE',  ( -38.08875739639999836, -74.50000000000000000, 9.476764215410000247 ) ) ;
#16498 = ADVANCED_FACE ( 'NONE', ( #24560 ), #2580, .F. ) ;
#16499 = ADVANCED_FACE ( 'NONE', ( #18454 ), #10865, .F. ) ;
#16500 = EDGE_LOOP ( 'NONE', ( #23188, #5490, #12455, #7986 ) ) ;
#16501 = FACE_OUTER_BOUND ( 'NONE', #19364, .T. ) ;
#16502 = CARTESIAN_POINT ( 'NONE',  ( 19.72252123670000401, -35.98036830730000446, -9.327645202300001159 ) ) ;
#16503 = CARTESIAN_POINT ( 'NONE',  ( 7.292753731799999528, -92.50000000000000000, -29.01615345709999971 ) ) ;
#16504 = VERTEX_POINT ( 'NONE', #11127 ) ;
#16505 = CARTESIAN_POINT ( 'NONE',  ( -3.807886452449999570, -80.00000000000000000, 46.75000000000000000 ) ) ;
#16506 = DIRECTION ( 'NONE',  ( 0.000000000000000000, 1.000000000000000000, 0.000000000000000000 ) ) ;
#16507 = CARTESIAN_POINT ( 'NONE',  ( -18.08359759629999886, -92.56168670950000887, -23.48371534130000171 ) ) ;
#16508 = CIRCLE ( 'NONE', #8110, 3.500000000000003109 ) ;
#16509 = CARTESIAN_POINT ( 'NONE',  ( 27.68682485439999752, -25.10000000000000142, 50.68039294919999804 ) ) ;
#16510 = DIRECTION ( 'NONE',  ( 0.000000000000000000, -1.000000000000000000, 0.000000000000000000 ) ) ;
#16511 = CARTESIAN_POINT ( 'NONE',  ( 7.252148862920000383, -101.2521831870000142, 13.35282088509999987 ) ) ;
#16512 = ORIENTED_EDGE ( 'NONE', *, *, #9543, .T. ) ;
#16513 = CARTESIAN_POINT ( 'NONE',  ( 25.57735248450000043, -26.54349610970000128, 46.81902967690000139 ) ) ;
#16514 = CARTESIAN_POINT ( 'NONE',  ( -29.77335029849999870, -92.50000460620000808, -0.5783696374510000071 ) ) ;
#16515 = CARTESIAN_POINT ( 'NONE',  ( 26.62370195360000125, -72.37489743489999228, 10.79038948700000056 ) ) ;
#16516 = CARTESIAN_POINT ( 'NONE',  ( 11.21565222179999921, -96.96081043319999537, -17.72906860990000411 ) ) ;
#16517 = ORIENTED_EDGE ( 'NONE', *, *, #47, .T. ) ;
#16518 = AXIS2_PLACEMENT_3D ( 'NONE', #11855, #20460, #15930 ) ;
#16519 = CARTESIAN_POINT ( 'NONE',  ( 20.20034866289999798, -19.47487085739999912, -8.528768463580000514 ) ) ;
#16520 = CARTESIAN_POINT ( 'NONE',  ( 11.97277113790000058, -101.5369810359999860, -10.61440544620000104 ) ) ;
#16521 = CARTESIAN_POINT ( 'NONE',  ( -25.34421590619999876, -10.95575221240000019, -46.39227603280000523 ) ) ;
#16522 = DIRECTION ( 'NONE',  ( 0.9704142011833033488, 0.000000000000000000, -0.2414462220490755373 ) ) ;
#16523 = CARTESIAN_POINT ( 'NONE',  ( -37.95930193997842395, -65.71630926063573952, 0.8827409024611270194 ) ) ;
#16524 = CARTESIAN_POINT ( 'NONE',  ( -40.00000000000000000, -66.00000000000000000, 0.000000000000000000 ) ) ;
#16525 = CARTESIAN_POINT ( 'NONE',  ( 22.71123055929999879, -49.06719615680000146, -9.238026508709999973 ) ) ;
#16526 = CARTESIAN_POINT ( 'NONE',  ( 13.77871658040979419, -98.12113978595867536, 15.06064669432830705 ) ) ;
#16527 = CARTESIAN_POINT ( 'NONE',  ( -16.97397862119999701, -99.68179698959998802, 2.927883187840000012 ) ) ;
#16528 = VERTEX_POINT ( 'NONE', #11428 ) ;
#16529 = EDGE_CURVE ( 'NONE', #19071, #20556, #19294, .T. ) ;
#16530 = CARTESIAN_POINT ( 'NONE',  ( -32.68577570540000465, -74.40224539360001188, -21.72078879429999887 ) ) ;
#16531 = CARTESIAN_POINT ( 'NONE',  ( 0.000000000000000000, -84.75000000000000000, 0.000000000000000000 ) ) ;
#16532 = AXIS2_PLACEMENT_3D ( 'NONE', #11869, #11718, #22970 ) ;
#16533 = EDGE_CURVE ( 'NONE', #2786, #20017, #5036, .T. ) ;
#16534 = CARTESIAN_POINT ( 'NONE',  ( -11.18841398930000075, -94.77531363049999413, -20.78536845970000257 ) ) ;
#16535 = CARTESIAN_POINT ( 'NONE',  ( 9.038647664420000893, -35.72724364799999819, -19.55068599180000177 ) ) ;
#16536 = CARTESIAN_POINT ( 'NONE',  ( 36.44456167670000468, -80.16838065170000505, -14.57571988100000127 ) ) ;
#16537 = AXIS2_PLACEMENT_3D ( 'NONE', #19309, #27543, #1828 ) ;
#16538 = B_SPLINE_CURVE_WITH_KNOTS ( 'NONE', 5,
 ( #2057, #26375, #15270, #12663, #22008, #10897 ),
 .UNSPECIFIED., .F., .F.,
 ( 6, 6 ),
 ( 0.000000000000000000, 1.000000000000000000 ),
 .UNSPECIFIED. ) ;
#16539 = CARTESIAN_POINT ( 'NONE',  ( 23.58466923419999972, -94.98812477769999418, -2.405350023570000051 ) ) ;
#16540 = CARTESIAN_POINT ( 'NONE',  ( -20.54445053870980686, -93.08694455160939185, -20.58885575223966669 ) ) ;
#16541 = DIRECTION ( 'NONE',  ( 0.000000000000000000, 1.000000000000000000, 0.000000000000000000 ) ) ;
#16542 = PRESENTATION_STYLE_ASSIGNMENT (( #23247 ) ) ;
#16543 = ORIENTED_EDGE ( 'NONE', *, *, #6726, .T. ) ;
#16544 = CARTESIAN_POINT ( 'NONE',  ( 32.97008024890000399, -74.00000000000000000, -20.36016474349999683 ) ) ;
#16545 = CARTESIAN_POINT ( 'NONE',  ( -12.19871226703897804, -59.03921358009454678, -19.98711032788098763 ) ) ;
#16546 = ORIENTED_EDGE ( 'NONE', *, *, #11503, .F. ) ;
#16547 = FACE_OUTER_BOUND ( 'NONE', #7990, .T. ) ;
#16548 = CARTESIAN_POINT ( 'NONE',  ( 0.5866164698262277266, -100.8738282930437720, -16.59383815637838566 ) ) ;
#16549 = CARTESIAN_POINT ( 'NONE',  ( -7.462548272780000325, -74.10728787440000076, 39.37382359230000617 ) ) ;
#16550 = CARTESIAN_POINT ( 'NONE',  ( -10.00000000000000000, -19.00000000000000000, 1.224606353819999829E-15 ) ) ;
#16551 = CARTESIAN_POINT ( 'NONE',  ( -12.45019672459999960, -94.16701134360000935, -21.10503017290000116 ) ) ;
#16552 = DIRECTION ( 'NONE',  ( 0.000000000000000000, 1.000000000000000000, 0.000000000000000000 ) ) ;
#16553 = CARTESIAN_POINT ( 'NONE',  ( 25.25824993130000351, -73.10684313109999266, -29.82725550210000165 ) ) ;
#16554 = DIRECTION ( 'NONE',  ( 0.000000000000000000, -1.000000000000000000, 0.000000000000000000 ) ) ;
#16555 = CARTESIAN_POINT ( 'NONE',  ( 23.85248605308397885, -92.80442066019703873, -19.00813913752200790 ) ) ;
#16556 = CARTESIAN_POINT ( 'NONE',  ( 0.000000000000000000, -18.50000000000000000, 0.000000000000000000 ) ) ;
#16557 = CARTESIAN_POINT ( 'NONE',  ( -2.756696846970000170, -109.2500000000000000, -5.046099730869999966 ) ) ;
#16558 = DIRECTION ( 'NONE',  ( 0.000000000000000000, -1.000000000000000000, 0.000000000000000000 ) ) ;
#16559 = SURFACE_STYLE_USAGE ( .BOTH. , #7695 ) ;
#16560 = ORIENTED_EDGE ( 'NONE', *, *, #6184, .F. ) ;
#16561 = EDGE_CURVE ( 'NONE', #27225, #13659, #17419, .T. ) ;
#16562 = CARTESIAN_POINT ( 'NONE',  ( -41.41155280139999917, -65.17124718639999514, 2.835686332019999867 ) ) ;
#16563 = ORIENTED_EDGE ( 'NONE', *, *, #4617, .T. ) ;
#16564 = EDGE_CURVE ( 'NONE', #3430, #18376, #28736, .T. ) ;
#16565 = CARTESIAN_POINT ( 'NONE',  ( -0.5421338679160000451, -57.91805294160000273, -23.37022173519999768 ) ) ;
#16566 = CARTESIAN_POINT ( 'NONE',  ( 10.42651188819999852, -36.18510625669999570, -22.68565687619999949 ) ) ;
#16567 = CARTESIAN_POINT ( 'NONE',  ( 0.000000000000000000, -10.00000000000000000, 0.000000000000000000 ) ) ;
#16568 = DIRECTION ( 'NONE',  ( 0.000000000000000000, 0.000000000000000000, 1.000000000000000000 ) ) ;
#16569 = ORIENTED_EDGE ( 'NONE', *, *, #20226, .T. ) ;
#16570 = ORIENTED_EDGE ( 'NONE', *, *, #18432, .F. ) ;
#16571 = CARTESIAN_POINT ( 'NONE',  ( -28.88915324434640652, -93.08996811601012666, 3.176849059424360355 ) ) ;
#16572 = FACE_OUTER_BOUND ( 'NONE', #26565, .T. ) ;
#16573 = ORIENTED_EDGE ( 'NONE', *, *, #5182, .T. ) ;
#16574 = CIRCLE ( 'NONE', #22147, 58.54999999999999716 ) ;
#16575 = DIRECTION ( 'NONE',  ( 1.000000000000000000, 0.000000000000000000, 0.000000000000000000 ) ) ;
#16576 = CARTESIAN_POINT ( 'NONE',  ( -11.23686253208929919, -59.05314867388291589, 20.60269805518056074 ) ) ;
#16577 = DIRECTION ( 'NONE',  ( 0.000000000000000000, -1.000000000000000000, 0.000000000000000000 ) ) ;
#16578 = CARTESIAN_POINT ( 'NONE',  ( 0.000000000000000000, -12.64149019679999952, 0.000000000000000000 ) ) ;
#16579 = CARTESIAN_POINT ( 'NONE',  ( -3.236746276329999894, -71.55793241529998738, -28.02041562209999981 ) ) ;
#16580 = CARTESIAN_POINT ( 'NONE',  ( 32.75000000000000000, -73.50000000000000000, -2.303043639999999983E-16 ) ) ;
#16581 = ORIENTED_EDGE ( 'NONE', *, *, #21870, .F. ) ;
#16582 = CARTESIAN_POINT ( 'NONE',  ( -14.42556421679999978, -93.00000000000000000, -2.978755036369999942 ) ) ;
#16583 = CARTESIAN_POINT ( 'NONE',  ( -14.88703466399999975, -101.2270092189999957, 3.209821742049999926 ) ) ;
#16584 = CARTESIAN_POINT ( 'NONE',  ( 26.46311779310000034, -64.24504203739999753, 1.532421101449999989 ) ) ;
#16585 = DIRECTION ( 'NONE',  ( 1.000000000000000000, 0.000000000000000000, 0.000000000000000000 ) ) ;
#16586 = ORIENTED_EDGE ( 'NONE', *, *, #20660, .T. ) ;
#16587 = B_SPLINE_CURVE_WITH_KNOTS ( 'NONE', 3,
 ( #2554, #25134, #2994, #7355, #4872, #376, #9664, #9220, #27315, #13753 ),
 .UNSPECIFIED., .F., .F.,
 ( 4, 2, 2, 2, 4 ),
 ( 0.000000000000000000, 0.2500000000000000000, 0.5000000000000000000, 0.7500000000000000000, 1.000000000000000000 ),
 .UNSPECIFIED. ) ;
#16588 = CARTESIAN_POINT ( 'NONE',  ( 0.000000000000000000, -102.8486084350000027, 0.000000000000000000 ) ) ;
#16589 = CARTESIAN_POINT ( 'NONE',  ( -3.651945809410000354, -18.50000000000000000, -23.59378895079999694 ) ) ;
#16590 = CARTESIAN_POINT ( 'NONE',  ( -7.905721070053497002, -100.3617719037266767, 15.06330732917539095 ) ) ;
#16591 = ORIENTED_EDGE ( 'NONE', *, *, #3790, .F. ) ;
#16592 = EDGE_CURVE ( 'NONE', #10781, #8949, #5138, .T. ) ;
#16593 = EDGE_CURVE ( 'NONE', #28180, #2258, #26751, .T. ) ;
#16594 = DIRECTION ( 'NONE',  ( 0.000000000000000000, -1.000000000000000000, 0.000000000000000000 ) ) ;
#16595 = CARTESIAN_POINT ( 'NONE',  ( -41.79353403746807061, -65.72247384671341308, -1.295796974283231151 ) ) ;
#16596 = CARTESIAN_POINT ( 'NONE',  ( 36.59060436630000623, -79.19020236199999374, -14.75000000000000000 ) ) ;
#16597 = DIRECTION ( 'NONE',  ( 0.000000000000000000, 1.000000000000000000, 0.000000000000000000 ) ) ;
#16598 = ORIENTED_EDGE ( 'NONE', *, *, #456, .F. ) ;
#16599 = CARTESIAN_POINT ( 'NONE',  ( -12.15229178470000093, -18.85738388180000058, 18.91927663179999897 ) ) ;
#16600 = CARTESIAN_POINT ( 'NONE',  ( -0.8893110448141080537, -79.83729532519589611, 47.19525132417524560 ) ) ;
#16601 = EDGE_LOOP ( 'NONE', ( #1210, #20187 ) ) ;
#16602 = CARTESIAN_POINT ( 'NONE',  ( -14.61042918459367357, -74.50000000000000000, 36.68561768139541357 ) ) ;
#16603 = CARTESIAN_POINT ( 'NONE',  ( 47.25000000000000000, -75.00000000000000000, -1.242228542250000064E-12 ) ) ;
#16604 = ORIENTED_EDGE ( 'NONE', *, *, #5068, .T. ) ;
#16605 = CARTESIAN_POINT ( 'NONE',  ( -13.34665425529999894, -19.40595393460000295, 20.06920644170000045 ) ) ;
#16606 = ORIENTED_EDGE ( 'NONE', *, *, #993, .T. ) ;
#16607 = CARTESIAN_POINT ( 'NONE',  ( -37.47207447326633201, -63.24690319806014571, -0.5612274588096003436 ) ) ;
#16608 = DIRECTION ( 'NONE',  ( 1.000000000000000000, 0.000000000000000000, 0.000000000000000000 ) ) ;
#16609 = ADVANCED_FACE ( 'NONE', ( #17395 ), #23038, .F. ) ;
#16610 = CARTESIAN_POINT ( 'NONE',  ( 39.92825895559999339, -74.14144493690000104, 7.283540599280000194 ) ) ;
#16611 = DIRECTION ( 'NONE',  ( 0.000000000000000000, 1.000000000000000000, 0.000000000000000000 ) ) ;
#16612 = CARTESIAN_POINT ( 'NONE',  ( -11.62982413452877317, -61.04161776321530652, -22.93818510518001830 ) ) ;
#16613 = DIRECTION ( 'NONE',  ( 1.000000000000000000, 0.000000000000000000, 0.000000000000000000 ) ) ;
#16614 = ORIENTED_EDGE ( 'NONE', *, *, #217, .T. ) ;
#16615 = CARTESIAN_POINT ( 'NONE',  ( -32.54924051920000494, -80.01920155719999173, -22.21939872999999821 ) ) ;
#16616 = CARTESIAN_POINT ( 'NONE',  ( 10.49047210377122497, -92.65509297689168022, -25.64082608166361155 ) ) ;
#16617 = CARTESIAN_POINT ( 'NONE',  ( -20.45316973280000283, -93.85308800720000022, 14.21304034189999932 ) ) ;
#16618 = CARTESIAN_POINT ( 'NONE',  ( 0.000000000000000000, -108.5000000000000000, 0.000000000000000000 ) ) ;
#16619 = VERTEX_POINT ( 'NONE', #10659 ) ;
#16620 = CARTESIAN_POINT ( 'NONE',  ( -2.271147603640000234, -79.96785398299999770, 47.05359239509999725 ) ) ;
#16621 = CARTESIAN_POINT ( 'NONE',  ( -12.76533973971643476, -68.20220985960887106, -23.31270125210677335 ) ) ;
#16622 = ORIENTED_EDGE ( 'NONE', *, *, #21838, .T. ) ;
#16623 = DIRECTION ( 'NONE',  ( 0.000000000000000000, 1.000000000000000000, 0.000000000000000000 ) ) ;
#16624 = B_SPLINE_CURVE_WITH_KNOTS ( 'NONE', 3,
 ( #9883, #23166, #14271, #897 ),
 .UNSPECIFIED., .F., .F.,
 ( 4, 4 ),
 ( 0.000000000000000000, 1.000000000000000000 ),
 .UNSPECIFIED. ) ;
#16625 = DIRECTION ( 'NONE',  ( 0.000000000000000000, -1.000000000000000000, 0.000000000000000000 ) ) ;
#16626 = LINE ( 'NONE', #5420, #19350 ) ;
#16627 = CARTESIAN_POINT ( 'NONE',  ( 31.27011777710000118, -74.10309036889998424, -23.59316291639999719 ) ) ;
#16628 = CARTESIAN_POINT ( 'NONE',  ( -16.85275212698199709, -72.18744872196315043, 23.44936106519583774 ) ) ;
#16629 = CIRCLE ( 'NONE', #11004, 8.000000000000000000 ) ;
#16630 = CARTESIAN_POINT ( 'NONE',  ( 25.42047192209999906, -65.65894985479999946, 0.2065551165869999872 ) ) ;
#16631 = CARTESIAN_POINT ( 'NONE',  ( -10.85837829980000002, -19.46429346509999903, 19.17438121190000189 ) ) ;
#16632 = EDGE_LOOP ( 'NONE', ( #4388, #11208, #6117, #28788 ) ) ;
#16633 = CARTESIAN_POINT ( 'NONE',  ( 20.37615251160000085, -53.60206220650000120, 11.14673842929999914 ) ) ;
#16634 = CARTESIAN_POINT ( 'NONE',  ( -41.00000000000000000, -84.50000000000000000, -10.20110288159999890 ) ) ;
#16635 = TOROIDAL_SURFACE ( 'NONE', #4519, 16.50000000000000000, 5.500000000000000000 ) ;
#16636 = CARTESIAN_POINT ( 'NONE',  ( 20.21146652389999687, -35.98398933269999844, -9.285965084309999895 ) ) ;
#16637 = LINE ( 'NONE', #25817, #15824 ) ;
#16638 = EDGE_LOOP ( 'NONE', ( #24081, #2069, #1230, #11769 ) ) ;
#16639 = DIRECTION ( 'NONE',  ( 1.000000000000000000, 0.000000000000000000, 0.000000000000000000 ) ) ;
#16640 = B_SPLINE_SURFACE_WITH_KNOTS ( 'NONE', 5, 5, ( 
 ( #6835, #24760, #2621, #15146, #24054, #4493 ),
 ( #13368, #15699, #13673, #9002, #2474, #26106 ),
 ( #19538, #24605, #4796, #22272, #22578, #28281 ),
 ( #17910, #6132, #444, #2320, #15999, #21591 ),
 ( #13519, #11470, #20086, #22428, #11328, #15005 ),
 ( #28426, #20375, #9294, #18196, #20233, #27091 ) ),
 .UNSPECIFIED., .F., .F., .F.,
 ( 6, 6 ),
 ( 6, 6 ),
 ( 2.788355763089999773, 6.107000906349999703 ),
 ( 0.000000000000000000, 0.5000000000000000000 ),
 .UNSPECIFIED. ) ;
#16641 = ADVANCED_FACE ( 'NONE', ( #13001 ), #27345, .T. ) ;
#16642 = CARTESIAN_POINT ( 'NONE',  ( 0.000000000000000000, -92.50000000000000000, 0.000000000000000000 ) ) ;
#16643 = CARTESIAN_POINT ( 'NONE',  ( -17.93028678539999987, -18.50000000000000000, 10.99759328500000066 ) ) ;
#16644 = CARTESIAN_POINT ( 'NONE',  ( 9.357772773659998933, -44.87455296190000098, -22.87094945020000125 ) ) ;
#16645 = DIRECTION ( 'NONE',  ( 1.000000000000000000, 0.000000000000000000, 1.224606353820001308E-16 ) ) ;
#16646 = ORIENTED_EDGE ( 'NONE', *, *, #2860, .T. ) ;
#16647 = ADVANCED_FACE ( 'NONE', ( #22349 ), #73, .F. ) ;
#16648 = CARTESIAN_POINT ( 'NONE',  ( -39.39373284327518832, -73.64797963447830398, 7.224658177534047709 ) ) ;
#16649 = CARTESIAN_POINT ( 'NONE',  ( -28.39500908420000158, -92.99999854809999533, -2.401901190519999840 ) ) ;
#16650 = CARTESIAN_POINT ( 'NONE',  ( 10.69569866790000034, -95.98460637910000059, -20.33107714349999995 ) ) ;
#16651 = ORIENTED_EDGE ( 'NONE', *, *, #5538, .T. ) ;
#16652 = CARTESIAN_POINT ( 'NONE',  ( 19.17432176879999872, -18.50000000000000000, -8.311993326940001481 ) ) ;
#16653 = EDGE_CURVE ( 'NONE', #27454, #22316, #22792, .T. ) ;
#16654 = CYLINDRICAL_SURFACE ( 'NONE', #27000, 0.9999999999999990008 ) ;
#16655 = CARTESIAN_POINT ( 'NONE',  ( -2.557496217909999814, -32.68478243010000028, -23.95624216479999902 ) ) ;
#16656 = DIRECTION ( 'NONE',  ( 1.000000000000000000, 0.000000000000000000, 0.000000000000000000 ) ) ;
#16657 = EDGE_CURVE ( 'NONE', #25992, #7997, #9211, .T. ) ;
#16658 = CARTESIAN_POINT ( 'NONE',  ( -38.71641004229999794, -73.50000000000000000, 7.135467526410000261 ) ) ;
#16659 = AXIS2_PLACEMENT_3D ( 'NONE', #21699, #19508, #20095 ) ;
#16660 = CARTESIAN_POINT ( 'NONE',  ( 26.60903970598167589, -26.59999999999999787, 48.70752046822583736 ) ) ;
#16661 = CARTESIAN_POINT ( 'NONE',  ( -38.62788938250000115, -74.00000000000000000, -7.627566167509999495 ) ) ;
#16662 = CARTESIAN_POINT ( 'NONE',  ( -10.69289422250000143, -27.02040600870000020, -21.42405574569999871 ) ) ;
#16663 = ORIENTED_EDGE ( 'NONE', *, *, #7469, .F. ) ;
#16664 = CARTESIAN_POINT ( 'NONE',  ( 6.963769279919999278, -101.5216621940000152, 14.41672748959999950 ) ) ;
#16665 = DIRECTION ( 'NONE',  ( 1.000000000000000000, 0.000000000000000000, 0.000000000000000000 ) ) ;
#16666 = CARTESIAN_POINT ( 'NONE',  ( 7.358959778060000012, -101.1389411659999951, 13.51882459459999986 ) ) ;
#16667 = AXIS2_PLACEMENT_3D ( 'NONE', #22275, #24461, #26950 ) ;
#16668 = CARTESIAN_POINT ( 'NONE',  ( -11.56445414979999953, -94.58710607640000489, -20.95866303660000085 ) ) ;
#16669 = CARTESIAN_POINT ( 'NONE',  ( -40.50000000000000000, -65.63577453799999262, -2.309401076760000393 ) ) ;
#16670 = CARTESIAN_POINT ( 'NONE',  ( 7.218875474177777640, -73.62261561668250920, 39.32889484839974870 ) ) ;
#16671 = CARTESIAN_POINT ( 'NONE',  ( 23.95218086839091498, -94.65677004896707558, -2.989273988903572210 ) ) ;
#16672 = CARTESIAN_POINT ( 'NONE',  ( 40.00000000000000000, -69.00000000000000000, 3.566319567039999839E-15 ) ) ;
#16673 = DIRECTION ( 'NONE',  ( 0.000000000000000000, 1.000000000000000000, 0.000000000000000000 ) ) ;
#16674 = EDGE_LOOP ( 'NONE', ( #17595, #13729, #15683, #2564, #7486, #4863, #27409, #24264, #11141, #18476, #14262, #28383, #2830, #2913, #7117, #27635, #28311, #11353, #20992, #14468, #9654, #2274, #26118, #22600, #15271, #14239, #27975, #17084, #18323, #5583, #18940, #4976, #27014, #25108, #3377, #10926, #4408 ) ) ;
#16675 = CARTESIAN_POINT ( 'NONE',  ( 30.67829226190271186, -74.17388968317500542, -24.28831386657427416 ) ) ;
#16676 = CARTESIAN_POINT ( 'NONE',  ( 12.01505635090000190, -101.1292389600000092, -9.802278386409998490 ) ) ;
#16677 = CARTESIAN_POINT ( 'NONE',  ( -28.19022166989999789, -39.75000000000000000, -51.60185463919999194 ) ) ;
#16678 = ORIENTED_EDGE ( 'NONE', *, *, #6094, .F. ) ;
#16679 = FACE_OUTER_BOUND ( 'NONE', #12519, .T. ) ;
#16680 = EDGE_CURVE ( 'NONE', #18617, #8439, #17900, .T. ) ;
#16681 = CARTESIAN_POINT ( 'NONE',  ( 0.4132369963184429618, -99.96200787827957868, -17.32932737678238055 ) ) ;
#16682 = CARTESIAN_POINT ( 'NONE',  ( -7.378478634080000376, -74.05312334699999610, 39.40347957289999670 ) ) ;
#16683 = DIRECTION ( 'NONE',  ( -0.4047940155640055160, 0.000000000000000000, 0.9144078985680119676 ) ) ;
#16684 = CARTESIAN_POINT ( 'NONE',  ( -14.04223022189999881, -93.60790942709999740, -21.24517368629999936 ) ) ;
#16685 = ADVANCED_FACE ( 'NONE', ( #27016 ), #9155, .T. ) ;
#16686 = CARTESIAN_POINT ( 'NONE',  ( 20.35087214540000033, -74.00000000000000000, -32.65606037229999714 ) ) ;
#16687 = EDGE_CURVE ( 'NONE', #16053, #10781, #12294, .T. ) ;
#16688 = CIRCLE ( 'NONE', #1796, 13.13304743849999845 ) ;
#16689 = CARTESIAN_POINT ( 'NONE',  ( -38.25000000000000000, -65.63577453799999262, -1.587713240270000048 ) ) ;
#16690 = CARTESIAN_POINT ( 'NONE',  ( -13.76821744699999961, -50.22312506960000178, 21.09213694800000027 ) ) ;
#16691 = CARTESIAN_POINT ( 'NONE',  ( 26.66586753799999698, -92.50000000000000000, 13.56661073689999952 ) ) ;
#16692 = CARTESIAN_POINT ( 'NONE',  ( 7.734541327699999691, -19.43020093410000015, -20.63024918810000230 ) ) ;
#16693 = CARTESIAN_POINT ( 'NONE',  ( -17.79218750000000071, -74.00000000000000000, 44.84975545040000355 ) ) ;
#16694 = DIRECTION ( 'NONE',  ( 0.4794255386042036715, 0.000000000000000000, 0.8775825618903724257 ) ) ;
#16695 = VERTEX_POINT ( 'NONE', #11249 ) ;
#16696 = CARTESIAN_POINT ( 'NONE',  ( 10.20110288159999890, -74.50000000000000000, 41.00000000000000000 ) ) ;
#16697 = B_SPLINE_CURVE_WITH_KNOTS ( 'NONE', 3,
 ( #16661, #18723, #25556, #27620, #14338, #20619, #27471, #18575 ),
 .UNSPECIFIED., .F., .F.,
 ( 4, 2, 2, 4 ),
 ( 0.000000000000000000, 0.2499999999999987788, 0.4999999999999975575, 1.000000000000000000 ),
 .UNSPECIFIED. ) ;
#16698 = ORIENTED_EDGE ( 'NONE', *, *, #19034, .F. ) ;
#16699 = B_SPLINE_CURVE_WITH_KNOTS ( 'NONE', 5,
 ( #6027, #19165, #1684, #8220, #23263, #12170, #7818, #9982, #27915 ),
 .UNSPECIFIED., .F., .F.,
 ( 6, 3, 6 ),
 ( 0.000000000000000000, 0.5000000000000000000, 1.000000000000000000 ),
 .UNSPECIFIED. ) ;
#16700 = DIRECTION ( 'NONE',  ( 0.000000000000000000, 1.000000000000000000, 0.000000000000000000 ) ) ;
#16701 = CIRCLE ( 'NONE', #15753, 0.5000000000000004441 ) ;
#16702 = CARTESIAN_POINT ( 'NONE',  ( 10.59598273719999995, -36.06131723410000234, -22.18468985750000044 ) ) ;
#16703 = CYLINDRICAL_SURFACE ( 'NONE', #9757, 0.7999999999999994893 ) ;
#16704 = CARTESIAN_POINT ( 'NONE',  ( 37.60355029590000697, -84.00000000000000000, 9.356041104380000917 ) ) ;
#16705 = AXIS2_PLACEMENT_3D ( 'NONE', #5890, #21767, #14904 ) ;
#16706 = AXIS2_PLACEMENT_3D ( 'NONE', #15817, #2003, #10844 ) ;
#16707 = VECTOR ( 'NONE', #10762, 1000.000000000000000 ) ;
#16708 = CARTESIAN_POINT ( 'NONE',  ( -20.03576987106655238, -32.72519964002148640, 14.54909399142346160 ) ) ;
#16709 = VECTOR ( 'NONE', #20792, 1000.000000000000000 ) ;
#16710 = ORIENTED_EDGE ( 'NONE', *, *, #13652, .T. ) ;
#16711 = LINE ( 'NONE', #18478, #11115 ) ;
#16712 = EDGE_CURVE ( 'NONE', #22101, #21750, #2544, .T. ) ;
#16713 = CARTESIAN_POINT ( 'NONE',  ( 0.000000000000000000, -108.5000000000000000, 0.000000000000000000 ) ) ;
#16714 = EDGE_LOOP ( 'NONE', ( #12569, #2720, #21855, #5571 ) ) ;
#16715 = LINE ( 'NONE', #21655, #6111 ) ;
#16716 = CARTESIAN_POINT ( 'NONE',  ( 9.046504331389998654, -35.76492331110000578, -19.84904996739999916 ) ) ;
#16717 = EDGE_CURVE ( 'NONE', #8180, #7391, #17882, .T. ) ;
#16718 = CARTESIAN_POINT ( 'NONE',  ( 27.23270669000000055, -92.50000467790000869, -12.38956474639999961 ) ) ;
#16719 = EDGE_CURVE ( 'NONE', #12333, #26756, #14464, .T. ) ;
#16720 = CARTESIAN_POINT ( 'NONE',  ( -22.05955109964234495, -74.01432994044633062, -32.14328720598611255 ) ) ;
#16721 = ORIENTED_EDGE ( 'NONE', *, *, #2664, .F. ) ;
#16722 = EDGE_CURVE ( 'NONE', #12729, #5957, #20224, .T. ) ;
#16723 = CARTESIAN_POINT ( 'NONE',  ( -14.68103708169999955, -101.1848540220000103, 4.247747895729999890 ) ) ;
#16724 = CARTESIAN_POINT ( 'NONE',  ( -16.65233384409999928, -100.4382163219999882, 3.162646594119999932 ) ) ;
#16725 = CARTESIAN_POINT ( 'NONE',  ( 24.03655833510000051, -62.10499660389999832, 0.01904210411250000304 ) ) ;
#16726 = CARTESIAN_POINT ( 'NONE',  ( -19.90875640260000168, -60.57913428290000013, 12.83012088510000126 ) ) ;
#16727 = VERTEX_POINT ( 'NONE', #9516 ) ;
#16728 = AXIS2_PLACEMENT_3D ( 'NONE', #2291, #120, #16412 ) ;
#16729 = CARTESIAN_POINT ( 'NONE',  ( 19.66608320708412805, -98.68740020691039661, -0.5966002485424611868 ) ) ;
#16730 = CARTESIAN_POINT ( 'NONE',  ( -3.351256578809999720, -18.50000000000000000, -24.02084876199999997 ) ) ;
#16731 = CARTESIAN_POINT ( 'NONE',  ( 36.75634433000346490, -74.48625131260783405, -14.60844170371495210 ) ) ;
#16732 = ORIENTED_EDGE ( 'NONE', *, *, #1278, .F. ) ;
#16733 = CIRCLE ( 'NONE', #25583, 6.000000000000000000 ) ;
#16734 = AXIS2_PLACEMENT_3D ( 'NONE', #28146, #8181, #17067 ) ;
#16735 = CARTESIAN_POINT ( 'NONE',  ( -14.62247892739999955, -91.50000000000000000, -26.76626813769999913 ) ) ;
#16736 = CARTESIAN_POINT ( 'NONE',  ( 36.69050691090000527, -80.32091633570000511, -13.94376034409999932 ) ) ;
#16737 = CARTESIAN_POINT ( 'NONE',  ( 36.72991148340000223, -74.73026516779999895, -14.71529450729999944 ) ) ;
#16738 = ORIENTED_EDGE ( 'NONE', *, *, #19619, .T. ) ;
#16739 = UNCERTAINTY_MEASURE_WITH_UNIT (LENGTH_MEASURE( 1.000000000000000082E-05 ), #7496, 'distance_accuracy_value', 'NONE');
#16740 = CARTESIAN_POINT ( 'NONE',  ( 6.838213422042789702, -100.3796496173189894, 15.56132088991555129 ) ) ;
#16741 = CARTESIAN_POINT ( 'NONE',  ( -0.8115734779096079876, -79.80847618003535615, 47.20451980215236887 ) ) ;
#16742 = EDGE_LOOP ( 'NONE', ( #18738, #27580, #23046, #21002 ) ) ;
#16743 = CARTESIAN_POINT ( 'NONE',  ( 46.75000000000000000, -69.00000000000000000, 4.603792064249999600E-16 ) ) ;
#16744 = ORIENTED_EDGE ( 'NONE', *, *, #17606, .T. ) ;
#16745 = CARTESIAN_POINT ( 'NONE',  ( 28.56683165460000140, -92.91851489520000484, 8.527576185230000050 ) ) ;
#16746 = CARTESIAN_POINT ( 'NONE',  ( -6.249265825439999311, -101.3256027139999986, 14.62769162600000072 ) ) ;
#16747 = ORIENTED_EDGE ( 'NONE', *, *, #8059, .T. ) ;
#16748 = FACE_OUTER_BOUND ( 'NONE', #4773, .T. ) ;
#16749 = DIRECTION ( 'NONE',  ( 0.4794255386042041156, 0.000000000000000000, 0.8775825618903722036 ) ) ;
#16750 = AXIS2_PLACEMENT_3D ( 'NONE', #14684, #12216, #3759 ) ;
#16751 = EDGE_CURVE ( 'NONE', #19773, #11126, #16795, .T. ) ;
#16752 = ORIENTED_EDGE ( 'NONE', *, *, #18745, .F. ) ;
#16753 = CARTESIAN_POINT ( 'NONE',  ( -41.75516512379999767, -65.84529946160000691, -0.9588510772079998912 ) ) ;
#16754 = CARTESIAN_POINT ( 'NONE',  ( 16.77269055116476792, -99.57060688044040830, 4.505412732972978951 ) ) ;
#16755 = CARTESIAN_POINT ( 'NONE',  ( 46.91594090715152277, -79.74893011108233054, -2.749115903323809729 ) ) ;
#16756 = ORIENTED_EDGE ( 'NONE', *, *, #397, .T. ) ;
#16757 = CARTESIAN_POINT ( 'NONE',  ( -16.98465565300000080, -97.93128678269999909, -10.56456529129999922 ) ) ;
#16758 = DIRECTION ( 'NONE',  ( 1.000000000000000000, 0.000000000000000000, 0.000000000000000000 ) ) ;
#16759 = DIRECTION ( 'NONE',  ( 0.000000000000000000, -1.000000000000000000, 0.000000000000000000 ) ) ;
#16760 = DIRECTION ( 'NONE',  ( 1.095614826932720052E-15, 0.000000000000000000, -1.000000000000000000 ) ) ;
#16761 = FACE_OUTER_BOUND ( 'NONE', #6137, .T. ) ;
#16762 = B_SPLINE_CURVE_WITH_KNOTS ( 'NONE', 5,
 ( #14430, #23321, #5947, #1886, #10723, #12496, #6380, #12637, #1736 ),
 .UNSPECIFIED., .F., .F.,
 ( 6, 3, 6 ),
 ( 0.000000000000000000, 0.5240999523975469199, 1.000000000000000000 ),
 .UNSPECIFIED. ) ;
#16763 = CARTESIAN_POINT ( 'NONE',  ( -0.7692311531319999673, -79.63780243000000780, 47.25012955910000301 ) ) ;
#16764 = DIRECTION ( 'NONE',  ( 0.000000000000000000, -1.000000000000000000, 0.000000000000000000 ) ) ;
#16765 = EDGE_LOOP ( 'NONE', ( #10913, #2105 ) ) ;
#16766 = CARTESIAN_POINT ( 'NONE',  ( -30.31271238969999970, -93.00000000000000000, 0.1252161350790000072 ) ) ;
#16767 = DIRECTION ( 'NONE',  ( 0.4794255386042036715, 0.000000000000000000, 0.8775825618903724257 ) ) ;
#16768 = DIRECTION ( 'NONE',  ( -0.4151946956541399669, 0.5000000000001689759, -0.7600087925152558821 ) ) ;
#16769 = DIRECTION ( 'NONE',  ( 0.9397523434780248319, 0.000000000000000000, 0.3418560119810096221 ) ) ;
#16770 = DIRECTION ( 'NONE',  ( 0.000000000000000000, 1.000000000000000000, 0.000000000000000000 ) ) ;
#16771 = AXIS2_PLACEMENT_3D ( 'NONE', #265, #9107, #18008 ) ;
#16772 = CARTESIAN_POINT ( 'NONE',  ( 27.59093974670000193, -39.32601556110000018, 50.50487643680000360 ) ) ;
#16773 = AXIS2_PLACEMENT_3D ( 'NONE', #27997, #3801, #8035 ) ;
#16774 = EDGE_CURVE ( 'NONE', #10217, #25894, #9236, .T. ) ;
#16775 = CARTESIAN_POINT ( 'NONE',  ( -6.705637591229999472, -74.00000000000000000, 33.51864961869999604 ) ) ;
#16776 = ORIENTED_EDGE ( 'NONE', *, *, #7944, .T. ) ;
#16777 = CARTESIAN_POINT ( 'NONE',  ( -40.28633210810852461, -74.17816432860024634, -7.244343739419030648 ) ) ;
#16778 = B_SPLINE_CURVE_WITH_KNOTS ( 'NONE', 5,
 ( #27789, #870, #20957, #16708, #13798, #22703 ),
 .UNSPECIFIED., .F., .F.,
 ( 6, 6 ),
 ( 0.000000000000000000, 1.000000000000000000 ),
 .UNSPECIFIED. ) ;
#16779 = CARTESIAN_POINT ( 'NONE',  ( 21.75765532779999845, -37.94971352660000008, -8.412785021810000430 ) ) ;
#16780 = CARTESIAN_POINT ( 'NONE',  ( 12.82422237299999956, -94.98812477769999418, -19.93894812050000098 ) ) ;
#16781 = ORIENTED_EDGE ( 'NONE', *, *, #11152, .T. ) ;
#16782 = CARTESIAN_POINT ( 'NONE',  ( -13.14541460800000117, -101.3350617309999961, -9.160026903060000336 ) ) ;
#16783 = CARTESIAN_POINT ( 'NONE',  ( -29.21843812340000213, -93.00000000000000000, 6.434616699369999360 ) ) ;
#16784 = ADVANCED_FACE ( 'NONE', ( #22943 ), #2568, .F. ) ;
#16785 = CARTESIAN_POINT ( 'NONE',  ( 0.000000000000000000, 0.000000000000000000, 0.000000000000000000 ) ) ;
#16786 = CARTESIAN_POINT ( 'NONE',  ( -7.930433002940000975, -100.4731125450000064, 14.12856493100000144 ) ) ;
#16787 = EDGE_LOOP ( 'NONE', ( #19346, #7092 ) ) ;
#16788 = CARTESIAN_POINT ( 'NONE',  ( 1.869767860340000087, -92.87437365140000622, 27.35099196270000022 ) ) ;
#16789 = DIRECTION ( 'NONE',  ( 0.7071067811865475727, 0.000000000000000000, 0.7071067811865475727 ) ) ;
#16790 = CARTESIAN_POINT ( 'NONE',  ( -13.55269044519999966, -101.1889999979999999, -9.843123574170000722 ) ) ;
#16791 = AXIS2_PLACEMENT_3D ( 'NONE', #10071, #14192, #7506 ) ;
#16792 = CARTESIAN_POINT ( 'NONE',  ( 7.383226538699999786, -101.1286588279999989, 13.63651901270000089 ) ) ;
#16793 = ORIENTED_EDGE ( 'NONE', *, *, #19984, .F. ) ;
#16794 = VECTOR ( 'NONE', #22706, 1000.000000000000000 ) ;
#16795 = LINE ( 'NONE', #16513, #11373 ) ;
#16796 = AXIS2_PLACEMENT_3D ( 'NONE', #19344, #8253, #6220 ) ;
#16797 = CARTESIAN_POINT ( 'NONE',  ( -22.24124310690000073, -94.63960343439998724, -8.291373264160000645 ) ) ;
#16798 = CARTESIAN_POINT ( 'NONE',  ( 23.08916810359999872, -41.88175146140000038, -9.424942062580001334 ) ) ;
#16799 = ORIENTED_EDGE ( 'NONE', *, *, #11843, .F. ) ;
#16800 = LINE ( 'NONE', #18988, #16452 ) ;
#16801 = CARTESIAN_POINT ( 'NONE',  ( 11.29156748259999965, -101.1516803200000112, -10.36374020140000063 ) ) ;
#16802 = CARTESIAN_POINT ( 'NONE',  ( -14.16028365999999927, -74.03779068149999887, 36.32206337349999359 ) ) ;
#16803 = CARTESIAN_POINT ( 'NONE',  ( -17.48893075979999878, -94.09609773500001495, 17.08751209079999711 ) ) ;
#16804 = CARTESIAN_POINT ( 'NONE',  ( -18.08183833912162441, -92.54893169919637330, 24.56210854116960718 ) ) ;
#16805 = CARTESIAN_POINT ( 'NONE',  ( -1.328852201560088764, -74.17182873519007558, 47.12723346842092553 ) ) ;
#16806 = CARTESIAN_POINT ( 'NONE',  ( -0.03272619456850000413, -101.4121386959999995, -15.97721227889999795 ) ) ;
#16807 = DIRECTION ( 'NONE',  ( 0.000000000000000000, 1.000000000000000000, 0.000000000000000000 ) ) ;
#16808 = CARTESIAN_POINT ( 'NONE',  ( 7.010390260919999428E-15, -79.00000000000000000, 36.25000000000000000 ) ) ;
#16809 = CARTESIAN_POINT ( 'NONE',  ( 20.57008619019999784, -58.79569603810000444, 11.24574726549999859 ) ) ;
#16810 = EDGE_LOOP ( 'NONE', ( #14930, #8539, #19481, #6160, #26800, #17291, #26760, #19171 ) ) ;
#16811 = EDGE_CURVE ( 'NONE', #23252, #17023, #14803, .T. ) ;
#16812 = CARTESIAN_POINT ( 'NONE',  ( 6.324210420500000929, -100.7833805400000102, 14.60206476039999934 ) ) ;
#16813 = CARTESIAN_POINT ( 'NONE',  ( 47.17407167555492720, -74.61367352086737981, -1.124626421616047534 ) ) ;
#16814 = AXIS2_PLACEMENT_3D ( 'NONE', #1369, #14199, #5587 ) ;
#16815 = VECTOR ( 'NONE', #2861, 1000.000000000000000 ) ;
#16816 = CIRCLE ( 'NONE', #20049, 4.999999999999999112 ) ;
#16817 = CARTESIAN_POINT ( 'NONE',  ( -11.55953761080000142, -94.64048054399999899, -21.16633973740000130 ) ) ;
#16818 = DIRECTION ( 'NONE',  ( 0.000000000000000000, 1.000000000000000000, 0.000000000000000000 ) ) ;
#16819 = DIRECTION ( 'NONE',  ( 1.000000000000000000, 0.000000000000000000, 0.000000000000000000 ) ) ;
#16820 = B_SPLINE_CURVE_WITH_KNOTS ( 'NONE', 3,
 ( #2798, #15885, #13554, #11652, #7167, #24938, #7018, #22462, #20412, #15731, #2505, #20117, #24644, #8880, #4831, #16033, #11360, #22755, #483, #9326, #4524, #20263, #4673 ),
 .UNSPECIFIED., .F., .F.,
 ( 4, 2, 2, 1, 1, 2, 2, 2, 1, 1, 1, 2, 2, 4 ),
 ( 0.000000000000000000, 0.1249999999999429623, 0.1874999999999153177, 0.2187499999999028555, 0.2343749999998963329, 0.2421874999998903932, 0.2499999999998844813, 0.3749999999998625544, 0.4374999999998507860, 0.4687499999998409606, 0.4843749999998399614, 0.4921874999998397948, 0.4999999999998395728, 1.000000000000000000 ),
 .UNSPECIFIED. ) ;
#16821 = EDGE_CURVE ( 'NONE', #4122, #10810, #20733, .T. ) ;
#16822 = DIRECTION ( 'NONE',  ( 0.000000000000000000, 1.000000000000000000, 0.000000000000000000 ) ) ;
#16823 = DIRECTION ( 'NONE',  ( 0.000000000000000000, 1.000000000000000000, 0.000000000000000000 ) ) ;
#16824 = B_SPLINE_CURVE_WITH_KNOTS ( 'NONE', 5,
 ( #13281, #20285, #10932, #9056, #9198, #13427, #22632, #11068, #506 ),
 .UNSPECIFIED., .F., .F.,
 ( 6, 3, 6 ),
 ( 0.000000000000000000, 1.237573681340000009, 1.566718891480000098 ),
 .UNSPECIFIED. ) ;
#16825 = B_SPLINE_SURFACE_WITH_KNOTS ( 'NONE', 5, 5, ( 
 ( #13782, #4609, #410, #24425, #9261, #2438 ),
 ( #22683, #8966, #11292, #20491, #562, #28777 ),
 ( #4463, #13331, #22238, #11133, #14080, #7815 ),
 ( #16255, #998, #3032, #709, #14370, #18609 ),
 ( #12169, #27648, #9694, #16407, #23262, #27500 ),
 ( #5483, #7550, #12022, #21083, #7390, #1143 ) ),
 .UNSPECIFIED., .F., .F., .F.,
 ( 6, 6 ),
 ( 6, 6 ),
 ( 15.82768567779999991, 30.79603606440000263 ),
 ( 0.000000000000000000, 0.5000000000000000000 ),
 .UNSPECIFIED. ) ;
#16826 = CARTESIAN_POINT ( 'NONE',  ( 20.98512250110000110, -28.53090651930000021, -7.691805548749999666 ) ) ;
#16827 = CARTESIAN_POINT ( 'NONE',  ( 0.000000000000000000, -2.000000000000000000, 0.000000000000000000 ) ) ;
#16828 = ORIENTED_EDGE ( 'NONE', *, *, #27633, .T. ) ;
#16829 = CARTESIAN_POINT ( 'NONE',  ( 0.000000000000000000, -11.79999999999999893, 0.000000000000000000 ) ) ;
#16830 = DIRECTION ( 'NONE',  ( 0.000000000000000000, -1.000000000000000000, 0.000000000000000000 ) ) ;
#16831 = ORIENTED_EDGE ( 'NONE', *, *, #1523, .F. ) ;
#16832 = CARTESIAN_POINT ( 'NONE',  ( 7.215414233289999757, -74.50000000000000000, -40.70731707320000226 ) ) ;
#16833 = CARTESIAN_POINT ( 'NONE',  ( 0.5946929504664082433, -100.4010812937833350, -16.96993233685614300 ) ) ;
#16834 = FACE_OUTER_BOUND ( 'NONE', #24267, .T. ) ;
#16835 = CARTESIAN_POINT ( 'NONE',  ( 13.94204884902214658, -92.53260370676606783, 27.12694900991376912 ) ) ;
#16836 = CIRCLE ( 'NONE', #28000, 0.5000000000000004441 ) ;
#16837 = CARTESIAN_POINT ( 'NONE',  ( 23.65471649550000066, -72.84996959090000246, -30.57903112150000169 ) ) ;
#16838 = AXIS2_PLACEMENT_3D ( 'NONE', #23548, #9308, #3080 ) ;
#16839 = DIRECTION ( 'NONE',  ( 0.4794255386042040046, 0.000000000000000000, 0.8775825618903722036 ) ) ;
#16840 = CARTESIAN_POINT ( 'NONE',  ( 11.83146313070000133, -101.1461874320000049, -11.00634697169999932 ) ) ;
#16841 = CARTESIAN_POINT ( 'NONE',  ( -18.63062389896092341, -19.46426558511086569, 11.76718335430204299 ) ) ;
#16842 = CARTESIAN_POINT ( 'NONE',  ( 0.000000000000000000, -11.85850980319999870, 0.000000000000000000 ) ) ;
#16843 = DIRECTION ( 'NONE',  ( 0.4794255386042036160, 0.000000000000000000, 0.8775825618903723147 ) ) ;
#16844 = ORIENTED_EDGE ( 'NONE', *, *, #12974, .T. ) ;
#16845 = CARTESIAN_POINT ( 'NONE',  ( -10.61287167059999881, -19.46510050329999686, 19.30934957549999709 ) ) ;
#16846 = ORIENTED_EDGE ( 'NONE', *, *, #7558, .F. ) ;
#16847 = EDGE_CURVE ( 'NONE', #3368, #15375, #251, .T. ) ;
#16848 = EDGE_CURVE ( 'NONE', #12521, #10474, #2102, .T. ) ;
#16849 = CARTESIAN_POINT ( 'NONE',  ( -0.9714544087850000009, -64.02328494229999478, -24.65515989760000082 ) ) ;
#16850 = CARTESIAN_POINT ( 'NONE',  ( 9.393614098460000505, -37.68584072819999875, -22.97877291129999833 ) ) ;
#16851 = EDGE_CURVE ( 'NONE', #19704, #9831, #16587, .T. ) ;
#16852 = CARTESIAN_POINT ( 'NONE',  ( -27.80414915030000245, -92.67327634539999792, 1.811697503490000027 ) ) ;
#16853 = AXIS2_PLACEMENT_3D ( 'NONE', #27149, #8755, #17674 ) ;
#16854 = LINE ( 'NONE', #3320, #18982 ) ;
#16855 = EDGE_CURVE ( 'NONE', #3210, #10257, #23947, .T. ) ;
#16856 = CARTESIAN_POINT ( 'NONE',  ( 19.19205617106166883, -19.49520357620059130, -9.000935570425328436 ) ) ;
#16857 = ORIENTED_EDGE ( 'NONE', *, *, #26998, .F. ) ;
#16858 = CARTESIAN_POINT ( 'NONE',  ( -28.76693335801717666, -93.11247489672756217, 2.840853404041298713 ) ) ;
#16859 = CARTESIAN_POINT ( 'NONE',  ( -7.250053749315869212, -74.39269056244653200, -40.35493623770417315 ) ) ;
#16860 = EDGE_LOOP ( 'NONE', ( #11842, #3346, #5881, #17534 ) ) ;
#16861 = CARTESIAN_POINT ( 'NONE',  ( 8.386162616670347347, -68.18701404723893233, -25.21061241927545638 ) ) ;
#16862 = CARTESIAN_POINT ( 'NONE',  ( 7.913872602619999697, -36.43558290860000426, -21.40167476739999941 ) ) ;
#16863 = CARTESIAN_POINT ( 'NONE',  ( 22.26662627820000040, -57.47855601759999900, -7.066909182079999852 ) ) ;
#16864 = APPLICATION_CONTEXT ( 'automotive_design' ) ;
#16865 = CARTESIAN_POINT ( 'NONE',  ( -18.97570897180000316, -18.50000000000000000, 15.16944231589999958 ) ) ;
#16866 = ORIENTED_EDGE ( 'NONE', *, *, #6039, .T. ) ;
#16867 = CARTESIAN_POINT ( 'NONE',  ( -15.38068916850000001, -101.6095197629999944, 4.516181925269999731 ) ) ;
#16868 = CARTESIAN_POINT ( 'NONE',  ( -16.12803325799999854, -100.3774201490000024, 2.700167859220000022 ) ) ;
#16869 = CARTESIAN_POINT ( 'NONE',  ( -32.11921425309235190, -74.01249333572259559, -22.05455054358708011 ) ) ;
#16870 = CARTESIAN_POINT ( 'NONE',  ( -6.143223556138350361, -101.1586404113043898, 14.37947789112424601 ) ) ;
#16871 = AXIS2_PLACEMENT_3D ( 'NONE', #22973, #3018, #5032 ) ;
#16872 = ORIENTED_EDGE ( 'NONE', *, *, #4281, .T. ) ;
#16873 = CIRCLE ( 'NONE', #21091, 22.03370205219999889 ) ;
#16874 = CARTESIAN_POINT ( 'NONE',  ( 20.39783485576944599, -98.09459568642344607, -1.420636912331782353 ) ) ;
#16875 = DIRECTION ( 'NONE',  ( 0.000000000000000000, 1.000000000000000000, 0.000000000000000000 ) ) ;
#16876 = VECTOR ( 'NONE', #18259, 1000.000000000000000 ) ;
#16877 = CARTESIAN_POINT ( 'NONE',  ( 18.91112499396685465, -18.62337005498731912, -8.654031818350992111 ) ) ;
#16878 = CARTESIAN_POINT ( 'NONE',  ( -7.286203202325246764, -101.4304678898307372, 14.43370055275712183 ) ) ;
#16879 = ORIENTED_EDGE ( 'NONE', *, *, #14277, .F. ) ;
#16880 = DIRECTION ( 'NONE',  ( 0.8775825618903722036, 0.000000000000000000, -0.4794255386042041156 ) ) ;
#16881 = CARTESIAN_POINT ( 'NONE',  ( 8.988996100299999625, -34.66800400750000222, -19.43643858049999906 ) ) ;
#16882 = CARTESIAN_POINT ( 'NONE',  ( 36.31537122139999951, -79.49793013650000262, -14.89204469480000093 ) ) ;
#16883 = ORIENTED_EDGE ( 'NONE', *, *, #15229, .T. ) ;
#16884 = EDGE_CURVE ( 'NONE', #16942, #13903, #14046, .T. ) ;
#16885 = CARTESIAN_POINT ( 'NONE',  ( 36.76353006592368899, -79.41291915633111387, -14.66093257292968310 ) ) ;
#16886 = CARTESIAN_POINT ( 'NONE',  ( 6.664891844591124936, -100.9229461904473339, 15.16559953918201664 ) ) ;
#16887 = CARTESIAN_POINT ( 'NONE',  ( -0.8571442907775489450, -79.82540267843101844, 47.19917229225826816 ) ) ;
#16888 = EDGE_CURVE ( 'NONE', #5395, #20122, #5370, .T. ) ;
#16889 = ORIENTED_EDGE ( 'NONE', *, *, #12479, .F. ) ;
#16890 = CARTESIAN_POINT ( 'NONE',  ( -17.12548553040000243, -99.53431416519998720, 3.156821174210000081 ) ) ;
#16891 = ORIENTED_EDGE ( 'NONE', *, *, #26187, .T. ) ;
#16892 = AXIS2_PLACEMENT_3D ( 'NONE', #7607, #22900, #27122 ) ;
#16893 = CARTESIAN_POINT ( 'NONE',  ( 28.28014364260000235, -92.50732182220001221, 8.299785262969999522 ) ) ;
#16894 = ORIENTED_EDGE ( 'NONE', *, *, #201, .T. ) ;
#16895 = CIRCLE ( 'NONE', #5744, 1.000000000000000222 ) ;
#16896 = DIRECTION ( 'NONE',  ( 1.000000000000000000, 0.000000000000000000, 0.000000000000000000 ) ) ;
#16897 = CARTESIAN_POINT ( 'NONE',  ( -28.39367414323790229, -93.04141874247781629, -2.227239965210703776 ) ) ;
#16898 = EDGE_LOOP ( 'NONE', ( #17424, #28626, #22660, #19685 ) ) ;
#16899 = CARTESIAN_POINT ( 'NONE',  ( -21.60034897659999942, -79.81702851609999527, -32.77174746360000057 ) ) ;
#16900 = CARTESIAN_POINT ( 'NONE',  ( -11.62450342175550055, -60.96820961890185231, -22.92682159015150134 ) ) ;
#16901 = CARTESIAN_POINT ( 'NONE',  ( 25.40476796700415107, -67.67676320189275430, 10.87793065395078074 ) ) ;
#16902 = EDGE_LOOP ( 'NONE', ( #10752, #20405, #8000, #27717, #3874, #9574, #3310 ) ) ;
#16903 = CARTESIAN_POINT ( 'NONE',  ( -20.55443039410000239, -95.85308664750000673, -9.151112246150001184 ) ) ;
#16904 = CARTESIAN_POINT ( 'NONE',  ( 15.75263236761972863, -101.6484611539999747, 2.803083806627801433 ) ) ;
#16905 = CARTESIAN_POINT ( 'NONE',  ( -20.44152562849999910, -92.68419405429999358, 18.52892094230000097 ) ) ;
#16906 = CARTESIAN_POINT ( 'NONE',  ( 24.47825540369999686, -92.91851489729999969, -17.01759270650000033 ) ) ;
#16907 = CARTESIAN_POINT ( 'NONE',  ( -2.491468434920000252, -55.00753887619999460, -24.55868524289999755 ) ) ;
#16908 = CARTESIAN_POINT ( 'NONE',  ( 29.75862214763936819, -92.72722989466579691, 6.683900548007907894 ) ) ;
#16909 = VERTEX_POINT ( 'NONE', #5452 ) ;
#16910 = DIRECTION ( 'NONE',  ( 0.4794255386042040601, 0.000000000000000000, 0.8775825618903719816 ) ) ;
#16911 = DIRECTION ( 'NONE',  ( 0.6601796052711899065, 0.000000000000000000, -0.7511077744132169665 ) ) ;
#16912 = DIRECTION ( 'NONE',  ( 0.000000000000000000, 1.000000000000000000, 0.000000000000000000 ) ) ;
#16913 = CARTESIAN_POINT ( 'NONE',  ( -38.11607709268015043, -65.74504297427023403, 1.085364455066277101 ) ) ;
#16914 = CARTESIAN_POINT ( 'NONE',  ( -14.25438161831525363, -74.03830041542175877, 36.24026857307444516 ) ) ;
#16915 = AXIS2_PLACEMENT_3D ( 'NONE', #17901, #7125, #296 ) ;
#16916 = ADVANCED_FACE ( 'NONE', ( #822 ), #11700, .T. ) ;
#16917 = SHAPE_REPRESENTATION_RELATIONSHIP ( 'NONE' , 'NONE' ,  #2018, #8112 ) ;
#16918 = EDGE_CURVE ( 'NONE', #19506, #8148, #14652, .T. ) ;
#16919 = EDGE_LOOP ( 'NONE', ( #13288, #20798, #21241, #14900 ) ) ;
#16920 = LINE ( 'NONE', #25814, #25215 ) ;
#16921 = CARTESIAN_POINT ( 'NONE',  ( 21.34788073790000240, -35.28814185829999417, -7.426814485570000457 ) ) ;
#16922 = CIRCLE ( 'NONE', #19245, 55.50192378860000275 ) ;
#16923 = CARTESIAN_POINT ( 'NONE',  ( 41.00000000000000000, -80.50000000000000000, -10.20110288159999890 ) ) ;
#16924 = DIRECTION ( 'NONE',  ( 1.000000000000000000, 0.000000000000000000, 0.000000000000000000 ) ) ;
#16925 = ORIENTED_EDGE ( 'NONE', *, *, #18804, .F. ) ;
#16926 = CARTESIAN_POINT ( 'NONE',  ( -12.96048168789999977, -101.0356131030000029, -8.456406562079997968 ) ) ;
#16927 = DIRECTION ( 'NONE',  ( -0.1646113479699435889, 0.000000000000000000, 0.9863585068926603583 ) ) ;
#16928 = CARTESIAN_POINT ( 'NONE',  ( 9.348798002780000616, -13.50000000000000000, 17.11285995690000306 ) ) ;
#16929 = CARTESIAN_POINT ( 'NONE',  ( -7.941456924969999775, -100.0994409990000094, 15.28316630279999977 ) ) ;
#16930 = ORIENTED_EDGE ( 'NONE', *, *, #3849, .F. ) ;
#16931 = CARTESIAN_POINT ( 'NONE',  ( -0.009295818923119999674, -93.24058218830001010, 26.19215823259999709 ) ) ;
#16932 = CARTESIAN_POINT ( 'NONE',  ( -8.394720798919559357, -94.58015680889037924, -22.73927332636950993 ) ) ;
#16933 = CARTESIAN_POINT ( 'NONE',  ( -29.17304402409999753, -39.50000000000000000, -53.40089889099999709 ) ) ;
#16934 = PRESENTATION_LAYER_ASSIGNMENT (  '', '', ( #23473 ) ) ;
#16935 = DIRECTION ( 'NONE',  ( 0.000000000000000000, -1.000000000000000000, 0.000000000000000000 ) ) ;
#16936 = VERTEX_POINT ( 'NONE', #20905 ) ;
#16937 = CARTESIAN_POINT ( 'NONE',  ( 12.67863569023319492, -101.5409490182417329, -9.895065346989536437 ) ) ;
#16938 = ADVANCED_FACE ( 'NONE', ( #20615 ), #18857, .F. ) ;
#16939 = FACE_OUTER_BOUND ( 'NONE', #3988, .T. ) ;
#16940 = CARTESIAN_POINT ( 'NONE',  ( 25.62591688519999877, -71.82672919469999329, 11.84408135179999988 ) ) ;
#16941 = CARTESIAN_POINT ( 'NONE',  ( 7.007938636740000504, -99.64579651319999698, 15.84020959899999959 ) ) ;
#16942 = VERTEX_POINT ( 'NONE', #18129 ) ;
#16943 = CARTESIAN_POINT ( 'NONE',  ( -14.10481785270000010, -74.02367878169998505, 36.45432549239999531 ) ) ;
#16944 = CARTESIAN_POINT ( 'NONE',  ( 25.26718046270000073, -19.50000000000000000, 6.129403842640000377 ) ) ;
#16945 = DIRECTION ( 'NONE',  ( 1.000000000000000000, 0.000000000000000000, 0.000000000000000000 ) ) ;
#16946 = DIRECTION ( 'NONE',  ( 0.000000000000000000, 1.000000000000000000, 0.000000000000000000 ) ) ;
#16947 = ORIENTED_EDGE ( 'NONE', *, *, #15812, .F. ) ;
#16948 = AXIS2_PLACEMENT_3D ( 'NONE', #7071, #23099, #2844 ) ;
#16949 = DIRECTION ( 'NONE',  ( 0.7071067811865475727, 0.000000000000000000, 0.7071067811865475727 ) ) ;
#16950 = B_SPLINE_CURVE_WITH_KNOTS ( 'NONE', 3,
 ( #1674, #8624, #3567, #25858 ),
 .UNSPECIFIED., .F., .F.,
 ( 4, 4 ),
 ( 0.000000000000000000, 1.000000000000000000 ),
 .UNSPECIFIED. ) ;
#16951 = CARTESIAN_POINT ( 'NONE',  ( 8.664772570080000236, -60.49464403009999813, -22.56734825659999899 ) ) ;
#16952 = CARTESIAN_POINT ( 'NONE',  ( -39.07223452339999170, -73.87252278329999911, -7.323177335889999640 ) ) ;
#16953 = CARTESIAN_POINT ( 'NONE',  ( 23.15286878230000056, -57.80430419099999995, 10.38290477119999977 ) ) ;
#16954 = CARTESIAN_POINT ( 'NONE',  ( 0.000000000000000000, -23.00000000000000000, 0.000000000000000000 ) ) ;
#16955 = VERTEX_POINT ( 'NONE', #9810 ) ;
#16956 = EDGE_CURVE ( 'NONE', #3048, #25813, #7067, .T. ) ;
#16957 = CARTESIAN_POINT ( 'NONE',  ( 6.630693261409999373, -100.8088109309999965, 15.16285646280000066 ) ) ;
#16958 = CARTESIAN_POINT ( 'NONE',  ( 15.04054737160000066, -101.1411470200000053, 3.257342712189999823 ) ) ;
#16959 = CARTESIAN_POINT ( 'NONE',  ( -5.819199518928550141, -97.34036579023693037, 19.85381770611325791 ) ) ;
#16960 = AXIS2_PLACEMENT_3D ( 'NONE', #18020, #13643, #11300 ) ;
#16961 = DIRECTION ( 'NONE',  ( 1.000000000000000000, 0.000000000000000000, 0.000000000000000000 ) ) ;
#16962 = CARTESIAN_POINT ( 'NONE',  ( 5.003143695574637562, -92.66972459460949096, -30.08685070979726817 ) ) ;
#16963 = AXIS2_PLACEMENT_3D ( 'NONE', #11308, #8979, #6814 ) ;
#16964 = CARTESIAN_POINT ( 'NONE',  ( -6.670601060500000123, -97.64874574759998893, 18.82504149280000050 ) ) ;
#16965 = CARTESIAN_POINT ( 'NONE',  ( 6.598815769619999827, -93.39359504719999450, -26.37745322970000217 ) ) ;
#16966 = CARTESIAN_POINT ( 'NONE',  ( -1.598721155459999804E-14, -84.00000000000000000, 7.105427357599999217E-15 ) ) ;
#16967 = CARTESIAN_POINT ( 'NONE',  ( -17.94180966909999597, -74.00000000000000000, 18.81731824139999887 ) ) ;
#16968 = EDGE_LOOP ( 'NONE', ( #15056, #25755, #15384, #33 ) ) ;
#16969 = CIRCLE ( 'NONE', #7677, 8.000000000000000000 ) ;
#16970 = CARTESIAN_POINT ( 'NONE',  ( -17.12548553040000243, -99.53431416519998720, 3.156821174210000081 ) ) ;
#16971 = EDGE_LOOP ( 'NONE', ( #1760, #27880, #15823, #13025 ) ) ;
#16972 = CARTESIAN_POINT ( 'NONE',  ( -1.060320034430000113, -101.4334236450000049, -16.03230495190000227 ) ) ;
#16973 = EDGE_CURVE ( 'NONE', #28710, #17905, #18280, .T. ) ;
#16974 = CARTESIAN_POINT ( 'NONE',  ( -7.250938816910000639, -73.85300527940000848, 39.81408737849999824 ) ) ;
#16975 = DIRECTION ( 'NONE',  ( 0.000000000000000000, -1.000000000000000000, 0.000000000000000000 ) ) ;
#16976 = CARTESIAN_POINT ( 'NONE',  ( 9.334872109610000362E-16, -74.00000000000000000, -2.419703924680000090E-15 ) ) ;
#16977 = CARTESIAN_POINT ( 'NONE',  ( 15.82549146240000049, -101.1976625110000043, 4.106801947200000136 ) ) ;
#16978 = CARTESIAN_POINT ( 'NONE',  ( -8.306762876789999694, -99.70407914540000149, 15.05683357740000083 ) ) ;
#16979 = DIRECTION ( 'NONE',  ( 1.000000000000000000, 0.000000000000000000, 0.000000000000000000 ) ) ;
#16980 = AXIS2_PLACEMENT_3D ( 'NONE', #14854, #8293, #12799 ) ;
#16981 = CARTESIAN_POINT ( 'NONE',  ( 11.33780648110000122, -100.8733988930000010, -10.89600415129999966 ) ) ;
#16982 = CARTESIAN_POINT ( 'NONE',  ( -18.59805086797023321, -19.47341637985122631, 13.22102611671206240 ) ) ;
#16983 = CARTESIAN_POINT ( 'NONE',  ( 7.793340607010000198, -34.75995359360000236, -21.18684990219999875 ) ) ;
#16984 = DIRECTION ( 'NONE',  ( -0.000000000000000000, 1.000000000000000000, 0.000000000000000000 ) ) ;
#16985 = ORIENTED_EDGE ( 'NONE', *, *, #26230, .T. ) ;
#16986 = CARTESIAN_POINT ( 'NONE',  ( -39.50000000000000000, -63.30468293320000583, -2.309401076760000393 ) ) ;
#16987 = AXIS2_PLACEMENT_3D ( 'NONE', #25970, #5994, #1239 ) ;
#16988 = ORIENTED_EDGE ( 'NONE', *, *, #13728, .T. ) ;
#16989 = CARTESIAN_POINT ( 'NONE',  ( -2.080583965950000280, -64.78279487710000240, -25.39005782320000293 ) ) ;
#16990 = CARTESIAN_POINT ( 'NONE',  ( -27.68682485439999752, -31.69999999999999929, -50.68039294919999804 ) ) ;
#16991 = CARTESIAN_POINT ( 'NONE',  ( -19.51583823489999858, -52.61368720150000655, 13.56962763329999966 ) ) ;
#16992 = ORIENTED_EDGE ( 'NONE', *, *, #26119, .F. ) ;
#16993 = B_SPLINE_CURVE_WITH_KNOTS ( 'NONE', 5,
 ( #4051, #23735, #25926, #17036, #28240, #21273 ),
 .UNSPECIFIED., .F., .F.,
 ( 6, 6 ),
 ( 0.000000000000000000, 1.000000000000000000 ),
 .UNSPECIFIED. ) ;
#16994 = CARTESIAN_POINT ( 'NONE',  ( -40.00000000000000000, -69.00000000000000000, 3.236300116779999679E-15 ) ) ;
#16995 = DIRECTION ( 'NONE',  ( 1.000000000000000000, 0.000000000000000000, 0.000000000000000000 ) ) ;
#16996 = ORIENTED_EDGE ( 'NONE', *, *, #8198, .T. ) ;
#16997 = DIRECTION ( 'NONE',  ( 0.9620138697098239433, 0.000000000000000000, 0.2730005759809492893 ) ) ;
#16998 = ORIENTED_EDGE ( 'NONE', *, *, #5356, .T. ) ;
#16999 = ADVANCED_FACE ( 'NONE', ( #23783 ), #3058, .F. ) ;
#17000 = CARTESIAN_POINT ( 'NONE',  ( -17.48567531570000000, -18.50000000000000000, 12.33326151890000055 ) ) ;
#17001 = EDGE_CURVE ( 'NONE', #26473, #27727, #9065, .T. ) ;
#17002 = CARTESIAN_POINT ( 'NONE',  ( 22.13380541979999805, -19.18187901349999791, 9.708259679350000226 ) ) ;
#17003 = CARTESIAN_POINT ( 'NONE',  ( -15.42363691649999957, -67.46051717960000360, 22.84488648889999851 ) ) ;
#17004 = CARTESIAN_POINT ( 'NONE',  ( -3.355978770230000130, 4.440892098500000496E-16, -6.143077933229999843 ) ) ;
#17005 = ORIENTED_EDGE ( 'NONE', *, *, #9744, .T. ) ;
#17006 = CARTESIAN_POINT ( 'NONE',  ( -1.776356839399999804E-15, -89.50000000000000000, 0.000000000000000000 ) ) ;
#17007 = CARTESIAN_POINT ( 'NONE',  ( -12.46057752100000116, -101.1191090859999946, -10.51508789569999891 ) ) ;
#17008 = EDGE_CURVE ( 'NONE', #12945, #6664, #1649, .T. ) ;
#17009 = CARTESIAN_POINT ( 'NONE',  ( -7.227961103978413959, -73.66549258102378417, 39.43512252455204248 ) ) ;
#17010 = CARTESIAN_POINT ( 'NONE',  ( -7.888607335952146471, -100.4507315480479548, 14.99179633818354240 ) ) ;
#17011 = ORIENTED_EDGE ( 'NONE', *, *, #2998, .T. ) ;
#17012 = ADVANCED_FACE ( 'NONE', ( #23228 ), #28021, .T. ) ;
#17013 = AXIS2_PLACEMENT_3D ( 'NONE', #7164, #16030, #20717 ) ;
#17014 = FACE_OUTER_BOUND ( 'NONE', #19089, .T. ) ;
#17015 = CARTESIAN_POINT ( 'NONE',  ( -31.89935321680000158, -74.00000000000000000, -21.99985828019999801 ) ) ;
#17016 = CARTESIAN_POINT ( 'NONE',  ( 36.68904416859999884, -80.12912447070000610, -14.08963035319999868 ) ) ;
#17017 = ORIENTED_EDGE ( 'NONE', *, *, #9071, .F. ) ;
#17018 = CARTESIAN_POINT ( 'NONE',  ( 6.661181729204114887, -100.9609609850482883, 15.13455079199698083 ) ) ;
#17019 = VECTOR ( 'NONE', #7321, 1000.000000000000114 ) ;
#17020 = CARTESIAN_POINT ( 'NONE',  ( 11.49573228323775531, -101.1962283502455335, -10.04692880049169013 ) ) ;
#17021 = ORIENTED_EDGE ( 'NONE', *, *, #1470, .T. ) ;
#17022 = CARTESIAN_POINT ( 'NONE',  ( -18.13582102693932896, -98.48184326581569792, 4.852288895080256736 ) ) ;
#17023 = VERTEX_POINT ( 'NONE', #16658 ) ;
#17024 = CARTESIAN_POINT ( 'NONE',  ( 27.05235185969999634, -92.55031885960001148, 9.384696477129999437 ) ) ;
#17025 = DIRECTION ( 'NONE',  ( 0.000000000000000000, -1.000000000000000000, 0.000000000000000000 ) ) ;
#17026 = CARTESIAN_POINT ( 'NONE',  ( 4.226834115039999951, -93.34497626389999425, 25.39917024580000060 ) ) ;
#17027 = VERTEX_POINT ( 'NONE', #17221 ) ;
#17028 = CARTESIAN_POINT ( 'NONE',  ( 9.476129726560001743, -36.00000000000000000, -20.06309461059999677 ) ) ;
#17029 = DIRECTION ( 'NONE',  ( 0.4794255386042036160, 0.000000000000000000, 0.8775825618903723147 ) ) ;
#17030 = EDGE_LOOP ( 'NONE', ( #186, #2820, #26173, #19342 ) ) ;
#17031 = CARTESIAN_POINT ( 'NONE',  ( 24.01307781190000057, -93.00000000000000000, -18.61462211579999959 ) ) ;
#17032 = CARTESIAN_POINT ( 'NONE',  ( 7.500294343269999331, -101.1699703470000031, 13.83260060669999980 ) ) ;
#17033 = CARTESIAN_POINT ( 'NONE',  ( 25.32394939313839188, -67.45391685492131728, 10.87937782985497215 ) ) ;
#17034 = EDGE_LOOP ( 'NONE', ( #12271, #6265, #9702, #20126 ) ) ;
#17035 = EDGE_CURVE ( 'NONE', #3774, #13014, #13721, .T. ) ;
#17036 = CARTESIAN_POINT ( 'NONE',  ( 25.57918037516483523, -64.69849890637429723, 1.120748866632130580 ) ) ;
#17037 = CARTESIAN_POINT ( 'NONE',  ( 13.31770606849999972, -100.4792519539999915, -9.213118301410000655 ) ) ;
#17038 = CARTESIAN_POINT ( 'NONE',  ( -16.54318588419999969, -93.00000000000000000, 25.62368046950000178 ) ) ;
#17039 = CARTESIAN_POINT ( 'NONE',  ( 24.05283483419999868, -94.34469964500000572, -8.234368469370000554 ) ) ;
#17040 = CARTESIAN_POINT ( 'NONE',  ( -38.25000000000000000, -63.00000000000000000, -1.587713240270000048 ) ) ;
#17041 = DIRECTION ( 'NONE',  ( 0.6710129359900831592, 0.000000000000000000, -0.7414456417930911369 ) ) ;
#17042 = CARTESIAN_POINT ( 'NONE',  ( -12.05824591346449459, -67.66818470673190689, -24.37625945436767694 ) ) ;
#17043 = ORIENTED_EDGE ( 'NONE', *, *, #28760, .T. ) ;
#17044 = ADVANCED_FACE ( 'NONE', ( #5590 ), #1514, .F. ) ;
#17045 = CARTESIAN_POINT ( 'NONE',  ( 27.36513940969999936, -92.50000000000000000, 13.03937715500000039 ) ) ;
#17046 = CARTESIAN_POINT ( 'NONE',  ( -26.69293917519999937, -23.30310889129999907, -48.86109741659999628 ) ) ;
#17047 = CARTESIAN_POINT ( 'NONE',  ( 38.62788938250000115, -74.00000000000000000, 7.627566167509999495 ) ) ;
#17048 = CARTESIAN_POINT ( 'NONE',  ( 8.969779973459999667, -35.75711592580000087, -20.13916512639999823 ) ) ;
#17049 = CARTESIAN_POINT ( 'NONE',  ( 25.25824993130000351, -73.10684313109999266, -29.82725550210000165 ) ) ;
#17050 = B_SPLINE_SURFACE_WITH_KNOTS ( 'NONE', 5, 5, ( 
 ( #12566, #28305, #12706, #19565, #23945, #24234, #3982, #6015, #19842 ),
 ( #1806, #28594, #15031, #4267, #26419, #14896, #28725, #21620, #8763 ),
 ( #5880, #21902, #25856, #23805, #8338, #10648, #28453, #8487, #17388 ),
 ( #26861, #24519, #4706, #4994, #514, #6606, #13434, #11077, #7050 ),
 ( #19994, #13586, #22191, #20292, #67, #9206, #22494, #8913, #9361 ),
 ( #22338, #17822, #11390, #2386, #2536, #13739, #13881, #22639, #26716 ),
 ( #18262, #22786, #2824, #11242, #11686, #20597, #15619, #657, #11977 ),
 ( #12261, #5434, #27857, #7906, #5575, #955, #12116, #16786, #9932 ),
 ( #23353, #18846, #25682, #14591, #808, #27300, #7495, #7338, #2977 ),
 ( #11836, #9649, #16204, #27450, #25269, #23625, #28005, #8041, #14860 ),
 ( #16929, #3944, #3665, #12808, #12668, #12527, #24043, #23907, #5978 ),
 ( #25821, #23764, #1498, #21580, #6408, #5844, #26092, #6121, #21717 ) ),
 .UNSPECIFIED., .F., .F., .F.,
 ( 6, 3, 3, 6 ),
 ( 6, 3, 6 ),
 ( 3.852920539479999906, 4.834764074430000669, 6.134713715060000183, 8.383984506240000911 ),
 ( 0.000000000000000000, 0.2500000000000000000, 0.5000000000000000000 ),
 .UNSPECIFIED. ) ;
#17051 = VERTEX_POINT ( 'NONE', #23368 ) ;
#17052 = B_SPLINE_CURVE_WITH_KNOTS ( 'NONE', 5,
 ( #16691, #28326, #25593, #7951, #5759, #1270 ),
 .UNSPECIFIED., .F., .F.,
 ( 6, 6 ),
 ( 0.000000000000000000, 1.000000000000000000 ),
 .UNSPECIFIED. ) ;
#17053 = CARTESIAN_POINT ( 'NONE',  ( 21.43077048929999862, -35.81319862919999508, -7.299949289889999804 ) ) ;
#17054 = ORIENTED_EDGE ( 'NONE', *, *, #503, .F. ) ;
#17055 = CARTESIAN_POINT ( 'NONE',  ( 21.46039065680000135, -36.43422328669999644, -7.619628857949999556 ) ) ;
#17056 = CARTESIAN_POINT ( 'NONE',  ( -20.70743651480000125, -111.0000000000000000, -4.683547831859999455 ) ) ;
#17057 = EDGE_LOOP ( 'NONE', ( #1155, #8003, #25343, #7680, #19770, #6750, #26031, #17183, #14384 ) ) ;
#17058 = CARTESIAN_POINT ( 'NONE',  ( 12.05761442979999920, -96.99283697629999779, 17.05217550289999906 ) ) ;
#17059 = DIRECTION ( 'NONE',  ( -1.000000000000000000, -0.000000000000000000, -1.738658080640000114E-17 ) ) ;
#17060 = CARTESIAN_POINT ( 'NONE',  ( -0.5726204572655302361, -18.60284036877294156, -21.53722082371633917 ) ) ;
#17061 = CARTESIAN_POINT ( 'NONE',  ( 1.924356917819999957, -93.14733690340000294, 27.32343874049999854 ) ) ;
#17062 = EDGE_CURVE ( 'NONE', #20989, #28649, #21188, .T. ) ;
#17063 = CARTESIAN_POINT ( 'NONE',  ( 6.974892859179999682, -49.11505549650000546, -21.98941332900000134 ) ) ;
#17064 = CARTESIAN_POINT ( 'NONE',  ( 0.000000000000000000, 0.000000000000000000, 0.000000000000000000 ) ) ;
#17065 = ORIENTED_EDGE ( 'NONE', *, *, #14662, .T. ) ;
#17066 = ADVANCED_FACE ( 'NONE', ( #9948 ), #25371, .F. ) ;
#17067 = DIRECTION ( 'NONE',  ( -0.09756097560976760563, 0.000000000000000000, -0.9952295494196654602 ) ) ;
#17068 = CARTESIAN_POINT ( 'NONE',  ( -27.08130798099999836, -92.87437365140000622, -4.263279399680000026 ) ) ;
#17069 = CARTESIAN_POINT ( 'NONE',  ( 39.61603006823808215, -73.75061506092693264, 7.239953483540725543 ) ) ;
#17070 = VERTEX_POINT ( 'NONE', #8191 ) ;
#17071 = CARTESIAN_POINT ( 'NONE',  ( 18.91112499059999763, -18.62337005500000231, -8.654031818700001821 ) ) ;
#17072 = DIRECTION ( 'NONE',  ( 0.000000000000000000, -1.000000000000000000, 0.000000000000000000 ) ) ;
#17073 = CARTESIAN_POINT ( 'NONE',  ( -1.281139941660000225, -19.46501104069999855, -22.08267515169999839 ) ) ;
#17074 = DIRECTION ( 'NONE',  ( 1.000000000000000000, 0.000000000000000000, 0.000000000000000000 ) ) ;
#17075 = ORIENTED_EDGE ( 'NONE', *, *, #24416, .T. ) ;
#17076 = EDGE_CURVE ( 'NONE', #21210, #11981, #26774, .T. ) ;
#17077 = DIRECTION ( 'NONE',  ( 1.000000000000000000, 0.000000000000000000, 0.000000000000000000 ) ) ;
#17078 = CARTESIAN_POINT ( 'NONE',  ( 0.08847858422719999394, -101.5964542560000012, -16.04011128580000189 ) ) ;
#17079 = CARTESIAN_POINT ( 'NONE',  ( 22.71963733680000175, -57.44066854489999940, -9.099149309629998683 ) ) ;
#17080 = CARTESIAN_POINT ( 'NONE',  ( -38.68350846249999364, -73.93831524339999817, -7.318371247189999984 ) ) ;
#17081 = CARTESIAN_POINT ( 'NONE',  ( 6.153546133999999945, -93.00000450890000536, 28.82528558229999760 ) ) ;
#17082 = AXIS2_PLACEMENT_3D ( 'NONE', #10591, #17186, #8287 ) ;
#17083 = CARTESIAN_POINT ( 'NONE',  ( -10.53866346480000082, -19.41822431039999941, -21.28095825400000152 ) ) ;
#17084 = ORIENTED_EDGE ( 'NONE', *, *, #5783, .T. ) ;
#17085 = CARTESIAN_POINT ( 'NONE',  ( 6.664266769160000159, -101.1191090859999946, 14.88020880370000043 ) ) ;
#17086 = CARTESIAN_POINT ( 'NONE',  ( -15.68499803141670057, -92.57495907656227985, -24.03044298549235691 ) ) ;
#17087 = AXIS2_PLACEMENT_3D ( 'NONE', #22656, #1240, #23927 ) ;
#17088 = CARTESIAN_POINT ( 'NONE',  ( -7.340076801780219817, -98.99956641980976713, 17.08769940940410237 ) ) ;
#17089 = B_SPLINE_CURVE_WITH_KNOTS ( 'NONE', 5,
 ( #25442, #19019, #9971, #18884, #14637, #23533 ),
 .UNSPECIFIED., .F., .F.,
 ( 6, 6 ),
 ( -40.74965564189999867, -28.77371845028335073 ),
 .UNSPECIFIED. ) ;
#17090 = CARTESIAN_POINT ( 'NONE',  ( 21.21808891099999883, -34.59820414320000026, -7.670974023059999425 ) ) ;
#17091 = CARTESIAN_POINT ( 'NONE',  ( 6.623136366559999821, -92.50000000000000000, -29.58057261400000115 ) ) ;
#17092 = DIRECTION ( 'NONE',  ( 0.000000000000000000, 1.000000000000000000, 0.000000000000000000 ) ) ;
#17093 = ORIENTED_EDGE ( 'NONE', *, *, #21446, .F. ) ;
#17094 = CARTESIAN_POINT ( 'NONE',  ( 8.553834212409999083, -94.06807348059999185, -23.81750769579999982 ) ) ;
#17095 = CIRCLE ( 'NONE', #23608, 55.67692378859999991 ) ;
#17096 = AXIS2_PLACEMENT_3D ( 'NONE', #7939, #9968, #18739 ) ;
#17097 = CARTESIAN_POINT ( 'NONE',  ( 20.65664752990000252, -31.58327036160000389, -8.509521500050000853 ) ) ;
#17098 = DIRECTION ( 'NONE',  ( 0.000000000000000000, 1.000000000000000000, 0.000000000000000000 ) ) ;
#17099 = CARTESIAN_POINT ( 'NONE',  ( 0.000000000000000000, -13.50000000000000000, 0.000000000000000000 ) ) ;
#17100 = ORIENTED_EDGE ( 'NONE', *, *, #14978, .F. ) ;
#17101 = CARTESIAN_POINT ( 'NONE',  ( -11.41594931139999858, -19.46510050329999686, -18.84569254350000023 ) ) ;
#17102 = DIRECTION ( 'NONE',  ( 0.4999999999997570277, 0.000000000000000000, 0.8660254037845789288 ) ) ;
#17103 = ORIENTED_EDGE ( 'NONE', *, *, #13176, .F. ) ;
#17104 = EDGE_CURVE ( 'NONE', #11916, #24358, #23506, .T. ) ;
#17105 = EDGE_CURVE ( 'NONE', #18741, #23988, #12751, .T. ) ;
#17106 = CARTESIAN_POINT ( 'NONE',  ( 12.59683198944025229, -94.65677004896708979, -20.59035092372582554 ) ) ;
#17107 = DIRECTION ( 'NONE',  ( 0.4794255386042040601, 0.000000000000000000, 0.8775825618903719816 ) ) ;
#17108 = CARTESIAN_POINT ( 'NONE',  ( 36.50549972238673035, -74.62369757142499793, -14.71598444713541021 ) ) ;
#17109 = AXIS2_PLACEMENT_3D ( 'NONE', #13421, #2372, #20135 ) ;
#17110 = CARTESIAN_POINT ( 'NONE',  ( 16.40944971170530309, -94.60237058323863835, 17.21713387757399971 ) ) ;
#17111 = CARTESIAN_POINT ( 'NONE',  ( -22.70539113190000080, -72.04110636640000109, 17.08947363740000114 ) ) ;
#17112 = CARTESIAN_POINT ( 'NONE',  ( -36.79999999999999716, -65.14977478849999670, -0.1732050807570000017 ) ) ;
#17113 = CARTESIAN_POINT ( 'NONE',  ( -19.23753200850040912, -19.48999941762926369, 14.12819559392180224 ) ) ;
#17114 = CARTESIAN_POINT ( 'NONE',  ( -27.18988201479999844, -25.69844555429999744, -49.77074518290000071 ) ) ;
#17115 = CARTESIAN_POINT ( 'NONE',  ( 24.10654937457443125, -94.27895761462396251, -8.513691059147493689 ) ) ;
#17116 = CARTESIAN_POINT ( 'NONE',  ( 40.70731707320000226, -74.50000000000000000, 7.215414233289999757 ) ) ;
#17117 = ORIENTED_EDGE ( 'NONE', *, *, #22270, .F. ) ;
#17118 = CARTESIAN_POINT ( 'NONE',  ( 7.491375829749999937, -18.50000000000000000, -19.98345411639999725 ) ) ;
#17119 = TOROIDAL_SURFACE ( 'NONE', #15714, 7.750000000000000000, 0.5000000000000000000 ) ;
#17120 = ORIENTED_EDGE ( 'NONE', *, *, #23443, .F. ) ;
#17121 = CARTESIAN_POINT ( 'NONE',  ( 22.51853742080000131, -36.00000000000000000, -11.01541626720000089 ) ) ;
#17122 = ORIENTED_EDGE ( 'NONE', *, *, #15642, .T. ) ;
#17123 = EDGE_CURVE ( 'NONE', #26673, #4890, #13043, .T. ) ;
#17124 = CARTESIAN_POINT ( 'NONE',  ( -1.448823250100000015, -58.77396426510000538, -23.58892699440000129 ) ) ;
#17125 = CARTESIAN_POINT ( 'NONE',  ( 9.214873172669999946, -37.66961404259999568, -22.49121690919999850 ) ) ;
#17126 = CARTESIAN_POINT ( 'NONE',  ( -29.15742847839999996, -92.53610956480000027, 4.773646594879999761 ) ) ;
#17127 = CARTESIAN_POINT ( 'NONE',  ( -0.6875333948397619466, -101.1962283502373623, -15.25188306018329243 ) ) ;
#17128 = ORIENTED_EDGE ( 'NONE', *, *, #17487, .T. ) ;
#17129 = CARTESIAN_POINT ( 'NONE',  ( -25.57735248450000043, -37.08699221940000257, -46.81902967690000139 ) ) ;
#17130 = CARTESIAN_POINT ( 'NONE',  ( -13.70187146129979183, -57.41946977618258074, 20.98050236089959952 ) ) ;
#17131 = ORIENTED_EDGE ( 'NONE', *, *, #11744, .F. ) ;
#17132 = DIRECTION ( 'NONE',  ( 0.000000000000000000, -1.000000000000000000, 0.000000000000000000 ) ) ;
#17133 = ORIENTED_EDGE ( 'NONE', *, *, #1222, .T. ) ;
#17134 = AXIS2_PLACEMENT_3D ( 'NONE', #9444, #12059, #7136 ) ;
#17135 = ADVANCED_FACE ( 'NONE', ( #25551 ), #18753, .T. ) ;
#17136 = CIRCLE ( 'NONE', #10589, 3.499999999999999556 ) ;
#17137 = AXIS2_PLACEMENT_3D ( 'NONE', #21541, #1597, #28100 ) ;
#17138 = CARTESIAN_POINT ( 'NONE',  ( -19.35716652280000005, -18.50000000000000000, 15.34467299940000018 ) ) ;
#17139 = CARTESIAN_POINT ( 'NONE',  ( -15.61807470970000011, -101.5138947819999942, 3.547044975749999995 ) ) ;
#17140 = CARTESIAN_POINT ( 'NONE',  ( -27.68682485439999752, -24.80000000000000071, -50.68039294919999804 ) ) ;
#17141 = CARTESIAN_POINT ( 'NONE',  ( -20.45733727490000220, -60.27256034759999892, 14.77382382620000101 ) ) ;
#17142 = ORIENTED_EDGE ( 'NONE', *, *, #9550, .F. ) ;
#17143 =( GEOMETRIC_REPRESENTATION_CONTEXT ( 3 ) GLOBAL_UNCERTAINTY_ASSIGNED_CONTEXT ( ( #3351 ) ) GLOBAL_UNIT_ASSIGNED_CONTEXT ( ( #10188, #19512, #21429 ) ) REPRESENTATION_CONTEXT ( 'NONE', 'WORKASPACE' ) );
#17144 = CYLINDRICAL_SURFACE ( 'NONE', #2278, 3.749999999999996447 ) ;
#17145 = CARTESIAN_POINT ( 'NONE',  ( -12.55040281159999971, -101.4254868729999970, -9.874220623960001220 ) ) ;
#17146 = CARTESIAN_POINT ( 'NONE',  ( -0.5672159954309998753, -18.50000000000000000, -21.33394993619999624 ) ) ;
#17147 = CARTESIAN_POINT ( 'NONE',  ( -7.556190961256522343, -101.1451610289769718, 14.54526516815933590 ) ) ;
#17148 = EDGE_LOOP ( 'NONE', ( #5778, #22184, #2160, #27030 ) ) ;
#17149 = DIRECTION ( 'NONE',  ( 1.000000000000000000, 0.000000000000000000, 0.000000000000000000 ) ) ;
#17150 = DIRECTION ( 'NONE',  ( 1.000000000000000000, 0.000000000000000000, 0.000000000000000000 ) ) ;
#17151 = CARTESIAN_POINT ( 'NONE',  ( 37.07813615679999941, -80.00739956740001446, -13.83267119569999970 ) ) ;
#17152 = VERTEX_POINT ( 'NONE', #22032 ) ;
#17153 = AXIS2_PLACEMENT_3D ( 'NONE', #16410, #5345, #18754 ) ;
#17154 = ADVANCED_FACE ( 'NONE', ( #21736 ), #14216, .T. ) ;
#17155 = CIRCLE ( 'NONE', #19477, 30.50000000000000000 ) ;
#17156 = CARTESIAN_POINT ( 'NONE',  ( 6.785573360597900283, -100.4872618017465840, 15.49051439867366398 ) ) ;
#17157 = CARTESIAN_POINT ( 'NONE',  ( -1.451021762614941979, -80.03759595315190722, 47.10371954600015698 ) ) ;
#17158 = ORIENTED_EDGE ( 'NONE', *, *, #26589, .T. ) ;
#17159 = CARTESIAN_POINT ( 'NONE',  ( -40.00000000000000000, -73.00000000000000000, 2.464695114669999848E-15 ) ) ;
#17160 = ORIENTED_EDGE ( 'NONE', *, *, #27284, .F. ) ;
#17161 = CARTESIAN_POINT ( 'NONE',  ( 22.56940788859999714, -57.43018266629999857, 10.15711811299999923 ) ) ;
#17162 = CARTESIAN_POINT ( 'NONE',  ( 7.215414233289999757, -74.50000000000000000, 40.70731707320000226 ) ) ;
#17163 = ADVANCED_FACE ( 'NONE', ( #4399 ), #24427, .F. ) ;
#17164 = ORIENTED_EDGE ( 'NONE', *, *, #3412, .T. ) ;
#17165 = CARTESIAN_POINT ( 'NONE',  ( 12.86597616020000068, -100.8023006570000035, -9.130347141119999677 ) ) ;
#17166 = CARTESIAN_POINT ( 'NONE',  ( -3.577689640331729759, -18.50000000000000000, -25.07857796645360793 ) ) ;
#17167 = B_SPLINE_CURVE_WITH_KNOTS ( 'NONE', 5,
 ( #24989, #11108, #13765, #27182, #542, #22664 ),
 .UNSPECIFIED., .F., .F.,
 ( 6, 6 ),
 ( 0.000000000000000000, 1.000000000000000000 ),
 .UNSPECIFIED. ) ;
#17168 = VERTEX_POINT ( 'NONE', #8743 ) ;
#17169 = FACE_OUTER_BOUND ( 'NONE', #12755, .T. ) ;
#17170 = DIRECTION ( 'NONE',  ( 0.7414446217286146945, 0.000000000000000000, 0.6710140631236514164 ) ) ;
#17171 = CARTESIAN_POINT ( 'NONE',  ( -23.48382783139999930, -92.84292833370000153, -19.25540828950000360 ) ) ;
#17172 = CARTESIAN_POINT ( 'NONE',  ( -3.649267921049999863, -18.50000000000000000, -24.01816718290000097 ) ) ;
#17173 = ORIENTED_EDGE ( 'NONE', *, *, #6517, .T. ) ;
#17174 = TOROIDAL_SURFACE ( 'NONE', #8778, 6.750000000000000000, 0.5000000000000000000 ) ;
#17175 = CARTESIAN_POINT ( 'NONE',  ( -13.15906405200000151, -99.57787118749999422, -11.31977148680000056 ) ) ;
#17176 = VECTOR ( 'NONE', #17724, 999.9999999999998863 ) ;
#17177 = CARTESIAN_POINT ( 'NONE',  ( 12.85509542230000157, -100.8455998110000138, -9.598705754820000990 ) ) ;
#17178 = CARTESIAN_POINT ( 'NONE',  ( -18.69985100839999959, -93.00000000000000000, 22.78328762010000119 ) ) ;
#17179 = CARTESIAN_POINT ( 'NONE',  ( 23.50847989309999875, -93.85715850779999414, -8.212858164749999190 ) ) ;
#17180 = CARTESIAN_POINT ( 'NONE',  ( -2.582194743379999657, -56.19735282230000450, -25.20298037470000097 ) ) ;
#17181 = CARTESIAN_POINT ( 'NONE',  ( 11.37093174122694528, -72.27543338683032914, -27.00921921794252967 ) ) ;
#17182 = CARTESIAN_POINT ( 'NONE',  ( -38.25000000000000000, -65.63577453799999262, -1.587713240270000048 ) ) ;
#17183 = ORIENTED_EDGE ( 'NONE', *, *, #22791, .F. ) ;
#17184 = CARTESIAN_POINT ( 'NONE',  ( 9.855634485030901004, -64.48636389391205626, -24.31831199924348397 ) ) ;
#17185 = CARTESIAN_POINT ( 'NONE',  ( -14.01337423630000067, -80.50000000000000000, 36.66316738249999929 ) ) ;
#17186 = DIRECTION ( 'NONE',  ( 0.000000000000000000, 1.000000000000000000, 0.000000000000000000 ) ) ;
#17187 = CARTESIAN_POINT ( 'NONE',  ( 18.81756521970000406, -18.50000000000000000, 9.528581421409999308 ) ) ;
#17188 = CARTESIAN_POINT ( 'NONE',  ( -13.78473438695133346, -69.07614453243721186, 23.18529913744219328 ) ) ;
#17189 = CARTESIAN_POINT ( 'NONE',  ( -40.00000000000000000, -74.00000000000000000, 3.466919520389999841E-15 ) ) ;
#17190 = CARTESIAN_POINT ( 'NONE',  ( -11.90444329340000174, -64.24504203739999753, -23.68394282290000064 ) ) ;
#17191 = CARTESIAN_POINT ( 'NONE',  ( -22.43272078519999724, -80.50000000000000000, -32.20769377289999369 ) ) ;
#17192 = EDGE_CURVE ( 'NONE', #26794, #21398, #12378, .T. ) ;
#17193 = EDGE_CURVE ( 'NONE', #9831, #5266, #26398, .T. ) ;
#17194 = AXIS2_PLACEMENT_3D ( 'NONE', #5076, #22867, #3062 ) ;
#17195 = ORIENTED_EDGE ( 'NONE', *, *, #2545, .T. ) ;
#17196 = CARTESIAN_POINT ( 'NONE',  ( 21.11704720389999679, -35.76753062550000095, -8.346333568960000449 ) ) ;
#17197 = VERTEX_POINT ( 'NONE', #26263 ) ;
#17198 = CARTESIAN_POINT ( 'NONE',  ( 21.08638048839999968, -36.32484399220000171, -8.697366343609999717 ) ) ;
#17199 = CARTESIAN_POINT ( 'NONE',  ( -42.89961768690000099, -65.31510159580000163, -0.3466308900769999313 ) ) ;
#17200 = EDGE_CURVE ( 'NONE', #22875, #23028, #736, .T. ) ;
#17201 = EDGE_LOOP ( 'NONE', ( #21316, #20787, #6993, #18899 ) ) ;
#17202 = CARTESIAN_POINT ( 'NONE',  ( -12.73050580650000008, -101.1716782170000073, -9.245982730369998848 ) ) ;
#17203 = EDGE_CURVE ( 'NONE', #22807, #22871, #19313, .T. ) ;
#17204 = CARTESIAN_POINT ( 'NONE',  ( -2.865017121281941748, -64.99739744814985443, -26.59911453002877124 ) ) ;
#17205 = CARTESIAN_POINT ( 'NONE',  ( -2.864434201389999934, -99.61931799660000308, -17.24218458769999884 ) ) ;
#17206 = CARTESIAN_POINT ( 'NONE',  ( 9.524618309619999224, -53.22700740319999824, -23.40924512820000203 ) ) ;
#17207 = CARTESIAN_POINT ( 'NONE',  ( 0.000000000000000000, -2.000000000000000000, 0.000000000000000000 ) ) ;
#17208 = ORIENTED_EDGE ( 'NONE', *, *, #18312, .F. ) ;
#17209 = CARTESIAN_POINT ( 'NONE',  ( 12.45133382055230165, -101.6484611539999747, -10.04845847643241541 ) ) ;
#17210 = CARTESIAN_POINT ( 'NONE',  ( 22.71928070270000077, -19.44965585980000000, 1.104521532629999969 ) ) ;
#17211 = CARTESIAN_POINT ( 'NONE',  ( 22.41768028079999908, -65.59529275500000267, 11.91456822289999984 ) ) ;
#17212 = CARTESIAN_POINT ( 'NONE',  ( 6.944463756510000252, -99.57787269160000676, 15.90826982280000124 ) ) ;
#17213 = EDGE_LOOP ( 'NONE', ( #10377, #18566, #20, #14649 ) ) ;
#17214 = FACE_OUTER_BOUND ( 'NONE', #28679, .T. ) ;
#17215 = AXIS2_PLACEMENT_3D ( 'NONE', #18896, #7553, #5347 ) ;
#17216 = CARTESIAN_POINT ( 'NONE',  ( -1.604812007069718272, -64.93834275522041821, -25.19371719667666198 ) ) ;
#17217 = CARTESIAN_POINT ( 'NONE',  ( -41.70685699858434958, -63.05597747387410834, -2.814055025999628867 ) ) ;
#17218 = CARTESIAN_POINT ( 'NONE',  ( 5.329070518200000398E-15, -74.50000000000000000, 0.000000000000000000 ) ) ;
#17219 = ORIENTED_EDGE ( 'NONE', *, *, #26996, .T. ) ;
#17220 = CIRCLE ( 'NONE', #12106, 2.000000000000000000 ) ;
#17221 = CARTESIAN_POINT ( 'NONE',  ( -37.75000000000000000, -65.63577453799999262, -0.7216878364849999006 ) ) ;
#17222 = DIRECTION ( 'NONE',  ( 0.000000000000000000, -1.000000000000000000, 0.000000000000000000 ) ) ;
#17223 = CARTESIAN_POINT ( 'NONE',  ( 9.577933644319998052, -58.81640545049999957, -23.56560165069999968 ) ) ;
#17224 = B_SPLINE_CURVE_WITH_KNOTS ( 'NONE', 3,
 ( #8461, #1237, #12821, #17217, #21185, #14470, #3677, #3960, #1511, #18991 ),
 .UNSPECIFIED., .F., .F.,
 ( 4, 2, 2, 2, 4 ),
 ( 0.000000000000000000, 0.2500000000000000000, 0.5000000000000000000, 0.7500000000000000000, 1.000000000000000000 ),
 .UNSPECIFIED. ) ;
#17225 = CARTESIAN_POINT ( 'NONE',  ( 15.07019258820000118, -101.1848541600000004, 2.542738038029999981 ) ) ;
#17226 = CARTESIAN_POINT ( 'NONE',  ( 23.02633534789999814, -60.04642514249999863, 10.32969153620000213 ) ) ;
#17227 = DIRECTION ( 'NONE',  ( 0.000000000000000000, -1.000000000000000000, 0.000000000000000000 ) ) ;
#17228 = VERTEX_POINT ( 'NONE', #15151 ) ;
#17229 = B_SPLINE_CURVE_WITH_KNOTS ( 'NONE', 5,
 ( #13413, #341, #26989, #9184, #24802, #13861, #18089, #4839, #13718 ),
 .UNSPECIFIED., .F., .F.,
 ( 6, 3, 6 ),
 ( 0.000000000000000000, 0.3451758947491398444, 1.000000000000000000 ),
 .UNSPECIFIED. ) ;
#17230 = CARTESIAN_POINT ( 'NONE',  ( 6.933748734719999973, -99.99711545080000974, 15.71060619540000047 ) ) ;
#17231 = CARTESIAN_POINT ( 'NONE',  ( -15.77460418939101849, -92.56934535156428012, -24.02693241158716120 ) ) ;
#17232 = EDGE_CURVE ( 'NONE', #13203, #3822, #24897, .T. ) ;
#17233 = DIRECTION ( 'NONE',  ( 0.000000000000000000, 1.000000000000000000, 0.000000000000000000 ) ) ;
#17234 = CARTESIAN_POINT ( 'NONE',  ( 4.261015134245454306, -92.86276748796085201, -30.20116777978838840 ) ) ;
#17235 = CARTESIAN_POINT ( 'NONE',  ( -3.215500929169999633, -94.59276292389999696, 23.57860676330000160 ) ) ;
#17236 = ORIENTED_EDGE ( 'NONE', *, *, #1428, .F. ) ;
#17237 = TOROIDAL_SURFACE ( 'NONE', #8377, 55.85192378860000417, 0.3499999999999999778 ) ;
#17238 = CARTESIAN_POINT ( 'NONE',  ( 7.993247198980000690, -93.67384740779999674, -24.35792768219999971 ) ) ;
#17239 = AXIS2_PLACEMENT_3D ( 'NONE', #27856, #11835, #14590 ) ;
#17240 = EDGE_CURVE ( 'NONE', #5855, #9315, #20027, .T. ) ;
#17241 = CIRCLE ( 'NONE', #18188, 7.000000000000000000 ) ;
#17242 = CARTESIAN_POINT ( 'NONE',  ( 20.94292112449999976, -31.57154123859999473, -8.118247248619999468 ) ) ;
#17243 = CARTESIAN_POINT ( 'NONE',  ( 6.708131455446116220, -101.3586211801433166, 14.77255361321039118 ) ) ;
#17244 = DIRECTION ( 'NONE',  ( 0.4794255386042040601, 0.000000000000000000, 0.8775825618903722036 ) ) ;
#17245 = EDGE_LOOP ( 'NONE', ( #3513, #18526, #27657, #23442 ) ) ;
#17246 = CARTESIAN_POINT ( 'NONE',  ( -40.00000000000000000, -82.25000000000000000, 0.000000000000000000 ) ) ;
#17247 = CARTESIAN_POINT ( 'NONE',  ( -12.52732263940944435, -101.0610180771033413, -10.67209290993696236 ) ) ;
#17248 = ORIENTED_EDGE ( 'NONE', *, *, #23702, .T. ) ;
#17249 = CARTESIAN_POINT ( 'NONE',  ( 25.70121108570000246, -93.05538536790000137, -5.710191390220000329 ) ) ;
#17250 = CARTESIAN_POINT ( 'NONE',  ( -0.8149835146670000308, -101.1716782080000030, -15.71308785760000148 ) ) ;
#17251 = CARTESIAN_POINT ( 'NONE',  ( 21.55856599210000013, -18.50000000000000000, 0.6626745995510000542 ) ) ;
#17252 = DIRECTION ( 'NONE',  ( 1.000000000000000000, 0.000000000000000000, 0.000000000000000000 ) ) ;
#17253 = DIRECTION ( 'NONE',  ( 0.8775825618903722036, 0.000000000000000000, -0.4794255386042041156 ) ) ;
#17254 = CARTESIAN_POINT ( 'NONE',  ( 16.02651611377384810, -94.78494200512166401, 17.25365316566084672 ) ) ;
#17255 = CARTESIAN_POINT ( 'NONE',  ( -22.76595506760000021, -72.55114968140000542, 17.38101673350000098 ) ) ;
#17256 = CARTESIAN_POINT ( 'NONE',  ( 26.40471317329472711, -92.73901256243104285, 13.20493500560145073 ) ) ;
#17257 = CARTESIAN_POINT ( 'NONE',  ( -19.73459501710000197, -19.50000000000000000, 14.41863426819999994 ) ) ;
#17258 = DIRECTION ( 'NONE',  ( 0.000000000000000000, -1.000000000000000000, 0.000000000000000000 ) ) ;
#17259 = CARTESIAN_POINT ( 'NONE',  ( 24.43683151600445314, -93.86130746219269838, -9.930393139660877111 ) ) ;
#17260 = FACE_BOUND ( 'NONE', #14999, .T. ) ;
#17261 = AXIS2_PLACEMENT_3D ( 'NONE', #22504, #22647, #5003 ) ;
#17262 = VERTEX_POINT ( 'NONE', #18243 ) ;
#17263 = VECTOR ( 'NONE', #7575, 999.9999999999998863 ) ;
#17264 = AXIS2_PLACEMENT_3D ( 'NONE', #15121, #21289, #10189 ) ;
#17265 = DIRECTION ( 'NONE',  ( 0.9988549560444618391, 0.000000000000000000, 0.04784116204082212997 ) ) ;
#17266 = CIRCLE ( 'NONE', #2853, 6.749999999999999112 ) ;
#17267 = ORIENTED_EDGE ( 'NONE', *, *, #24990, .T. ) ;
#17268 = AXIS2_PLACEMENT_3D ( 'NONE', #12332, #28349, #27936 ) ;
#17269 = CARTESIAN_POINT ( 'NONE',  ( 5.326862811529999898E-15, -69.50000000000000000, -47.25000000000000000 ) ) ;
#17270 = EDGE_CURVE ( 'NONE', #22334, #13365, #7031, .T. ) ;
#17271 = VERTEX_POINT ( 'NONE', #25097 ) ;
#17272 = CARTESIAN_POINT ( 'NONE',  ( -1.084625078730000025, -65.04696937989999128, -25.11520914390000314 ) ) ;
#17273 = CARTESIAN_POINT ( 'NONE',  ( -25.18134011720000132, -94.15497152599999708, -3.050188418449999883 ) ) ;
#17274 = CARTESIAN_POINT ( 'NONE',  ( 0.000000000000000000, -110.0000000000000000, 0.000000000000000000 ) ) ;
#17275 = ADVANCED_FACE ( 'NONE', ( #22472 ), #25492, .F. ) ;
#17276 =( GEOMETRIC_REPRESENTATION_CONTEXT ( 3 ) GLOBAL_UNCERTAINTY_ASSIGNED_CONTEXT ( ( #10594 ) ) GLOBAL_UNIT_ASSIGNED_CONTEXT ( ( #1392, #27764, #23108 ) ) REPRESENTATION_CONTEXT ( 'NONE', 'WORKASPACE' ) );
#17277 = ORIENTED_EDGE ( 'NONE', *, *, #10056, .F. ) ;
#17278 = DIRECTION ( 'NONE',  ( -0.9295286103719511139, 0.000000000000000000, -0.3687499999999862554 ) ) ;
#17279 = CARTESIAN_POINT ( 'NONE',  ( -12.29363612059999866, -101.2530993000000024, -8.928690578620001261 ) ) ;
#17280 = ORIENTED_EDGE ( 'NONE', *, *, #18763, .T. ) ;
#17281 = AXIS2_PLACEMENT_3D ( 'NONE', #24095, #24247, #4430 ) ;
#17282 = DIRECTION ( 'NONE',  ( 0.000000000000000000, -1.000000000000000000, 0.000000000000000000 ) ) ;
#17283 = TOROIDAL_SURFACE ( 'NONE', #15380, 33.64999999999999858, 1.250000000000000000 ) ;
#17284 = VECTOR ( 'NONE', #4368, 1000.000000000000000 ) ;
#17285 = CARTESIAN_POINT ( 'NONE',  ( -22.22906645665673153, -74.41344022149685600, -32.83566817454327946 ) ) ;
#17286 = CARTESIAN_POINT ( 'NONE',  ( 22.35420149509999987, -19.50000008899999671, 9.881343242109998926 ) ) ;
#17287 = CARTESIAN_POINT ( 'NONE',  ( -32.58054283434451293, -74.15589285242916162, -22.16749819904017826 ) ) ;
#17288 = CARTESIAN_POINT ( 'NONE',  ( -19.63525383109999822, -57.47122600979999874, 13.01113855729999891 ) ) ;
#17289 = B_SPLINE_SURFACE_WITH_KNOTS ( 'NONE', 5, 5, ( 
 ( #26600, #6643, #15505, #4014, #20038, #24414, #21788, #1844, #9684 ),
 ( #20186, #9548, #18596, #14223, #22534, #4747, #13771, #26901, #13921 ),
 ( #22822, #22673, #13626, #5185, #24997, #15952, #2576, #2865, #11425 ),
 ( #20326, #2717, #399, #9246, #261, #27192, #9100, #18004, #11281 ),
 ( #15803, #696, #11725, #24711, #4892, #18148, #11571, #27045, #20481 ),
 ( #549, #9395, #16394, #7232, #18302, #16097, #20640, #7088, #24857 ) ),
 .UNSPECIFIED., .F., .F., .F.,
 ( 6, 6 ),
 ( 6, 3, 6 ),
 ( 10.27983419550000121, 28.98451109730000042 ),
 ( 0.000000000000000000, 0.2500000000000000000, 0.5000000000000000000 ),
 .UNSPECIFIED. ) ;
#17290 = ADVANCED_FACE ( 'NONE', ( #19233 ), #3494, .T. ) ;
#17291 = ORIENTED_EDGE ( 'NONE', *, *, #5008, .T. ) ;
#17292 = CARTESIAN_POINT ( 'NONE',  ( 0.000000000000000000, -15.80000000000000071, 0.000000000000000000 ) ) ;
#17293 = CARTESIAN_POINT ( 'NONE',  ( -12.06953548060000081, -101.1411470200000053, -9.548139877839998846 ) ) ;
#17294 = CARTESIAN_POINT ( 'NONE',  ( -7.522398661245357054, -101.1884902308600118, 14.52463055899669087 ) ) ;
#17295 = EDGE_LOOP ( 'NONE', ( #12594, #382, #23362, #28201 ) ) ;
#17296 = AXIS2_PLACEMENT_3D ( 'NONE', #6201, #26318, #20040 ) ;
#17297 = DIRECTION ( 'NONE',  ( 0.000000000000000000, 1.000000000000000000, 0.000000000000000000 ) ) ;
#17298 = CARTESIAN_POINT ( 'NONE',  ( -32.78146620020000057, -74.32000120609998817, -22.21606701669999850 ) ) ;
#17299 = CARTESIAN_POINT ( 'NONE',  ( -22.39529575027539110, -79.87460703810864970, -32.76478017285002409 ) ) ;
#17300 = ORIENTED_EDGE ( 'NONE', *, *, #1716, .F. ) ;
#17301 = AXIS2_PLACEMENT_3D ( 'NONE', #5688, #16486, #20870 ) ;
#17302 = EDGE_CURVE ( 'NONE', #18220, #25027, #5690, .T. ) ;
#17303 = EDGE_CURVE ( 'NONE', #20739, #16026, #250, .T. ) ;
#17304 = CYLINDRICAL_SURFACE ( 'NONE', #16750, 0.5000000000000012212 ) ;
#17305 = DIRECTION ( 'NONE',  ( 0.000000000000000000, -1.000000000000000000, 0.000000000000000000 ) ) ;
#17306 = ORIENTED_EDGE ( 'NONE', *, *, #11110, .T. ) ;
#17307 = DIRECTION ( 'NONE',  ( 0.000000000000000000, -1.000000000000000000, 0.000000000000000000 ) ) ;
#17308 = VERTEX_POINT ( 'NONE', #1211 ) ;
#17309 = CARTESIAN_POINT ( 'NONE',  ( 20.38362048469999976, -53.84434310259999279, 11.15071595380000069 ) ) ;
#17310 = DIRECTION ( 'NONE',  ( 0.000000000000000000, -1.000000000000000000, 0.000000000000000000 ) ) ;
#17311 = CARTESIAN_POINT ( 'NONE',  ( 1.631276547419999945, -94.59276292389999696, 23.74086995720000104 ) ) ;
#17312 = ORIENTED_EDGE ( 'NONE', *, *, #4606, .F. ) ;
#17313 = CARTESIAN_POINT ( 'NONE',  ( 0.000000000000000000, -29.89689110870000022, 0.000000000000000000 ) ) ;
#17314 = PLANE ( 'NONE',  #11274 ) ;
#17315 = AXIS2_PLACEMENT_3D ( 'NONE', #15353, #24269, #4309 ) ;
#17316 = CARTESIAN_POINT ( 'NONE',  ( -29.47186832370000076, -93.00000450890000536, -0.4149655844399999793 ) ) ;
#17317 = CARTESIAN_POINT ( 'NONE',  ( -18.81974815339999907, -92.68289710869998999, -20.86662628930000096 ) ) ;
#17318 = CIRCLE ( 'NONE', #8472, 8.099999999999999645 ) ;
#17319 = CARTESIAN_POINT ( 'NONE',  ( 25.56573787435306144, -68.11428155215978109, 10.87001957151865383 ) ) ;
#17320 = ORIENTED_EDGE ( 'NONE', *, *, #26448, .T. ) ;
#17321 = CARTESIAN_POINT ( 'NONE',  ( -20.51325115670000443, -95.66919271829999616, -9.269412113539999609 ) ) ;
#17322 = CARTESIAN_POINT ( 'NONE',  ( 12.01586610120000032, -101.1700440390000040, -9.474730661679998889 ) ) ;
#17323 = CARTESIAN_POINT ( 'NONE',  ( 0.000000000000000000, -26.90310889129999694, 0.000000000000000000 ) ) ;
#17324 = EDGE_CURVE ( 'NONE', #16038, #13829, #15570, .T. ) ;
#17325 = DIRECTION ( 'NONE',  ( 0.4794255386042040601, 0.000000000000000000, 0.8775825618903720926 ) ) ;
#17326 = ADVANCED_FACE ( 'NONE', ( #1338 ), #3791, .F. ) ;
#17327 = CARTESIAN_POINT ( 'NONE',  ( 11.65689279962786884, -72.11966578858674382, -27.17683449633075554 ) ) ;
#17328 = CARTESIAN_POINT ( 'NONE',  ( -38.25000000000000000, -65.56519245710001087, -1.769653913539999790 ) ) ;
#17329 = ORIENTED_EDGE ( 'NONE', *, *, #17432, .F. ) ;
#17330 = CARTESIAN_POINT ( 'NONE',  ( 0.000000000000000000, -12.64149019679999952, 0.000000000000000000 ) ) ;
#17331 = CARTESIAN_POINT ( 'NONE',  ( -2.664535259099999805E-15, -101.6484611540000031, 1.776356839399999804E-15 ) ) ;
#17332 = CARTESIAN_POINT ( 'NONE',  ( 21.67693832783029961, -96.57210917632126268, 0.1672311650303546227 ) ) ;
#17333 = CARTESIAN_POINT ( 'NONE',  ( 27.68682485439999752, -21.50000000000000000, 50.68039294919999804 ) ) ;
#17334 = EDGE_CURVE ( 'NONE', #5555, #15327, #2523, .T. ) ;
#17335 = CARTESIAN_POINT ( 'NONE',  ( -0.2442174124554105097, -92.66191076887825773, -30.49908852203764198 ) ) ;
#17336 = SHAPE_REPRESENTATION_RELATIONSHIP ( 'NONE' , 'NONE' ,  #19699, #5353 ) ;
#17337 = TOROIDAL_SURFACE ( 'NONE', #4318, 6.750000000000000000, 0.5000000000000000000 ) ;
#17338 = DIRECTION ( 'NONE',  ( 0.000000000000000000, 1.000000000000000000, 0.000000000000000000 ) ) ;
#17339 = TOROIDAL_SURFACE ( 'NONE', #146, 21.03431122519999974, 1.000000000000000000 ) ;
#17340 = FACE_OUTER_BOUND ( 'NONE', #22846, .T. ) ;
#17341 = ORIENTED_EDGE ( 'NONE', *, *, #1993, .T. ) ;
#17342 = CARTESIAN_POINT ( 'NONE',  ( 21.26288536570000076, -97.23151480340000319, -2.165621899160000030 ) ) ;
#17343 = VERTEX_POINT ( 'NONE', #17045 ) ;
#17344 = CARTESIAN_POINT ( 'NONE',  ( 21.52213036419999881, -37.12342612100000139, -7.869482006920000217 ) ) ;
#17345 = DIRECTION ( 'NONE',  ( 1.000000000000000000, 0.000000000000000000, 0.000000000000000000 ) ) ;
#17346 = ORIENTED_EDGE ( 'NONE', *, *, #11744, .T. ) ;
#17347 = CARTESIAN_POINT ( 'NONE',  ( -13.05440433799999944, -101.3957169669999985, -9.227549938650001948 ) ) ;
#17348 = B_SPLINE_SURFACE_WITH_KNOTS ( 'NONE', 5, 5, ( 
 ( #19230, #5687, #3644, #1073, #12508, #20868 ),
 ( #27715, #8155, #25932, #5955, #11956, #27981 ),
 ( #25516, #1334, #928, #3514, #16620, #18956 ),
 ( #14437, #12097, #23328, #1476, #14839, #27839 ),
 ( #21010, #23193, #7884, #7621, #9913, #16763 ),
 ( #25658, #12370, #7757, #14569, #23474, #21278 ) ),
 .UNSPECIFIED., .F., .F., .F.,
 ( 6, 6 ),
 ( 6, 6 ),
 ( 3.704386147560000175, 9.195309357930000260 ),
 ( 0.000000000000000000, 0.5000000000000000000 ),
 .UNSPECIFIED. ) ;
#17349 = DIRECTION ( 'NONE',  ( -0.000000000000000000, 1.000000000000000000, 0.000000000000000000 ) ) ;
#17350 = CARTESIAN_POINT ( 'NONE',  ( -0.1520325283909999825, -93.05538537019999978, 26.32746518160000093 ) ) ;
#17351 = AXIS2_PLACEMENT_3D ( 'NONE', #13902, #18724, #4877 ) ;
#17352 = CARTESIAN_POINT ( 'NONE',  ( -30.37538215883989068, -92.92035259800012170, 2.768038011894732087 ) ) ;
#17353 = CARTESIAN_POINT ( 'NONE',  ( 9.427231679889999327, -53.23790003359999901, -23.11289036089999982 ) ) ;
#17354 = LINE ( 'NONE', #23911, #10171 ) ;
#17355 = DIRECTION ( 'NONE',  ( 0.000000000000000000, -1.000000000000000000, 0.000000000000000000 ) ) ;
#17356 = EDGE_LOOP ( 'NONE', ( #16487, #11426, #6493, #27120 ) ) ;
#17357 = CARTESIAN_POINT ( 'NONE',  ( 13.06668678909421111, -101.2021794473205603, -9.821573571294250016 ) ) ;
#17358 = CARTESIAN_POINT ( 'NONE',  ( 24.30550941250000108, -42.22519323649999734, 1.361066622060000064 ) ) ;
#17359 = CARTESIAN_POINT ( 'NONE',  ( 23.10489107149999910, -66.56254540410000686, 11.55379042880000107 ) ) ;
#17360 = CARTESIAN_POINT ( 'NONE',  ( 0.000000000000000000, -13.50000000000000000, 0.000000000000000000 ) ) ;
#17361 = ORIENTED_EDGE ( 'NONE', *, *, #20069, .T. ) ;
#17362 = CIRCLE ( 'NONE', #4813, 7.000000000000000000 ) ;
#17363 = CARTESIAN_POINT ( 'NONE',  ( -2.080583445478223936, -64.78278821048890279, -25.39005510556196654 ) ) ;
#17364 = FACE_OUTER_BOUND ( 'NONE', #16263, .T. ) ;
#17365 = CARTESIAN_POINT ( 'NONE',  ( -20.54393874204836123, -94.23729456146304528, 12.90813503536128692 ) ) ;
#17366 = VERTEX_POINT ( 'NONE', #12648 ) ;
#17367 = EDGE_CURVE ( 'NONE', #3493, #11457, #12100, .T. ) ;
#17368 = DIRECTION ( 'NONE',  ( 0.000000000000000000, -1.000000000000000000, 0.000000000000000000 ) ) ;
#17369 = CARTESIAN_POINT ( 'NONE',  ( 1.057205864080000168, -100.1340845430000002, -16.60558664359999881 ) ) ;
#17370 = CARTESIAN_POINT ( 'NONE',  ( 22.95932595720000080, -57.43039249360000298, -9.307783803350000440 ) ) ;
#17371 = CARTESIAN_POINT ( 'NONE',  ( -12.07714908089999994, -67.83051071330000070, -24.91356169369999662 ) ) ;
#17372 = EDGE_CURVE ( 'NONE', #7997, #10981, #21281, .T. ) ;
#17373 = CARTESIAN_POINT ( 'NONE',  ( -29.41275679339999982, -37.50000000000000000, -53.83969017199999740 ) ) ;
#17374 = CARTESIAN_POINT ( 'NONE',  ( 24.78974499519999952, -64.24504771300000527, -10.08507930170000044 ) ) ;
#17375 = ORIENTED_EDGE ( 'NONE', *, *, #5206, .T. ) ;
#17376 = ADVANCED_FACE ( 'NONE', ( #25935 ), #25662, .T. ) ;
#17377 = CARTESIAN_POINT ( 'NONE',  ( 6.475617225940000665, -101.0151300849999814, 14.23442573650000043 ) ) ;
#17378 = CARTESIAN_POINT ( 'NONE',  ( -16.36884634468729516, -92.53775804172235553, -23.99411788281411972 ) ) ;
#17379 = VECTOR ( 'NONE', #21345, 999.9999999999998863 ) ;
#17380 = EDGE_LOOP ( 'NONE', ( #5624, #16303, #19720, #4473 ) ) ;
#17381 = CARTESIAN_POINT ( 'NONE',  ( -40.28469781717293330, -65.70975255743327637, -2.216737453835613714 ) ) ;
#17382 = CARTESIAN_POINT ( 'NONE',  ( 4.396272035099083375, -92.82529299094557018, -30.18149772317508805 ) ) ;
#17383 = CARTESIAN_POINT ( 'NONE',  ( 7.250053749315197749, -74.39269056243638545, 40.35493623771126437 ) ) ;
#17384 = ORIENTED_EDGE ( 'NONE', *, *, #1297, .F. ) ;
#17385 = AXIS2_PLACEMENT_3D ( 'NONE', #28282, #23921, #8314 ) ;
#17386 = CARTESIAN_POINT ( 'NONE',  ( 3.408291041020000467, -92.96321827540000982, -28.95142855790000169 ) ) ;
#17387 = CARTESIAN_POINT ( 'NONE',  ( 6.788846616428737768, -101.5026031440148842, 14.61257718564415242 ) ) ;
#17388 = CARTESIAN_POINT ( 'NONE',  ( -6.708539788989999586, -101.2358105800000061, 13.65871639999999942 ) ) ;
#17389 = ORIENTED_EDGE ( 'NONE', *, *, #6138, .T. ) ;
#17390 = CARTESIAN_POINT ( 'NONE',  ( -5.813199663199999812, -6.776234273679999198, -10.64099060729999913 ) ) ;
#17391 = CARTESIAN_POINT ( 'NONE',  ( -12.77330844608892590, -100.5798851005997676, -10.97038188722230956 ) ) ;
#17392 = VERTEX_POINT ( 'NONE', #14573 ) ;
#17393 = CARTESIAN_POINT ( 'NONE',  ( 8.071123906760000466, -36.85053012899999914, -21.46851019590000220 ) ) ;
#17394 = CARTESIAN_POINT ( 'NONE',  ( 24.71295097499999827, -93.67869433800001389, -3.805954965999999828 ) ) ;
#17395 = FACE_OUTER_BOUND ( 'NONE', #17213, .T. ) ;
#17396 = CIRCLE ( 'NONE', #5311, 20.64285714289999873 ) ;
#17397 = B_SPLINE_CURVE_WITH_KNOTS ( 'NONE', 3,
 ( #5456, #14339, #23232, #22806 ),
 .UNSPECIFIED., .F., .F.,
 ( 4, 4 ),
 ( -7.329014384030000606, -6.713731535029999975 ),
 .UNSPECIFIED. ) ;
#17398 = CARTESIAN_POINT ( 'NONE',  ( 22.56104036090000164, -19.46971296670000129, 0.9632387859859999901 ) ) ;
#17399 = CARTESIAN_POINT ( 'NONE',  ( -7.318371247189999984, -73.93831524339999817, 38.68350846249999364 ) ) ;
#17400 = AXIS2_PLACEMENT_3D ( 'NONE', #27943, #10546, #3603 ) ;
#17401 = DIRECTION ( 'NONE',  ( 0.000000000000000000, 1.000000000000000000, 0.000000000000000000 ) ) ;
#17402 = EDGE_LOOP ( 'NONE', ( #11941, #5131, #13977, #27353 ) ) ;
#17403 = DIRECTION ( 'NONE',  ( 0.000000000000000000, -1.000000000000000000, 0.000000000000000000 ) ) ;
#17404 = B_SPLINE_CURVE_WITH_KNOTS ( 'NONE', 5,
 ( #16292, #14672, #27382, #12337, #1036, #7580 ),
 .UNSPECIFIED., .F., .F.,
 ( 6, 6 ),
 ( 0.000000000000000000, 1.000000000000000000 ),
 .UNSPECIFIED. ) ;
#17405 = CARTESIAN_POINT ( 'NONE',  ( 29.52540673129999860, -93.00000000000000000, 7.168153169610000930 ) ) ;
#17406 = EDGE_CURVE ( 'NONE', #15088, #24436, #11326, .T. ) ;
#17407 = CARTESIAN_POINT ( 'NONE',  ( 9.334872109610000362E-16, -74.00000000000000000, -2.419703924680000090E-15 ) ) ;
#17408 = CARTESIAN_POINT ( 'NONE',  ( 36.28420073633509446, -75.00000019211667279, -14.96759456046001091 ) ) ;
#17409 = FACE_OUTER_BOUND ( 'NONE', #23825, .T. ) ;
#17410 = CARTESIAN_POINT ( 'NONE',  ( -24.15516222759999820, -94.98812477599999227, -4.102682929219999330 ) ) ;
#17411 = VECTOR ( 'NONE', #25092, 1000.000000000000000 ) ;
#17412 = CARTESIAN_POINT ( 'NONE',  ( 23.69519146889223649, -94.79128788265268213, -7.184658344615285408 ) ) ;
#17413 = DIRECTION ( 'NONE',  ( 1.000000000000000000, 0.000000000000000000, 0.000000000000000000 ) ) ;
#17414 = ORIENTED_EDGE ( 'NONE', *, *, #10853, .T. ) ;
#17415 = EDGE_CURVE ( 'NONE', #10810, #4274, #3891, .T. ) ;
#17416 = CARTESIAN_POINT ( 'NONE',  ( 7.924293243680000209, -18.50000000000000000, -19.29218481000000196 ) ) ;
#17417 = CARTESIAN_POINT ( 'NONE',  ( 21.62249394079999831, -36.00000000000000000, -10.68317415409999960 ) ) ;
#17418 = CARTESIAN_POINT ( 'NONE',  ( -2.578021201719999933, -61.45046333410000017, -25.33276682509999844 ) ) ;
#17419 = CIRCLE ( 'NONE', #21161, 39.25000000000000000 ) ;
#17420 = B_SPLINE_CURVE_WITH_KNOTS ( 'NONE', 5,
 ( #4395, #13263, #6281, #17216, #17363, #12963, #4244, #8888, #17801 ),
 .UNSPECIFIED., .F., .F.,
 ( 6, 3, 6 ),
 ( 0.000000000000000000, 0.5000000000000000000, 1.000000000000000000 ),
 .UNSPECIFIED. ) ;
#17421 = LINE ( 'NONE', #1983, #15778 ) ;
#17422 = CARTESIAN_POINT ( 'NONE',  ( 0.000000000000000000, -14.00000000000000000, 0.000000000000000000 ) ) ;
#17423 = DIRECTION ( 'NONE',  ( 1.000000000000000000, 0.000000000000000000, 0.000000000000000000 ) ) ;
#17424 = ORIENTED_EDGE ( 'NONE', *, *, #14512, .T. ) ;
#17425 = CARTESIAN_POINT ( 'NONE',  ( 21.19938064309999959, -34.67919421940000291, -7.731040044549999379 ) ) ;
#17426 = DIRECTION ( 'NONE',  ( 0.05900121837168382372, 0.000000000000000000, 0.9982579106777251798 ) ) ;
#17427 = ORIENTED_EDGE ( 'NONE', *, *, #20155, .F. ) ;
#17428 = AXIS2_PLACEMENT_3D ( 'NONE', #2256, #11102, #8934 ) ;
#17429 = DIRECTION ( 'NONE',  ( 0.000000000000000000, 1.000000000000000000, 0.000000000000000000 ) ) ;
#17430 = CIRCLE ( 'NONE', #9509, 9.500000000000000000 ) ;
#17431 = CARTESIAN_POINT ( 'NONE',  ( 21.40964882759999810, -19.42987840509999842, 9.433029012200000452 ) ) ;
#17432 = EDGE_CURVE ( 'NONE', #10427, #8854, #9000, .T. ) ;
#17433 = CARTESIAN_POINT ( 'NONE',  ( -22.19729432756942700, -74.24324329339850692, -32.70355094814552643 ) ) ;
#17434 = ADVANCED_FACE ( 'NONE', ( #16488 ), #27718, .T. ) ;
#17435 = CARTESIAN_POINT ( 'NONE',  ( -14.89662347129999986, -101.1848541720000014, 3.414158506610000199 ) ) ;
#17436 = CARTESIAN_POINT ( 'NONE',  ( -32.71258333431942589, -74.25151540671238592, -22.19947060199589828 ) ) ;
#17437 = CARTESIAN_POINT ( 'NONE',  ( -13.16239993169999956, -100.8816835080000089, -8.729908192910000864 ) ) ;
#17438 = VERTEX_POINT ( 'NONE', #25520 ) ;
#17439 = AXIS2_PLACEMENT_3D ( 'NONE', #25699, #16949, #3823 ) ;
#17440 = DIRECTION ( 'NONE',  ( 1.000000000000000000, 0.000000000000000000, 0.000000000000000000 ) ) ;
#17441 = CARTESIAN_POINT ( 'NONE',  ( -11.80853318720000011, -100.8815367389999977, -10.30796059140000054 ) ) ;
#17442 = CARTESIAN_POINT ( 'NONE',  ( -22.83401285485959065, -72.59721320750036000, 17.30277226862465412 ) ) ;
#17443 = CARTESIAN_POINT ( 'NONE',  ( -7.762847924256437437, -100.8061861225939708, 14.73824615606121746 ) ) ;
#17444 = ORIENTED_EDGE ( 'NONE', *, *, #3812, .F. ) ;
#17445 = EDGE_CURVE ( 'NONE', #2579, #5717, #12373, .T. ) ;
#17446 = B_SPLINE_CURVE_WITH_KNOTS ( 'NONE', 3,
 ( #23592, #16754, #12363, #3636, #1064, #1466 ),
 .UNSPECIFIED., .F., .F.,
 ( 4, 2, 4 ),
 ( 0.000000000000000000, 0.5000000000000000000, 1.000000000000000000 ),
 .UNSPECIFIED. ) ;
#17447 = DIRECTION ( 'NONE',  ( -0.000000000000000000, 1.000000000000000000, 0.000000000000000000 ) ) ;
#17448 = CARTESIAN_POINT ( 'NONE',  ( -32.54298110219999529, -74.18397341870000616, -22.08462029819999728 ) ) ;
#17449 = CARTESIAN_POINT ( 'NONE',  ( -10.63276174549836917, -93.28923452009620121, -23.66442649163524337 ) ) ;
#17450 = ORIENTED_EDGE ( 'NONE', *, *, #28485, .F. ) ;
#17451 = DIRECTION ( 'NONE',  ( 1.000000000000000000, 0.000000000000000000, 0.000000000000000000 ) ) ;
#17452 = CYLINDRICAL_SURFACE ( 'NONE', #21306, 5.999999999999999112 ) ;
#17453 = B_SPLINE_CURVE_WITH_KNOTS ( 'NONE', 3,
 ( #3771, #8408, #10030, #21684, #3908, #1195, #23315, #12491, #12774, #1462, #27827, #1731, #10572, #10303, #28232, #23589, #19487 ),
 .UNSPECIFIED., .F., .F.,
 ( 4, 2, 2, 1, 1, 1, 1, 1, 2, 2, 4 ),
 ( 0.000000000000000000, 0.2500000000000092149, 0.3750000000000130451, 0.4375000000000158762, 0.4687500000000175970, 0.4843750000000193179, 0.4921875000000209832, 0.4960937500000218159, 0.4980468750000214273, 0.5000000000000209832, 1.000000000000000000 ),
 .UNSPECIFIED. ) ;
#17454 = ORIENTED_EDGE ( 'NONE', *, *, #21515, .F. ) ;
#17455 = CARTESIAN_POINT ( 'NONE',  ( -17.16748885897166943, -93.45279863366459949, -21.41968775130273528 ) ) ;
#17456 = ORIENTED_EDGE ( 'NONE', *, *, #26258, .F. ) ;
#17457 = CARTESIAN_POINT ( 'NONE',  ( 24.24773784319999947, -93.39359559929999932, 12.30290705160000009 ) ) ;
#17458 = LINE ( 'NONE', #19772, #18594 ) ;
#17459 = ORIENTED_EDGE ( 'NONE', *, *, #18934, .F. ) ;
#17460 = CARTESIAN_POINT ( 'NONE',  ( 21.33676308416200129, -18.50000000000000000, -0.4490900276398021584 ) ) ;
#17461 = CARTESIAN_POINT ( 'NONE',  ( -21.85457013290000106, -79.50000016359999222, -32.66023313979999187 ) ) ;
#17462 = CARTESIAN_POINT ( 'NONE',  ( -2.583988331150000040, -57.40875702419999982, -25.23271569440000306 ) ) ;
#17463 = CARTESIAN_POINT ( 'NONE',  ( 8.793944060959999476, -36.72282064609999708, -21.68248837259999817 ) ) ;
#17464 = CARTESIAN_POINT ( 'NONE',  ( -20.32909851670000378, -92.54030566109999256, -20.27308962609999909 ) ) ;
#17465 = CARTESIAN_POINT ( 'NONE',  ( -3.641273963749999787, -18.50000000000000000, -23.80755169360000068 ) ) ;
#17466 = ORIENTED_EDGE ( 'NONE', *, *, #24925, .F. ) ;
#17467 = CARTESIAN_POINT ( 'NONE',  ( -6.126542658125574192, -101.6174239712916432, 14.80565200955684801 ) ) ;
#17468 = ADVANCED_FACE ( 'NONE', ( #5556 ), #25326, .F. ) ;
#17469 = CARTESIAN_POINT ( 'NONE',  ( 13.64192749750000111, -100.1340845430000002, -9.526857098169999816 ) ) ;
#17470 = CARTESIAN_POINT ( 'NONE',  ( 23.97433219293744955, -62.13475794617575332, -0.5610772764335347773 ) ) ;
#17471 = CARTESIAN_POINT ( 'NONE',  ( -5.731166642400647326, -98.21052819054347083, -19.47007456258096170 ) ) ;
#17472 = CLOSED_SHELL ( 'NONE', ( #14577, #7057, #1804, #1664, #16121, #3881, #26679, #17741, #9960, #16685, #28635, #28399, #7219, #14666, #5402, #391, #1784, #24098, #24615, #2912, #15071, #8723, #6885, #12925, #9415, #11542, #10461, #27027, #6554, #28374, #22290, #4310, #24544, #12203, #15132, #20648, #28064, #22585, #16641, #20723, #1589, #8332, #6479, #27724, #571, #10206, #28095, #1216, #21008, #9465, #18103, #28532, #7362, #11917, #1693, #8939, #10218, #5603, #23185, #16451, #5886, #13340, #20191, #21356, #8269, #12825, #9339, #1076, #4983, #22818, #26884, #24617, #17275, #5215, #25303, #19144, #9241, #21615, #2123, #21454, #3157, #8433, #23953, #25427, #3149, #5699, #12552, #27686, #16218, #27089, #12359, #772, #15226, #8347, #24970, #23612, #16784, #14913, #6143, #17693, #14164, #25854, #11883, #4542, #2452, #17522, #7788, #11708, #24651, #1564, #22009, #3613, #17812, #17044, #26723, #22483, #16499, #21642, #3125, #26079, #24137, #13308, #27758, #22168, #12107, #8233, #28334, #7846, #25231, #7998, #11463, #23792, #9231, #20336, #20618, #23821, #13535, #6302, #26748, #27808, #24507, #14612, #28126, #6828, #10751, #18041, #4851, #17434, #10498, #2420, #11378, #15809, #7675, #12797, #26223, #25475 ) ) ;
#17473 = DIRECTION ( 'NONE',  ( 0.000000000000000000, -1.000000000000000000, 0.000000000000000000 ) ) ;
#17474 = CARTESIAN_POINT ( 'NONE',  ( 11.38494915445543754, -72.26806502549214883, -27.01670803782107910 ) ) ;
#17475 = CARTESIAN_POINT ( 'NONE',  ( -18.60684769790000104, -18.50000000000000000, 14.95957231910000118 ) ) ;
#17476 = ORIENTED_EDGE ( 'NONE', *, *, #6883, .F. ) ;
#17477 = DIRECTION ( 'NONE',  ( 0.000000000000000000, 1.000000000000000000, 0.000000000000000000 ) ) ;
#17478 = B_SPLINE_CURVE_WITH_KNOTS ( 'NONE', 5,
 ( #20262, #27125, #7466, #20561, #25083, #9325, #13851, #20719, #18229 ),
 .UNSPECIFIED., .F., .F.,
 ( 6, 3, 6 ),
 ( 0.000000000000000000, 1.237573681330000008, 1.566718891470000097 ),
 .UNSPECIFIED. ) ;
#17479 = DIRECTION ( 'NONE',  ( 0.4794255386042040601, 0.000000000000000000, 0.8775825618903720926 ) ) ;
#17480 = CARTESIAN_POINT ( 'NONE',  ( -23.91155634505533811, -92.72722989463423460, -18.93376855828962135 ) ) ;
#17481 = CARTESIAN_POINT ( 'NONE',  ( 8.862965437350000641, -35.80913068480000305, -20.41714882420000166 ) ) ;
#17482 = CARTESIAN_POINT ( 'NONE',  ( -39.50000000000000000, -65.63577453799999262, 2.309401076760000393 ) ) ;
#17483 = CARTESIAN_POINT ( 'NONE',  ( 40.00000000000000711, 0.000000000000000000, 40.00000000000000000 ) ) ;
#17484 = CARTESIAN_POINT ( 'NONE',  ( -31.64302845809999809, -74.50000000000000000, -31.64302845809999809 ) ) ;
#17485 = DIRECTION ( 'NONE',  ( 0.4794255386042041156, 0.000000000000000000, 0.8775825618903722036 ) ) ;
#17486 = ORIENTED_EDGE ( 'NONE', *, *, #12896, .T. ) ;
#17487 = EDGE_CURVE ( 'NONE', #22409, #24426, #15997, .T. ) ;
#17488 = CARTESIAN_POINT ( 'NONE',  ( 20.68906639099999722, -96.97547176279999803, -2.416818656099999796 ) ) ;
#17489 = ORIENTED_EDGE ( 'NONE', *, *, #21763, .F. ) ;
#17490 = CARTESIAN_POINT ( 'NONE',  ( 21.47403927899999587, -36.87897171440000221, -8.083288125820001113 ) ) ;
#17491 = DIRECTION ( 'NONE',  ( 0.000000000000000000, -1.000000000000000000, 0.000000000000000000 ) ) ;
#17492 = VERTEX_POINT ( 'NONE', #6699 ) ;
#17493 = CARTESIAN_POINT ( 'NONE',  ( 8.479935047972508855, -37.33301741675911245, -21.77931238865912533 ) ) ;
#17494 = CARTESIAN_POINT ( 'NONE',  ( -15.09559145619999931, -92.94652576229999852, -23.64540529880000008 ) ) ;
#17495 = ORIENTED_EDGE ( 'NONE', *, *, #3792, .F. ) ;
#17496 = CARTESIAN_POINT ( 'NONE',  ( -6.552399679369999674, -97.31350077540000143, -20.03651016279999908 ) ) ;
#17497 = CARTESIAN_POINT ( 'NONE',  ( 41.00000000000000000, -84.00000000000000000, -10.20110288159999890 ) ) ;
#17498 = FACE_OUTER_BOUND ( 'NONE', #25244, .T. ) ;
#17499 = CARTESIAN_POINT ( 'NONE',  ( -10.85800713629999947, -18.85488210659999808, -19.08173651049999719 ) ) ;
#17500 = AXIS2_PLACEMENT_3D ( 'NONE', #16842, #7395, #1145 ) ;
#17501 = CARTESIAN_POINT ( 'NONE',  ( -39.77149792059732647, -65.72204893723611008, 2.201677205306737495 ) ) ;
#17502 = VERTEX_POINT ( 'NONE', #4501 ) ;
#17503 = CARTESIAN_POINT ( 'NONE',  ( 13.27592836724310743, -100.9570234915505154, -9.862972498476620942 ) ) ;
#17504 = CARTESIAN_POINT ( 'NONE',  ( 22.83116343590000241, -42.27294335679999904, -0.2419517822940000229 ) ) ;
#17505 = CARTESIAN_POINT ( 'NONE',  ( 22.17951941979999830, -65.07442867339999282, 11.85657634389999870 ) ) ;
#17506 = DIRECTION ( 'NONE',  ( 1.000000000000000000, 0.000000000000000000, 0.000000000000000000 ) ) ;
#17507 = VERTEX_POINT ( 'NONE', #13084 ) ;
#17508 = CARTESIAN_POINT ( 'NONE',  ( 7.105427357599999217E-15, -69.00000000000000000, -40.00000000000000000 ) ) ;
#17509 = CARTESIAN_POINT ( 'NONE',  ( -14.11074263820000141, -92.49626986490000036, 25.91332334039999807 ) ) ;
#17510 = CARTESIAN_POINT ( 'NONE',  ( 10.50000000000000000, -89.00000000000000000, -1.981748098959999875E-14 ) ) ;
#17511 = ORIENTED_EDGE ( 'NONE', *, *, #23981, .T. ) ;
#17512 = DIRECTION ( 'NONE',  ( 0.4794255386042036160, 0.000000000000000000, 0.8775825618903723147 ) ) ;
#17513 = CARTESIAN_POINT ( 'NONE',  ( 0.8847930891630000350, -99.97545561319999763, -16.87691942780000076 ) ) ;
#17514 = CARTESIAN_POINT ( 'NONE',  ( 23.52264653552683527, -74.11875716583942619, -31.20127190410864770 ) ) ;
#17515 = CARTESIAN_POINT ( 'NONE',  ( -12.47539548249999974, -69.51716295290000858, -24.28999545310000130 ) ) ;
#17516 = LINE ( 'NONE', #20536, #25639 ) ;
#17517 = CARTESIAN_POINT ( 'NONE',  ( 22.76327770750000212, -62.13507791070000508, -7.555575355879999400 ) ) ;
#17518 = VERTEX_POINT ( 'NONE', #13231 ) ;
#17519 = CARTESIAN_POINT ( 'NONE',  ( 9.334872109610000362E-16, -74.00000000000000000, -2.419703924680000090E-15 ) ) ;
#17520 = CARTESIAN_POINT ( 'NONE',  ( -16.54020593362537639, -92.53069453552505763, -23.98110413831777521 ) ) ;
#17521 = ORIENTED_EDGE ( 'NONE', *, *, #27694, .F. ) ;
#17522 = ADVANCED_FACE ( 'NONE', ( #12927 ), #28391, .F. ) ;
#17523 = CARTESIAN_POINT ( 'NONE',  ( 27.89467015572686748, -92.52498922770504919, 12.33462672781183223 ) ) ;
#17524 = CARTESIAN_POINT ( 'NONE',  ( 5.818223828271644749, -92.52498922770502077, -29.94000519531349624 ) ) ;
#17525 = CARTESIAN_POINT ( 'NONE',  ( -5.605636395229999458, -96.73974214309998843, 20.49386430090000033 ) ) ;
#17526 = ORIENTED_EDGE ( 'NONE', *, *, #27781, .T. ) ;
#17527 = CARTESIAN_POINT ( 'NONE',  ( 7.854958299419999790, -93.60790942689999383, -24.22480680409999820 ) ) ;
#17528 = EDGE_CURVE ( 'NONE', #5350, #27002, #23204, .T. ) ;
#17529 = CARTESIAN_POINT ( 'NONE',  ( 6.838545786690161776, -101.5526869446500484, 14.54657801930438410 ) ) ;
#17530 = FACE_OUTER_BOUND ( 'NONE', #1101, .T. ) ;
#17531 = ORIENTED_EDGE ( 'NONE', *, *, #21224, .F. ) ;
#17532 = CARTESIAN_POINT ( 'NONE',  ( 0.000000000000000000, -107.5000000000000000, 0.000000000000000000 ) ) ;
#17533 = CARTESIAN_POINT ( 'NONE',  ( -12.48657657042820013, -101.1884902308936063, -10.56583077869183640 ) ) ;
#17534 = ORIENTED_EDGE ( 'NONE', *, *, #8341, .F. ) ;
#17535 = DIRECTION ( 'NONE',  ( 0.5301416321220552286, 0.000000000000000000, 0.8479091047340884257 ) ) ;
#17536 = EDGE_CURVE ( 'NONE', #10144, #26598, #27658, .T. ) ;
#17537 = DIRECTION ( 'NONE',  ( 1.000000000000000000, 0.000000000000000000, 0.000000000000000000 ) ) ;
#17538 = EDGE_CURVE ( 'NONE', #8283, #28554, #5445, .T. ) ;
#17539 = CARTESIAN_POINT ( 'NONE',  ( 12.32081986847368071, -94.36683344927988060, -21.27645860062538574 ) ) ;
#17540 = FACE_OUTER_BOUND ( 'NONE', #13663, .T. ) ;
#17541 = CARTESIAN_POINT ( 'NONE',  ( -7.196176986149999344, -73.81415963839999961, 38.70548920639999579 ) ) ;
#17542 = CARTESIAN_POINT ( 'NONE',  ( -20.95552429882483736, -92.86276748915979340, -22.16151589128406840 ) ) ;
#17543 = ORIENTED_EDGE ( 'NONE', *, *, #19763, .F. ) ;
#17544 = DIRECTION ( 'NONE',  ( 1.000000000000000000, 0.000000000000000000, 0.000000000000000000 ) ) ;
#17545 = CARTESIAN_POINT ( 'NONE',  ( -27.68682485439999752, -21.50000000000000000, -50.68039294919999804 ) ) ;
#17546 = CARTESIAN_POINT ( 'NONE',  ( 0.000000000000000000, -101.2530993010000060, 0.000000000000000000 ) ) ;
#17547 = CARTESIAN_POINT ( 'NONE',  ( -30.34790777679999962, -91.50000000000000000, 3.042119914239999723 ) ) ;
#17548 = CARTESIAN_POINT ( 'NONE',  ( 13.71624454005582905, -100.2392017794815189, -10.22880014236059054 ) ) ;
#17549 = CARTESIAN_POINT ( 'NONE',  ( -12.13283323140000114, -67.24447298400001216, -23.70109879609999837 ) ) ;
#17550 = CARTESIAN_POINT ( 'NONE',  ( 18.95948039760000015, -19.91448514760000066, -9.022805879459999900 ) ) ;
#17551 = ORIENTED_EDGE ( 'NONE', *, *, #28575, .T. ) ;
#17552 = CARTESIAN_POINT ( 'NONE',  ( 8.341252703189999451, -18.50000000000000000, -18.88171238309999822 ) ) ;
#17553 = CARTESIAN_POINT ( 'NONE',  ( -9.356041104380000917, -84.00000000000000000, -37.60355029590000697 ) ) ;
#17554 = AXIS2_PLACEMENT_3D ( 'NONE', #26422, #20294, #2388 ) ;
#17555 = EDGE_LOOP ( 'NONE', ( #25399, #26331, #9247, #21180 ) ) ;
#17556 = CARTESIAN_POINT ( 'NONE',  ( -12.91148099519999981, -61.97049086579999511, 20.77791015659999729 ) ) ;
#17557 = CARTESIAN_POINT ( 'NONE',  ( -24.42422992060000198, -94.22485739650001335, -3.548043453489999610 ) ) ;
#17558 = ADVANCED_FACE ( 'NONE', ( #4209 ), #13198, .T. ) ;
#17559 = AXIS2_PLACEMENT_3D ( 'NONE', #19100, #5961, #25808 ) ;
#17560 = CARTESIAN_POINT ( 'NONE',  ( -19.90265987359999755, -57.44036991819999827, 14.20824064939999865 ) ) ;
#17561 = EDGE_CURVE ( 'NONE', #14549, #28390, #4771, .T. ) ;
#17562 = CARTESIAN_POINT ( 'NONE',  ( 15.78891807579999984, -101.1191090859999946, 4.067324870920000279 ) ) ;
#17563 = VERTEX_POINT ( 'NONE', #11020 ) ;
#17564 = CARTESIAN_POINT ( 'NONE',  ( -20.93804484360220641, -95.75133630109712612, -8.863926826236266265 ) ) ;
#17565 = AXIS2_PLACEMENT_3D ( 'NONE', #4724, #17985, #9083 ) ;
#17566 = CARTESIAN_POINT ( 'NONE',  ( 7.196176986149999344, -73.81415963839999961, -38.70548920639999579 ) ) ;
#17567 = EDGE_LOOP ( 'NONE', ( #869, #5399, #12874, #20607 ) ) ;
#17568 = ADVANCED_FACE ( 'NONE', ( #19935 ), #1150, .F. ) ;
#17569 = CARTESIAN_POINT ( 'NONE',  ( 7.694334339803791778, -37.39019464809554449, -21.51655577991487078 ) ) ;
#17570 = EDGE_CURVE ( 'NONE', #13393, #6364, #24465, .T. ) ;
#17571 = CARTESIAN_POINT ( 'NONE',  ( -14.13580644329999991, -80.00000064429998758, 36.98348703120000636 ) ) ;
#17572 = CARTESIAN_POINT ( 'NONE',  ( 20.39668362470000318, -32.72716367860000020, 10.02066118239999959 ) ) ;
#17573 = DIRECTION ( 'NONE',  ( 1.000000000000000000, 0.000000000000000000, 0.000000000000000000 ) ) ;
#17574 = AXIS2_PLACEMENT_3D ( 'NONE', #1697, #21647, #6638 ) ;
#17575 = CARTESIAN_POINT ( 'NONE',  ( -15.62855498089999884, -101.6223710729999965, 3.522773483530000416 ) ) ;
#17576 = LINE ( 'NONE', #1998, #15525 ) ;
#17577 = CARTESIAN_POINT ( 'NONE',  ( -39.83713153847065769, -63.35496709430439921, 2.175426692284139651 ) ) ;
#17578 = ORIENTED_EDGE ( 'NONE', *, *, #19283, .F. ) ;
#17579 = AXIS2_PLACEMENT_3D ( 'NONE', #11921, #18490, #16585 ) ;
#17580 = DIRECTION ( 'NONE',  ( -0.6390296260299768161, 0.06995790998169656993, -0.7659941435069727023 ) ) ;
#17581 = CARTESIAN_POINT ( 'NONE',  ( -1.826285548319301455, -96.92941681384529318, 21.94491567526166520 ) ) ;
#17582 = CARTESIAN_POINT ( 'NONE',  ( -11.79122448039999860, -101.0403179300000005, -10.01466385380000013 ) ) ;
#17583 = CARTESIAN_POINT ( 'NONE',  ( -7.223639776384101374, -73.64317723970496843, 39.38195712097429180 ) ) ;
#17584 = CARTESIAN_POINT ( 'NONE',  ( -40.70731707320000226, -74.50000000000000000, -7.215414233289999757 ) ) ;
#17585 = ORIENTED_EDGE ( 'NONE', *, *, #7384, .F. ) ;
#17586 = CARTESIAN_POINT ( 'NONE',  ( 19.97576656849999921, -36.00000000000000000, -19.97576656849999921 ) ) ;
#17587 = CARTESIAN_POINT ( 'NONE',  ( -32.46931817979999835, -74.16345073059999038, -21.99116898890000016 ) ) ;
#17588 = CARTESIAN_POINT ( 'NONE',  ( -22.35195235113883783, -79.82938816292890749, -32.78357590675958733 ) ) ;
#17589 = B_SPLINE_CURVE_WITH_KNOTS ( 'NONE', 3,
 ( #26699, #22320, #13568, #10922, #2519, #8746, #17514, #22035, #11375, #28706, #24361, #20278, #9049, #18093, #4402, #6430, #15293, #13269, #345, #6881, #10776, #19976, #7034, #199, #6740, #15900, #26994, #4844, #17953, #15604, #13723, #24503 ),
 .UNSPECIFIED., .F., .F.,
 ( 4, 2, 2, 2, 1, 1, 1, 1, 1, 2, 2, 2, 2, 1, 1, 1, 1, 1, 2, 2, 4 ),
 ( 0.000000000000000000, 0.2500000000000248690, 0.3750000000000378031, 0.4375000000000447420, 0.4687500000000484612, 0.4843750000000501821, 0.4921875000000506817, 0.4960937500000511258, 0.4980468750000515143, 0.4990234375000516254, 0.5000000000000518474, 0.6250000000000320854, 0.6875000000000219824, 0.7187500000000174305, 0.7343750000000153211, 0.7421875000000136557, 0.7460937500000127676, 0.7480468750000124345, 0.7490234375000122125, 0.7500000000000119904, 1.000000000000000000 ),
 .UNSPECIFIED. ) ;
#17590 = ORIENTED_EDGE ( 'NONE', *, *, #7631, .F. ) ;
#17591 = B_SPLINE_SURFACE_WITH_KNOTS ( 'NONE', 4, 5, ( 
 ( #23523, #7669, #18730, #3144, #27626, #14213, #16534, #27759, #25566 ),
 ( #20917, #1250, #19006, #21060, #4068, #23104, #1119, #27476, #25296 ),
 ( #12002, #21329, #18874, #25710, #7795, #14621, #9957, #14483, #28032 ),
 ( #980, #10229, #1387, #3559, #16817, #16668, #12414, #21849, #15122 ),
 ( #10743, #27886, #14345, #12146, #19143, #24031, #9822, #5600, #5739 ) ),
 .UNSPECIFIED., .F., .F., .F.,
 ( 5, 5 ),
 ( 6, 3, 6 ),
 ( 27.16653081609999987, 27.95952390849999958 ),
 ( 0.000000000000000000, 0.2500000000000000000, 0.5000000000000000000 ),
 .UNSPECIFIED. ) ;
#17592 = DIRECTION ( 'NONE',  ( 0.000000000000000000, -1.000000000000000000, 0.000000000000000000 ) ) ;
#17593 = CARTESIAN_POINT ( 'NONE',  ( 19.61885648609999677, -35.93737992959999872, -9.235927176200000588 ) ) ;
#17594 = CARTESIAN_POINT ( 'NONE',  ( 0.000000000000000000, -108.5000000000000000, 0.000000000000000000 ) ) ;
#17595 = ORIENTED_EDGE ( 'NONE', *, *, #16236, .F. ) ;
#17596 = EDGE_CURVE ( 'NONE', #1478, #20961, #24026, .T. ) ;
#17597 = AXIS2_PLACEMENT_3D ( 'NONE', #3476, #6212, #25624 ) ;
#17598 = DIRECTION ( 'NONE',  ( -0.9952295494196654602, 0.000000000000000000, 0.09756097560976760563 ) ) ;
#17599 = CARTESIAN_POINT ( 'NONE',  ( -13.66444693457865078, -94.27895761266917418, -21.60767336590412668 ) ) ;
#17600 = VERTEX_POINT ( 'NONE', #1747 ) ;
#17601 = CARTESIAN_POINT ( 'NONE',  ( 19.98296174609999909, -94.98812477599999227, 14.17692170709999822 ) ) ;
#17602 = CARTESIAN_POINT ( 'NONE',  ( 46.36824973070000055, -73.69905166609999014, -3.512760466140000037 ) ) ;
#17603 = ORIENTED_EDGE ( 'NONE', *, *, #17837, .F. ) ;
#17604 = CARTESIAN_POINT ( 'NONE',  ( 0.000000000000000000, -92.50000000000000000, 0.000000000000000000 ) ) ;
#17605 = CARTESIAN_POINT ( 'NONE',  ( -42.51878914953488220, -63.24880261862898578, -0.5665023486488870441 ) ) ;
#17606 = EDGE_CURVE ( 'NONE', #2738, #19454, #27188, .T. ) ;
#17607 = CARTESIAN_POINT ( 'NONE',  ( 12.41938065250000101, -101.4254868729999970, -10.03851721480000059 ) ) ;
#17608 = CARTESIAN_POINT ( 'NONE',  ( -41.91080743279999865, -63.35440207070000440, -1.043878858150000033 ) ) ;
#17609 = DIRECTION ( 'NONE',  ( 0.000000000000000000, 1.000000000000000000, 0.000000000000000000 ) ) ;
#17610 = EDGE_LOOP ( 'NONE', ( #25698, #21104, #14557, #8954 ) ) ;
#17611 = CARTESIAN_POINT ( 'NONE',  ( 36.38880822659999836, -73.99825405529999500, -13.96626921939999910 ) ) ;
#17612 = CARTESIAN_POINT ( 'NONE',  ( 13.35715127229999943, -100.8746138070000029, -9.861395958219999258 ) ) ;
#17613 = PLANE ( 'NONE',  #6422 ) ;
#17614 = CARTESIAN_POINT ( 'NONE',  ( -11.85289063449999958, -94.98812477599999227, -21.44324726029999795 ) ) ;
#17615 = DIRECTION ( 'NONE',  ( 0.000000000000000000, -1.000000000000000000, 0.000000000000000000 ) ) ;
#17616 = FACE_OUTER_BOUND ( 'NONE', #15280, .T. ) ;
#17617 = CARTESIAN_POINT ( 'NONE',  ( -17.71392320319999669, -18.50000000000000000, 12.76655036999999915 ) ) ;
#17618 = ORIENTED_EDGE ( 'NONE', *, *, #23651, .T. ) ;
#17619 = CIRCLE ( 'NONE', #19475, 1.000000000000000888 ) ;
#17620 = DIRECTION ( 'NONE',  ( -0.000000000000000000, 1.000000000000000000, 0.000000000000000000 ) ) ;
#17621 = VECTOR ( 'NONE', #21039, 1000.000000000000000 ) ;
#17622 = DIRECTION ( 'NONE',  ( 0.000000000000000000, 1.000000000000000000, 0.000000000000000000 ) ) ;
#17623 = CARTESIAN_POINT ( 'NONE',  ( -23.77551070246358478, -92.93978723897004102, -19.10432693837231000 ) ) ;
#17624 = CARTESIAN_POINT ( 'NONE',  ( 47.25000000000000000, -79.00000000000000000, -13.75000000000000000 ) ) ;
#17625 = CARTESIAN_POINT ( 'NONE',  ( -0.8980256170553421180, -92.52048598157983861, -30.48678096363293477 ) ) ;
#17626 = DIRECTION ( 'NONE',  ( 0.000000000000000000, 1.000000000000000000, 0.000000000000000000 ) ) ;
#17627 = CARTESIAN_POINT ( 'NONE',  ( 36.73460205735974426, 0.000000000000000000, -55.82937180330987559 ) ) ;
#17628 = DIRECTION ( 'NONE',  ( 0.02956883857460810769, 0.000000000000000000, 0.9995627462972741517 ) ) ;
#17629 = CARTESIAN_POINT ( 'NONE',  ( 25.09792694589999940, -16.00000000000000000, 45.94144711499999545 ) ) ;
#17630 = CARTESIAN_POINT ( 'NONE',  ( -11.22183587500000002, -57.45864773929999814, -21.12541641649999846 ) ) ;
#17632 = ORIENTED_EDGE ( 'NONE', *, *, #10842, .F. ) ;
#17631 = ADVANCED_FACE ( 'NONE', ( #26222 ), #27719, .F. ) ;
#17633 = ADVANCED_FACE ( 'NONE', ( #8704 ), #18347, .T. ) ;
#17634 = CARTESIAN_POINT ( 'NONE',  ( 23.52741021270000132, -94.89420189139998740, -6.742682298520000117 ) ) ;
#17636 = EDGE_LOOP ( 'NONE', ( #28085, #1906, #10490, #13445 ) ) ;
#17635 = AXIS2_PLACEMENT_3D ( 'NONE', #16713, #10410, #14791 ) ;
#17637 = CARTESIAN_POINT ( 'NONE',  ( -13.46276276179999876, -19.49999999970000175, 20.39865906480000035 ) ) ;
#17638 = DIRECTION ( 'NONE',  ( 0.000000000000000000, 1.000000000000000000, 0.000000000000000000 ) ) ;
#17639 = ORIENTED_EDGE ( 'NONE', *, *, #15571, .F. ) ;
#17640 = CARTESIAN_POINT ( 'NONE',  ( 16.03761573839999954, -101.2306315440000049, 2.381275335019999773 ) ) ;
#17641 = AXIS2_PLACEMENT_3D ( 'NONE', #8272, #11006, #10443 ) ;
#17642 = EDGE_CURVE ( 'NONE', #22108, #7500, #22061, .T. ) ;
#17643 = AXIS2_PLACEMENT_3D ( 'NONE', #15848, #24166, #4199 ) ;
#17644 = VERTEX_POINT ( 'NONE', #26507 ) ;
#17645 = CARTESIAN_POINT ( 'NONE',  ( 0.000000000000000000, -111.0000000000000000, 0.000000000000000000 ) ) ;
#17646 = CARTESIAN_POINT ( 'NONE',  ( 9.476764215410000247, -84.00000000000000000, -38.08875739639999836 ) ) ;
#17647 = CARTESIAN_POINT ( 'NONE',  ( 0.04171660379150000236, -111.0000000000000000, 21.23044528579999835 ) ) ;
#17648 = CYLINDRICAL_SURFACE ( 'NONE', #14385, 57.74999999999999289 ) ;
#17649 = CARTESIAN_POINT ( 'NONE',  ( -40.29307695968953595, -65.70763704136885508, 2.219188376449546141 ) ) ;
#17650 = ORIENTED_EDGE ( 'NONE', *, *, #1656, .T. ) ;
#17651 = DIRECTION ( 'NONE',  ( 0.000000000000000000, 1.000000000000000000, 0.000000000000000000 ) ) ;
#17652 = CARTESIAN_POINT ( 'NONE',  ( 22.53098139629999963, -27.06313850649999964, 0.4808225629529999656 ) ) ;
#17653 = CARTESIAN_POINT ( 'NONE',  ( -14.81587592385739605, -80.00394138637977903, 36.34631758749846853 ) ) ;
#17654 = CARTESIAN_POINT ( 'NONE',  ( -13.11455779531268284, -92.71346081468166744, 27.53649186493240464 ) ) ;
#17655 = ORIENTED_EDGE ( 'NONE', *, *, #15676, .T. ) ;
#17656 = CYLINDRICAL_SURFACE ( 'NONE', #8075, 7.249999999999999112 ) ;
#17657 = CARTESIAN_POINT ( 'NONE',  ( -14.45392997149999914, -92.99999875040001029, 26.19394095939999900 ) ) ;
#17658 = ORIENTED_EDGE ( 'NONE', *, *, #11854, .F. ) ;
#17659 = CARTESIAN_POINT ( 'NONE',  ( 26.61465604159999998, -68.28989644159999273, 0.1578853838729999959 ) ) ;
#17660 = ADVANCED_FACE ( 'NONE', ( #24320 ), #2918, .T. ) ;
#17661 = AXIS2_PLACEMENT_3D ( 'NONE', #14871, #3410, #1781 ) ;
#17662 = CARTESIAN_POINT ( 'NONE',  ( 0.7145790383449999172, -100.7707614970000094, -15.83861793500000026 ) ) ;
#17663 = CARTESIAN_POINT ( 'NONE',  ( 9.564508935660001043, -57.40875689140000304, -23.52622281860000086 ) ) ;
#17664 = CARTESIAN_POINT ( 'NONE',  ( 15.74335372269999844, -101.5369810359999860, 2.854262349850000380 ) ) ;
#17665 = CARTESIAN_POINT ( 'NONE',  ( -11.22008224870000070, -57.43018267659999765, -22.06025767750000099 ) ) ;
#17666 = EDGE_LOOP ( 'NONE', ( #17489, #2342, #17219, #22044 ) ) ;
#17667 = CIRCLE ( 'NONE', #15298, 39.25000000000000000 ) ;
#17668 = TOROIDAL_SURFACE ( 'NONE', #13468, 21.14285714289999873, 0.5000000000000000000 ) ;
#17669 = CARTESIAN_POINT ( 'NONE',  ( 22.13628285440143983, -57.47600047054346817, -7.675802460420446671 ) ) ;
#17671 = EDGE_LOOP ( 'NONE', ( #5544, #26314, #8297, #16563, #14519, #11400 ) ) ;
#17670 = EDGE_CURVE ( 'NONE', #24319, #618, #17917, .T. ) ;
#17672 = EDGE_CURVE ( 'NONE', #14960, #27229, #4847, .T. ) ;
#17673 = CARTESIAN_POINT ( 'NONE',  ( 27.97334130874722291, -92.55017404142810733, 12.15492542743048787 ) ) ;
#17674 = DIRECTION ( 'NONE',  ( 1.000000000000000000, 0.000000000000000000, 0.000000000000000000 ) ) ;
#17675 = CARTESIAN_POINT ( 'NONE',  ( 24.60124523610000224, -92.58502644590001296, 14.64067842810000108 ) ) ;
#17676 = CARTESIAN_POINT ( 'NONE',  ( 6.865158367083817659, -101.5740747342471337, 14.51578316883484199 ) ) ;
#17677 = EDGE_LOOP ( 'NONE', ( #20784, #11472, #16828, #27765 ) ) ;
#17678 = PLANE ( 'NONE',  #14757 ) ;
#17679 = CARTESIAN_POINT ( 'NONE',  ( -12.88209131945397168, -100.4211561362087792, -11.03803975983561791 ) ) ;
#17680 = ORIENTED_EDGE ( 'NONE', *, *, #18844, .T. ) ;
#17681 = CARTESIAN_POINT ( 'NONE',  ( 8.154778043900000384, -36.28970872960000094, -21.27812994379999978 ) ) ;
#17682 = CARTESIAN_POINT ( 'NONE',  ( -41.75000000000000000, -65.31510159580000163, 2.337827133090000231 ) ) ;
#17683 = CIRCLE ( 'NONE', #8364, 32.39999999999999858 ) ;
#17684 = PRESENTATION_LAYER_ASSIGNMENT (  '', '', ( #1417 ) ) ;
#17685 = CARTESIAN_POINT ( 'NONE',  ( 8.660862689520000046, -98.53838189920000445, 16.57756802869999646 ) ) ;
#17686 = CARTESIAN_POINT ( 'NONE',  ( 46.25000000000000000, -75.00000000000000000, -13.75000000000000000 ) ) ;
#17687 = DIRECTION ( 'NONE',  ( 0.7678754814159409747, 0.000000000000000000, -0.6405991297529499695 ) ) ;
#17688 = CARTESIAN_POINT ( 'NONE',  ( -15.38256540239999914, -101.5026274779999937, 4.483298071290000131 ) ) ;
#17689 = CARTESIAN_POINT ( 'NONE',  ( -13.46276276189999876, -19.18584073440000282, 20.39865906470000212 ) ) ;
#17690 = DIRECTION ( 'NONE',  ( 0.2414462220490755373, 0.000000000000000000, 0.9704142011833033488 ) ) ;
#17691 = CARTESIAN_POINT ( 'NONE',  ( -36.71072769287544446, -65.10052340105973201, 0.07634552798238451732 ) ) ;
#17692 = EDGE_CURVE ( 'NONE', #19989, #23575, #23897, .T. ) ;
#17693 = ADVANCED_FACE ( 'NONE', ( #7281 ), #26233, .T. ) ;
#17694 = CARTESIAN_POINT ( 'NONE',  ( 26.58922696730754254, -92.50000267096380924, 13.46049426897001489 ) ) ;
#17695 = CARTESIAN_POINT ( 'NONE',  ( 0.000000000000000000, -34.10310889129999623, 0.000000000000000000 ) ) ;
#17696 = CARTESIAN_POINT ( 'NONE',  ( -38.26484107678280822, -65.11704020643527713, -2.761498650871582416 ) ) ;
#17697 = DIRECTION ( 'NONE',  ( -0.9734759478401043831, 0.000000000000000000, -0.2287893768880245871 ) ) ;
#17698 = CARTESIAN_POINT ( 'NONE',  ( 22.48686483693199278, -94.01603309715282819, 13.16869411391845546 ) ) ;
#17699 = ORIENTED_EDGE ( 'NONE', *, *, #7898, .F. ) ;
#17700 = CARTESIAN_POINT ( 'NONE',  ( 8.810535018830000453, -19.17198326990000012, -19.82299369949999956 ) ) ;
#17701 = CARTESIAN_POINT ( 'NONE',  ( 22.51363372970000043, -36.53914150059999599, -9.828880634039999009 ) ) ;
#17702 = EDGE_CURVE ( 'NONE', #23314, #20359, #17396, .T. ) ;
#17703 = CONICAL_SURFACE ( 'NONE', #16771, 55.67692378859999280, 1.047197551199999799 ) ;
#17704 = AXIS2_PLACEMENT_3D ( 'NONE', #12667, #19524, #1766 ) ;
#17705 = ORIENTED_EDGE ( 'NONE', *, *, #1297, .T. ) ;
#17706 = B_SPLINE_CURVE_WITH_KNOTS ( 'NONE', 3,
 ( #23700, #6209, #28078, #28494, #1708, #8532 ),
 .UNSPECIFIED., .F., .F.,
 ( 4, 2, 4 ),
 ( 0.000000000000000000, 0.5000000000000000000, 1.000000000000000000 ),
 .UNSPECIFIED. ) ;
#17707 = CARTESIAN_POINT ( 'NONE',  ( -12.17169857430000057, -60.55460316730000159, 20.45714472730000111 ) ) ;
#17708 = CARTESIAN_POINT ( 'NONE',  ( 7.215414233289999757, -74.50000000000000000, 40.70731707320000226 ) ) ;
#17709 = CARTESIAN_POINT ( 'NONE',  ( -24.67624118369999664, -94.54647010790000650, -3.610732365350000084 ) ) ;
#17710 = CARTESIAN_POINT ( 'NONE',  ( -20.27744904749999932, -56.20810645120000260, 14.66966877139999959 ) ) ;
#17711 = B_SPLINE_CURVE_WITH_KNOTS ( 'NONE', 5,
 ( #3629, #9644, #14821, #5295, #23725, #12488 ),
 .UNSPECIFIED., .F., .F.,
 ( 6, 6 ),
 ( 0.000000000000000000, 1.000000000000000000 ),
 .UNSPECIFIED. ) ;
#17712 = CARTESIAN_POINT ( 'NONE',  ( 38.57396449699999863, -80.50000000000000000, -9.597487326430000465 ) ) ;
#17713 = CARTESIAN_POINT ( 'NONE',  ( 20.63161943080000071, -19.46510050319999863, -7.734358783100000245 ) ) ;
#17714 = CARTESIAN_POINT ( 'NONE',  ( 16.00391739089999987, -100.1785804069999983, 4.588803089980000749 ) ) ;
#17715 = ORIENTED_EDGE ( 'NONE', *, *, #13238, .F. ) ;
#17716 = CARTESIAN_POINT ( 'NONE',  ( 4.500000000000000000, -15.00000000000000000, 50.00000000000000000 ) ) ;
#17717 = LINE ( 'NONE', #28345, #24303 ) ;
#17718 = EDGE_LOOP ( 'NONE', ( #22482, #17705 ) ) ;
#17719 = CARTESIAN_POINT ( 'NONE',  ( 7.560610606073200124, -92.50638022835023833, 29.54840156989449440 ) ) ;
#17720 = ORIENTED_EDGE ( 'NONE', *, *, #26289, .T. ) ;
#17721 = DIRECTION ( 'NONE',  ( 0.000000000000000000, -1.000000000000000000, 0.000000000000000000 ) ) ;
#17722 = CARTESIAN_POINT ( 'NONE',  ( 19.55467021020000118, -26.09744228899999996, 10.64706777249999980 ) ) ;
#17723 = AXIS2_PLACEMENT_3D ( 'NONE', #3512, #25655, #25513 ) ;
#17724 = DIRECTION ( 'NONE',  ( -0.4151946956541399669, 0.5000000000001689759, -0.7600087925152558821 ) ) ;
#17725 = CARTESIAN_POINT ( 'NONE',  ( 24.37463189540000030, -92.54807930239999791, -15.31860879340000103 ) ) ;
#17726 = CIRCLE ( 'NONE', #20048, 34.89999999999999858 ) ;
#17727 = TOROIDAL_SURFACE ( 'NONE', #1023, 30.50381168839999901, 2.000000000000000000 ) ;
#17728 = LINE ( 'NONE', #24423, #23895 ) ;
#17729 = CARTESIAN_POINT ( 'NONE',  ( 10.65559738969999870, -67.35763218280000331, -25.86638506229999734 ) ) ;
#17730 = CARTESIAN_POINT ( 'NONE',  ( -17.04099446512953975, -97.63928043689861624, 10.20266565317231411 ) ) ;
#17731 = VERTEX_POINT ( 'NONE', #11337 ) ;
#17732 = CARTESIAN_POINT ( 'NONE',  ( 11.70455088819999823, -93.00000000000000000, 8.942783294160001617 ) ) ;
#17733 = CARTESIAN_POINT ( 'NONE',  ( 8.996935515640000602, -29.61190174099999695, -19.27470341220000094 ) ) ;
#17734 = CARTESIAN_POINT ( 'NONE',  ( -7.249922261819999214, -74.00000000000000000, 40.03357376379999977 ) ) ;
#17735 = CARTESIAN_POINT ( 'NONE',  ( -13.18018122016701277, -99.62767017969132155, -11.26298828346031300 ) ) ;
#17736 = ORIENTED_EDGE ( 'NONE', *, *, #20752, .F. ) ;
#17737 = ADVANCED_FACE ( 'NONE', ( #7140 ), #12277, .T. ) ;
#17738 = DIRECTION ( 'NONE',  ( -0.000000000000000000, 1.000000000000000000, 0.000000000000000000 ) ) ;
#17739 = CARTESIAN_POINT ( 'NONE',  ( -32.34497379209999934, -74.07302383969998516, -22.05334043340000250 ) ) ;
#17740 = ORIENTED_EDGE ( 'NONE', *, *, #14169, .T. ) ;
#17741 = ADVANCED_FACE ( 'NONE', ( #20692 ), #4762, .F. ) ;
#17742 = ADVANCED_FACE ( 'NONE', ( #9150 ), #3205, .F. ) ;
#17743 = CARTESIAN_POINT ( 'NONE',  ( -5.122964312370000606, -100.0012764450000020, 17.27741718500000090 ) ) ;
#17744 = CIRCLE ( 'NONE', #5192, 7.250000000000000000 ) ;
#17745 = CARTESIAN_POINT ( 'NONE',  ( -17.63662161709793708, -94.54718950358140717, 16.06392408143854666 ) ) ;
#17746 = CIRCLE ( 'NONE', #6101, 16.00000000000000000 ) ;
#17747 = EDGE_LOOP ( 'NONE', ( #8291, #19622 ) ) ;
#17748 = CARTESIAN_POINT ( 'NONE',  ( -14.43573106120380523, -94.04667188284982160, -21.62179604614098949 ) ) ;
#17749 = ORIENTED_EDGE ( 'NONE', *, *, #11503, .T. ) ;
#17750 = CARTESIAN_POINT ( 'NONE',  ( 8.408333318189998979E-15, -74.00000000000000000, 40.00000000000000000 ) ) ;
#17751 = DIRECTION ( 'NONE',  ( 0.000000000000000000, 1.000000000000000000, 0.000000000000000000 ) ) ;
#17752 = CARTESIAN_POINT ( 'NONE',  ( -15.07208659220000158, -101.6484611540000031, 3.616933197699999880 ) ) ;
#17753 = EDGE_LOOP ( 'NONE', ( #5153, #27378, #11482, #28212 ) ) ;
#17754 = FACE_OUTER_BOUND ( 'NONE', #21869, .T. ) ;
#17755 = CARTESIAN_POINT ( 'NONE',  ( 21.08559791559969554, -57.47122622298945060, 10.49905601409981237 ) ) ;
#17756 = CARTESIAN_POINT ( 'NONE',  ( -38.25000000000000000, -64.11445222650000630, 2.684678751729999480 ) ) ;
#17757 = CARTESIAN_POINT ( 'NONE',  ( -18.92594650439999882, -92.98926436760000058, -21.15881086809999800 ) ) ;
#17758 = CARTESIAN_POINT ( 'NONE',  ( 3.166345171159999694, -92.50000000000000000, -25.30265318609999881 ) ) ;
#17759 = ORIENTED_EDGE ( 'NONE', *, *, #25573, .T. ) ;
#17760 = CARTESIAN_POINT ( 'NONE',  ( -1.526197323679999940, -100.8869817940000075, -15.59251925729999932 ) ) ;
#17761 = CARTESIAN_POINT ( 'NONE',  ( 0.000000000000000000, -91.50000000000000000, 0.000000000000000000 ) ) ;
#17762 = CARTESIAN_POINT ( 'NONE',  ( -22.04294097380000039, -74.04477437299999565, -32.27064897399999666 ) ) ;
#17763 = CARTESIAN_POINT ( 'NONE',  ( -2.355531086969999688, -56.22908209860000284, -24.30570137699999833 ) ) ;
#17764 = AXIS2_PLACEMENT_3D ( 'NONE', #13140, #22053, #4118 ) ;
#17765 = DIRECTION ( 'NONE',  ( 0.000000000000000000, 1.000000000000000000, 0.000000000000000000 ) ) ;
#17766 = VECTOR ( 'NONE', #23194, 1000.000000000000000 ) ;
#17767 = DIRECTION ( 'NONE',  ( 0.4794255386042040601, 0.000000000000000000, 0.8775825618903720926 ) ) ;
#17768 = CARTESIAN_POINT ( 'NONE',  ( 7.627566167509999495, -74.00000000000000000, -38.62788938250000115 ) ) ;
#17770 = VERTEX_POINT ( 'NONE', #15055 ) ;
#17769 = B_SPLINE_CURVE_WITH_KNOTS ( 'NONE', 3,
 ( #27334, #5335, #6938, #27488 ),
 .UNSPECIFIED., .F., .F.,
 ( 4, 4 ),
 ( 0.000000000000000000, 1.000000000000000000 ),
 .UNSPECIFIED. ) ;
#17771 = EDGE_CURVE ( 'NONE', #22153, #726, #3721, .T. ) ;
#17772 = CARTESIAN_POINT ( 'NONE',  ( 7.727581852389999284, -65.07443093669999712, -23.93312597839999967 ) ) ;
#17773 = CARTESIAN_POINT ( 'NONE',  ( -12.09704001540000107, -77.00000000000000000, 47.10905722069999513 ) ) ;
#17774 = CARTESIAN_POINT ( 'NONE',  ( 3.129685915889999670, -92.55031878719999838, -28.46238550929999889 ) ) ;
#17775 = CARTESIAN_POINT ( 'NONE',  ( -26.60903970598167589, -30.20000000000000284, -48.70752046822583736 ) ) ;
#17776 = LINE ( 'NONE', #11024, #1548 ) ;
#17777 = EDGE_CURVE ( 'NONE', #17228, #26695, #2993, .T. ) ;
#17778 = SHAPE_DEFINITION_REPRESENTATION ( #4079, #5912 ) ;
#17779 = FACE_OUTER_BOUND ( 'NONE', #23233, .T. ) ;
#17780 = ORIENTED_EDGE ( 'NONE', *, *, #10852, .T. ) ;
#17781 = CARTESIAN_POINT ( 'NONE',  ( 21.88853012090000050, -95.77248565319999329, -4.561213946619999682 ) ) ;
#17782 = EDGE_LOOP ( 'NONE', ( #2559, #9569, #18025, #15630 ) ) ;
#17783 = DIRECTION ( 'NONE',  ( 0.000000000000000000, -1.000000000000000000, 0.000000000000000000 ) ) ;
#17784 = CARTESIAN_POINT ( 'NONE',  ( -41.75000000000000000, -63.07912966450000880, -2.684678751739999925 ) ) ;
#17785 = ORIENTED_EDGE ( 'NONE', *, *, #7823, .T. ) ;
#17786 = AXIS2_PLACEMENT_3D ( 'NONE', #24028, #4211, #8430 ) ;
#17787 = CARTESIAN_POINT ( 'NONE',  ( 16.08037959500000014, -101.3150700380000018, 2.354223078750000031 ) ) ;
#17788 = CARTESIAN_POINT ( 'NONE',  ( -11.17102524760000115, -94.77696045309998851, -20.89250772250000310 ) ) ;
#17789 = CARTESIAN_POINT ( 'NONE',  ( 22.29340633682235762, -27.06771711593788154, -0.5094401308349546520 ) ) ;
#17790 = FACE_OUTER_BOUND ( 'NONE', #22188, .T. ) ;
#17791 = CARTESIAN_POINT ( 'NONE',  ( -18.87705750089999768, -97.64875668899999539, 6.521983386959999685 ) ) ;
#17792 = CARTESIAN_POINT ( 'NONE',  ( -10.67495457480000098, -18.61783141309999934, -18.91245961079999915 ) ) ;
#17793 = CARTESIAN_POINT ( 'NONE',  ( 47.21754643642892546, -79.25383175836481087, -0.8707321872798817752 ) ) ;
#17794 = ORIENTED_EDGE ( 'NONE', *, *, #23307, .F. ) ;
#17795 = CARTESIAN_POINT ( 'NONE',  ( 11.67094882200000150, -93.01584738609999192, -23.70866791699999965 ) ) ;
#17796 = CARTESIAN_POINT ( 'NONE',  ( 23.08853106659999810, -49.87553805839999654, -0.5737624632769999788 ) ) ;
#17797 = CARTESIAN_POINT ( 'NONE',  ( 0.000000000000000000, -94.59276292389999696, 0.000000000000000000 ) ) ;
#17798 = CARTESIAN_POINT ( 'NONE',  ( -13.12698473016186895, -92.72059904818586062, 27.53057009221356921 ) ) ;
#17799 = EDGE_LOOP ( 'NONE', ( #43, #1005, #3497, #4058, #16363 ) ) ;
#17800 = APPLICATION_CONTEXT ( 'automotive_design' ) ;
#17801 = CARTESIAN_POINT ( 'NONE',  ( -2.790536503729999840, -64.24504439390000243, -26.36014981959999659 ) ) ;
#17802 = CARTESIAN_POINT ( 'NONE',  ( -14.45493179810000051, -92.91908509549999451, 26.19282653499999824 ) ) ;
#17803 = CARTESIAN_POINT ( 'NONE',  ( -11.32307664120000013, -111.0000000000000000, 9.421136869679999748 ) ) ;
#17804 = ORIENTED_EDGE ( 'NONE', *, *, #907, .T. ) ;
#17805 = ADVANCED_FACE ( 'NONE', ( #10394 ), #5898, .T. ) ;
#17806 = CARTESIAN_POINT ( 'NONE',  ( 28.43332587009999912, -71.30829807179999591, 2.547915100310000014 ) ) ;
#17807 = CARTESIAN_POINT ( 'NONE',  ( 0.6052036509410000376, -100.3063911739999980, -17.04494785839999693 ) ) ;
#17808 = DIRECTION ( 'NONE',  ( 0.000000000000000000, 1.000000000000000000, 0.000000000000000000 ) ) ;
#17809 = CARTESIAN_POINT ( 'NONE',  ( -12.09181944520000052, -68.76958053619999589, -24.81138139369999962 ) ) ;
#17810 = CARTESIAN_POINT ( 'NONE',  ( -11.22183525189999820, -57.45864775100000088, -21.12541653479999937 ) ) ;
#17811 = TOROIDAL_SURFACE ( 'NONE', #22950, 29.91857981989999971, 10.00000000000000000 ) ;
#17812 = ADVANCED_FACE ( 'NONE', ( #25874 ), #10383, .F. ) ;
#17813 = CARTESIAN_POINT ( 'NONE',  ( 0.000000000000000000, -90.50000000000000000, 0.000000000000000000 ) ) ;
#17814 = EDGE_LOOP ( 'NONE', ( #20341, #10801, #802 ) ) ;
#17815 = CARTESIAN_POINT ( 'NONE',  ( -17.49492164999999844, -94.26879627710000875, 16.77352930379999663 ) ) ;
#17816 = FACE_OUTER_BOUND ( 'NONE', #19933, .T. ) ;
#17817 = CIRCLE ( 'NONE', #23420, 55.67692378859999991 ) ;
#17818 = CARTESIAN_POINT ( 'NONE',  ( -42.04069757566796284, -65.71630940569886548, -0.8827413896567969376 ) ) ;
#17819 = CARTESIAN_POINT ( 'NONE',  ( 23.18113824346705698, -92.50630337894787658, -19.82174805298759424 ) ) ;
#17820 = CARTESIAN_POINT ( 'NONE',  ( 18.40795691769999820, -93.85307999900000198, 16.77768149470000125 ) ) ;
#17821 = CARTESIAN_POINT ( 'NONE',  ( 11.36572001294154788, -99.82487968003715650, -12.74458838826810236 ) ) ;
#17822 = CARTESIAN_POINT ( 'NONE',  ( -7.380602427890000428, -101.2251655520000071, 14.44694227429999955 ) ) ;
#17823 = EDGE_LOOP ( 'NONE', ( #18385, #20812, #8589, #18468 ) ) ;
#17824 = CARTESIAN_POINT ( 'NONE',  ( -16.49390888960000368, -79.50000000000000000, 44.28897684009999836 ) ) ;
#17825 = CARTESIAN_POINT ( 'NONE',  ( -12.50561141126462950, -101.1248211534225163, -10.62038857907609746 ) ) ;
#17826 = CARTESIAN_POINT ( 'NONE',  ( 8.983162410790001218, -36.08615800729999989, -20.65197200649999942 ) ) ;
#17827 = AXIS2_PLACEMENT_3D ( 'NONE', #5710, #5150, #9652 ) ;
#17828 = CARTESIAN_POINT ( 'NONE',  ( -37.28811165380000148, -65.41419836839999391, -0.4550164754550000135 ) ) ;
#17829 = VERTEX_POINT ( 'NONE', #12725 ) ;
#17830 = DIRECTION ( 'NONE',  ( 1.000000000000000000, 0.000000000000000000, 0.000000000000000000 ) ) ;
#17831 = DIRECTION ( 'NONE',  ( 1.000000000000000000, 0.000000000000000000, 0.000000000000000000 ) ) ;
#17832 = CARTESIAN_POINT ( 'NONE',  ( 0.7331249433679999372, -99.53431242750001218, -17.39855866090000092 ) ) ;
#17833 = DIRECTION ( 'NONE',  ( 1.000000000000000000, 0.000000000000000000, 0.000000000000000000 ) ) ;
#17834 = CARTESIAN_POINT ( 'NONE',  ( 11.14159932559999966, -101.1364147039999892, -10.55279472049999967 ) ) ;
#17835 = CARTESIAN_POINT ( 'NONE',  ( 28.81424833448794942, -71.66550124175094538, 2.966281764014999656 ) ) ;
#17836 = CARTESIAN_POINT ( 'NONE',  ( 15.28191216724069612, -95.14282497074401590, 17.30484737853460686 ) ) ;
#17837 = EDGE_CURVE ( 'NONE', #5717, #14760, #24852, .T. ) ;
#17838 = DIRECTION ( 'NONE',  ( 0.000000000000000000, 1.000000000000000000, 0.000000000000000000 ) ) ;
#17839 = B_SPLINE_SURFACE_WITH_KNOTS ( 'NONE', 5, 5, ( 
 ( #2666, #11820, #792, #2810, #14303, #24806, #11667, #9189, #7033 ),
 ( #4843, #3109, #9492, #16342, #18397, #25250, #20578, #25098, #9776 ),
 ( #11517, #20875, #11961, #14166, #27432, #16189, #5279, #3245, #25393 ),
 ( #21017, #9631, #4979, #22769, #934, #5419, #27140, #14013, #18689 ),
 ( #22919, #13866, #27585, #23198, #13722, #20734, #12101, #7180, #7626 ),
 ( #18092, #18537, #15899, #22622, #10320, #1619, #23891, #19374, #1078 ) ),
 .UNSPECIFIED., .F., .F., .F.,
 ( 6, 6 ),
 ( 6, 3, 6 ),
 ( 0.000000000000000000, 46.92994236210000025 ),
 ( 0.000000000000000000, 1.000000000000000000, 2.000000000000000000 ),
 .UNSPECIFIED. ) ;
#17840 = AXIS2_PLACEMENT_3D ( 'NONE', #5340, #11430, #13929 ) ;
#17841 = DIRECTION ( 'NONE',  ( -0.3687499999999814260, 0.000000000000000000, 0.9295286103719527793 ) ) ;
#17842 = CARTESIAN_POINT ( 'NONE',  ( 8.125631349740000786, -93.00000000000000000, 24.17072847820000092 ) ) ;
#17843 = CARTESIAN_POINT ( 'NONE',  ( -13.45981261770000081, -71.49302942239999936, -24.63802173330000045 ) ) ;
#17844 = CARTESIAN_POINT ( 'NONE',  ( 24.64422047424358553, -93.08694455160397752, -15.44790685958040655 ) ) ;
#17845 = CARTESIAN_POINT ( 'NONE',  ( 25.04472665119416419, -93.40025063799829752, 11.65239934674920796 ) ) ;
#17846 = ORIENTED_EDGE ( 'NONE', *, *, #7062, .F. ) ;
#17847 = CARTESIAN_POINT ( 'NONE',  ( 36.59060417929999431, -75.00000019720000921, -14.75000047440000017 ) ) ;
#17848 = B_SPLINE_CURVE_WITH_KNOTS ( 'NONE', 3,
 ( #15139, #26097, #28271, #3669, #19674, #28144, #17649, #28563, #8598, #26530, #4086, #6125, #21443, #19391, #17501, #8179, #25957, #3810, #21868, #1920 ),
 .UNSPECIFIED., .F., .F.,
 ( 4, 2, 1, 2, 2, 2, 2, 1, 2, 2, 4 ),
 ( 0.000000000000000000, 0.1250000000000256462, 0.1875000000000293099, 0.2187500000000258127, 0.2500000000000223155, 0.5000000000000198730, 0.6250000000000186517, 0.6875000000000109912, 0.7187500000000103251, 0.7500000000000096589, 1.000000000000000000 ),
 .UNSPECIFIED. ) ;
#17849 = CIRCLE ( 'NONE', #14134, 0.5000000000000004441 ) ;
#17850 = ORIENTED_EDGE ( 'NONE', *, *, #8435, .F. ) ;
#17851 = CARTESIAN_POINT ( 'NONE',  ( -12.77829499169999927, -60.48561587360000402, 20.49208202570000026 ) ) ;
#17852 = CARTESIAN_POINT ( 'NONE',  ( 7.239203719536035031, -74.26034152750678174, 40.39659210523164745 ) ) ;
#17853 = CARTESIAN_POINT ( 'NONE',  ( -24.18521206880000207, -94.16309976690000383, -3.351640123200000154 ) ) ;
#17854 = CARTESIAN_POINT ( 'NONE',  ( 11.86655840719999944, -111.0000000000000000, -11.10431293650000129 ) ) ;
#17855 = AXIS2_PLACEMENT_3D ( 'NONE', #16766, #14302, #23478 ) ;
#17856 = EDGE_CURVE ( 'NONE', #20440, #3368, #12859, .T. ) ;
#17857 = CARTESIAN_POINT ( 'NONE',  ( -11.49099193064466817, -57.47122622516366874, -20.56185111776623486 ) ) ;
#17858 = ORIENTED_EDGE ( 'NONE', *, *, #3812, .T. ) ;
#17859 = AXIS2_PLACEMENT_3D ( 'NONE', #23672, #3716, #12577 ) ;
#17860 = CARTESIAN_POINT ( 'NONE',  ( 5.750078808689999654, -92.99020741600000406, 26.05463881579999708 ) ) ;
#17861 = CARTESIAN_POINT ( 'NONE',  ( 8.036479196959999201E-15, -84.50000000000000000, -43.75000000000000000 ) ) ;
#17862 = CARTESIAN_POINT ( 'NONE',  ( 7.250123850439999629, -73.75838856979999036, -39.12175830369999829 ) ) ;
#17863 = ORIENTED_EDGE ( 'NONE', *, *, #10792, .T. ) ;
#17864 = CARTESIAN_POINT ( 'NONE',  ( 7.915433586269055688, -92.54687141712493315, 29.45498200392744437 ) ) ;
#17865 = DIRECTION ( 'NONE',  ( 0.000000000000000000, 1.000000000000000000, 0.000000000000000000 ) ) ;
#17866 = CARTESIAN_POINT ( 'NONE',  ( 7.910521386969999291, -107.1975888269999899, 14.48011227119999944 ) ) ;
#17867 = CARTESIAN_POINT ( 'NONE',  ( -9.642319748410001168, -18.50000000000000000, -21.65408590870000083 ) ) ;
#17868 = AXIS2_PLACEMENT_3D ( 'NONE', #26951, #450, #27386 ) ;
#17869 = CARTESIAN_POINT ( 'NONE',  ( 7.105427357599999217E-15, -69.00000000000000000, 40.00000000000000000 ) ) ;
#17870 = CARTESIAN_POINT ( 'NONE',  ( 23.60843678869999707, -92.50000947299999154, -18.49675587200000137 ) ) ;
#17871 = CARTESIAN_POINT ( 'NONE',  ( 19.41707937360000003, -18.50000000000000000, 9.264983660499998663 ) ) ;
#17872 = CARTESIAN_POINT ( 'NONE',  ( 15.60567172371994005, -96.61062824143314742, 14.39926977216421911 ) ) ;
#17873 = CARTESIAN_POINT ( 'NONE',  ( -16.78971427428115604, -98.15124914739722328, 9.315172230392416708 ) ) ;
#17874 = EDGE_LOOP ( 'NONE', ( #19288, #3709, #9953 ) ) ;
#17875 = DIRECTION ( 'NONE',  ( 0.1066420485059984824, 0.000000000000000000, 0.9942974773630094409 ) ) ;
#17876 = CARTESIAN_POINT ( 'NONE',  ( 9.024081099289999131, -19.49999992740000110, -18.94592230980000380 ) ) ;
#17877 = CARTESIAN_POINT ( 'NONE',  ( -16.78865735879999832, -74.00000000000000000, 25.46808810279999946 ) ) ;
#17878 = DIRECTION ( 'NONE',  ( 0.000000000000000000, -1.000000000000000000, 0.000000000000000000 ) ) ;
#17879 = CARTESIAN_POINT ( 'NONE',  ( 23.93312658989999875, -65.07443093669999712, -7.727579958389999781 ) ) ;
#17880 = ORIENTED_EDGE ( 'NONE', *, *, #14157, .T. ) ;
#17881 = CIRCLE ( 'NONE', #9021, 55.67692378859999991 ) ;
#17882 = CIRCLE ( 'NONE', #228, 0.4999999999999967804 ) ;
#17883 = DIRECTION ( 'NONE',  ( 1.000000000000000000, 0.000000000000000000, 0.000000000000000000 ) ) ;
#17884 = VERTEX_POINT ( 'NONE', #26158 ) ;
#17885 = CARTESIAN_POINT ( 'NONE',  ( -7.325370793560000315, -18.50000000000000000, -24.94672208400000102 ) ) ;
#17886 = CARTESIAN_POINT ( 'NONE',  ( 19.54920062769999944, -35.79804965070000122, -9.079275989799999280 ) ) ;
#17887 = CONICAL_SURFACE ( 'NONE', #2556, 25.14975229270001833, 0.4276056667390000787 ) ;
#17888 = CARTESIAN_POINT ( 'NONE',  ( -0.5884599110899999541, -61.88564085890000399, -23.95484640009999922 ) ) ;
#17889 = EDGE_LOOP ( 'NONE', ( #12818, #22584, #26667 ) ) ;
#17890 = ADVANCED_FACE ( 'NONE', ( #21777, #28472, #8510, #14776, #17260, #28055 ), #19440, .F. ) ;
#17891 = TOROIDAL_SURFACE ( 'NONE', #21171, 0.5000000000000000000, 0.5000000000000000000 ) ;
#17892 = ORIENTED_EDGE ( 'NONE', *, *, #2284, .F. ) ;
#17893 = CARTESIAN_POINT ( 'NONE',  ( -26.03320226835694484, -93.98969193916619247, -2.031746379724110430 ) ) ;
#17894 = CARTESIAN_POINT ( 'NONE',  ( 20.70184870579999981, -94.64125193980000006, 13.94635761189999812 ) ) ;
#17895 = DIRECTION ( 'NONE',  ( 1.000000000000000000, 0.000000000000000000, 0.000000000000000000 ) ) ;
#17896 = ORIENTED_EDGE ( 'NONE', *, *, #7673, .T. ) ;
#17897 = CARTESIAN_POINT ( 'NONE',  ( 21.88953683589687671, -18.85523522018264941, -0.4607246244462301910 ) ) ;
#17898 = CARTESIAN_POINT ( 'NONE',  ( -22.00249007819999747, -79.50000010050000299, -32.67527197889999258 ) ) ;
#17899 = EDGE_CURVE ( 'NONE', #6032, #3916, #12065, .T. ) ;
#17900 = CIRCLE ( 'NONE', #5354, 57.75000000000000000 ) ;
#17901 = CARTESIAN_POINT ( 'NONE',  ( -17.80822692750000158, -93.00000000000000000, -18.25149456069999943 ) ) ;
#17902 = EDGE_CURVE ( 'NONE', #23053, #18448, #23013, .T. ) ;
#17903 = CARTESIAN_POINT ( 'NONE',  ( -11.77049175780000034, -94.59276292120000562, -20.68200896629999974 ) ) ;
#17904 = DIRECTION ( 'NONE',  ( 0.4794255386042041156, 0.000000000000000000, 0.8775825618903722036 ) ) ;
#17905 = VERTEX_POINT ( 'NONE', #17116 ) ;
#17906 = EDGE_CURVE ( 'NONE', #2020, #1715, #14171, .T. ) ;
#17907 = CARTESIAN_POINT ( 'NONE',  ( -18.05096283909999855, -93.00000167610001256, -23.30076369320000040 ) ) ;
#17908 = B_SPLINE_CURVE_WITH_KNOTS ( 'NONE', 3,
 ( #18354, #18494, #5382, #27387, #25206, #14265, #1041, #3203, #14122, #3070, #9879, #7723, #23295, #16590, #23849, #28356, #8121, #19064, #21382, #17010, #21526, #12889, #25898, #10700, #6356, #10286, #17443, #1301, #27948, #28502, #10423, #7985, #1443, #12614, #8388, #13047, #26185, #21665, #17147, #26035, #17294, #25765, #15219, #1582, #23707, #24135, #10143, #14807, #23992, #4171, #16878, #19341, #6216, #4027, #5794, #21805, #28217, #19196, #8251, #8538 ),
 .UNSPECIFIED., .F., .F.,
 ( 4, 2, 1, 1, 2, 2, 2, 2, 1, 1, 2, 2, 2, 2, 2, 2, 2, 1, 1, 2, 2, 2, 2, 1, 2, 2, 2, 1, 2, 2, 2, 2, 2, 4 ),
 ( 0.000000000000000000, 0.06250000000016231461, 0.09375000000024402702, 0.1093750000002796374, 0.1171875000002974010, 0.1250000000003151646, 0.1875000000004634071, 0.2187500000005324075, 0.2343750000005663525, 0.2421875000005828948, 0.2460937500005904999, 0.2500000000005981327, 0.3125000000005603296, 0.3437500000005472844, 0.3750000000005342393, 0.4375000000005085377, 0.4687500000004952150, 0.4843750000004883316, 0.4921875000004846124, 0.4960937500004830580, 0.5000000000004815037, 0.5625000000004248824, 0.5937500000003965717, 0.6093750000003884670, 0.6171875000003848033, 0.6250000000003811396, 0.6875000000003268497, 0.7187500000002994271, 0.7343750000002854383, 0.7500000000002715606, 0.8125000000002049472, 0.8437500000001668665, 0.8750000000001287859, 1.000000000000000000 ),
 .UNSPECIFIED. ) ;
#17909 = CARTESIAN_POINT ( 'NONE',  ( 13.82409059959999809, -99.78393592979999482, -10.43876300910000055 ) ) ;
#17910 = CARTESIAN_POINT ( 'NONE',  ( -40.03821526680000176, -73.97917265380000629, 7.260248548399999891 ) ) ;
#17911 = CARTESIAN_POINT ( 'NONE',  ( -21.98999391060000264, -74.14434415679998835, -32.46673792200000008 ) ) ;
#17912 = CARTESIAN_POINT ( 'NONE',  ( -11.71096558855141190, -94.52293547163276344, -20.87034194758490813 ) ) ;
#17913 = CARTESIAN_POINT ( 'NONE',  ( 50.00000000000000000, -13.00000000000000000, 4.500000000000000000 ) ) ;
#17914 = DIRECTION ( 'NONE',  ( 0.000000000000000000, 0.000000000000000000, -1.000000000000000000 ) ) ;
#17915 = CARTESIAN_POINT ( 'NONE',  ( -18.46388027080000072, -18.85965710059999978, 13.47021038649999980 ) ) ;
#17916 = ORIENTED_EDGE ( 'NONE', *, *, #3849, .T. ) ;
#17917 = LINE ( 'NONE', #27102, #25787 ) ;
#17918 = AXIS2_PLACEMENT_3D ( 'NONE', #471, #7599, #7454 ) ;
#17919 = CARTESIAN_POINT ( 'NONE',  ( 20.32381860445705968, -73.59933368480965044, -31.74152625608882161 ) ) ;
#17920 = CARTESIAN_POINT ( 'NONE',  ( -24.36269809241420958, -92.52640451560269241, -18.34963895739831941 ) ) ;
#17921 = FACE_OUTER_BOUND ( 'NONE', #8661, .T. ) ;
#17922 = CARTESIAN_POINT ( 'NONE',  ( -39.34243475499999221, -65.56519245710001087, 2.400371413390000264 ) ) ;
#17923 = DIRECTION ( 'NONE',  ( 0.000000000000000000, 0.000000000000000000, 1.000000000000000000 ) ) ;
#17924 = B_SPLINE_CURVE_WITH_KNOTS ( 'NONE', 5,
 ( #475, #15877, #5108, #4959, #622, #11494 ),
 .UNSPECIFIED., .F., .F.,
 ( 6, 6 ),
 ( 0.000000000000000000, 1.000000000000000000 ),
 .UNSPECIFIED. ) ;
#17925 = DIRECTION ( 'NONE',  ( 1.000000000000000000, 0.000000000000000000, 0.000000000000000000 ) ) ;
#17926 = DIRECTION ( 'NONE',  ( 0.000000000000000000, 1.000000000000000000, 0.000000000000000000 ) ) ;
#17927 = ORIENTED_EDGE ( 'NONE', *, *, #27347, .F. ) ;
#17928 = CARTESIAN_POINT ( 'NONE',  ( 24.39713723570755022, -19.23820060856055392, 1.459765156892738558 ) ) ;
#17929 = ORIENTED_EDGE ( 'NONE', *, *, #3188, .F. ) ;
#17930 = CARTESIAN_POINT ( 'NONE',  ( -13.61274982059999950, -49.81668346450000229, 20.80692016579999759 ) ) ;
#17931 = CARTESIAN_POINT ( 'NONE',  ( -31.00000000000000000, -11.00000000000000000, -4.500000000000000000 ) ) ;
#17932 = EDGE_LOOP ( 'NONE', ( #8669, #3156, #15387 ) ) ;
#17933 = DIRECTION ( 'NONE',  ( 0.4794255386042040046, 0.000000000000000000, 0.8775825618903722036 ) ) ;
#17934 = EDGE_CURVE ( 'NONE', #27321, #6167, #4175, .T. ) ;
#17935 = B_SPLINE_CURVE_WITH_KNOTS ( 'NONE', 3,
 ( #19068, #23297, #25769, #23711, #5925, #21121, #12618, #1303, #3342, #1177, #8124, #3754, #20979, #27809, #5797, #7588, #10016, #18930 ),
 .UNSPECIFIED., .F., .F.,
 ( 4, 2, 2, 2, 2, 2, 2, 2, 4 ),
 ( 0.000000000000000000, 0.1249999999999405753, 0.1874999999999341638, 0.2499999999999277800, 0.4999999999999432676, 0.6249999999999517053, 0.6874999999999569233, 0.7499999999999620304, 1.000000000000000000 ),
 .UNSPECIFIED. ) ;
#17936 = CARTESIAN_POINT ( 'NONE',  ( 6.042832004899746146, -93.45279863444233115, -26.77704013367506519 ) ) ;
#17937 = CARTESIAN_POINT ( 'NONE',  ( -26.33972759919999973, -74.50000000000000000, -36.23922253580000330 ) ) ;
#17938 = CARTESIAN_POINT ( 'NONE',  ( -19.97974828950000159, -95.94978106879999302, 10.41054471420000027 ) ) ;
#17939 = CARTESIAN_POINT ( 'NONE',  ( 26.57206548991637973, -68.20221397703001287, 0.6012562671682266657 ) ) ;
#17940 = CARTESIAN_POINT ( 'NONE',  ( 26.22877582859999990, -72.82938648530000592, 11.61106434019999867 ) ) ;
#17941 = ORIENTED_EDGE ( 'NONE', *, *, #1722, .T. ) ;
#17942 = EDGE_CURVE ( 'NONE', #22026, #28497, #3012, .T. ) ;
#17943 = DIRECTION ( 'NONE',  ( 0.000000000000000000, -1.000000000000000000, 0.000000000000000000 ) ) ;
#17944 = CARTESIAN_POINT ( 'NONE',  ( 0.000000000000000000, -102.5000000000000000, 0.000000000000000000 ) ) ;
#17945 = CARTESIAN_POINT ( 'NONE',  ( -12.92668336025674414, -92.62938374235253036, 27.62520349261831498 ) ) ;
#17946 = ORIENTED_EDGE ( 'NONE', *, *, #26793, .F. ) ;
#17947 = FACE_OUTER_BOUND ( 'NONE', #12737, .T. ) ;
#17948 = CARTESIAN_POINT ( 'NONE',  ( -14.87798422589999880, -92.52476525819999154, 24.84728676379999968 ) ) ;
#17949 = CARTESIAN_POINT ( 'NONE',  ( 19.97576656849999921, -19.50000000000000000, -19.97576656849999921 ) ) ;
#17950 = EDGE_LOOP ( 'NONE', ( #6580, #8936, #27983, #22278 ) ) ;
#17951 = CARTESIAN_POINT ( 'NONE',  ( 27.79580722110000224, -70.93604331640000282, 1.283943149509999992 ) ) ;
#17952 = CARTESIAN_POINT ( 'NONE',  ( 1.080755419719999999, -99.91102932019998661, -16.89321760849999876 ) ) ;
#17953 = CARTESIAN_POINT ( 'NONE',  ( 26.08183366116990243, -74.32916785640455259, -29.29060224673261459 ) ) ;
#17954 = CARTESIAN_POINT ( 'NONE',  ( -12.22902516030000086, -69.69726588759999686, -24.77074270770000197 ) ) ;
#17955 = CARTESIAN_POINT ( 'NONE',  ( 23.78781103989999934, -65.02207070560001512, -8.286109287880000451 ) ) ;
#17956 = FACE_OUTER_BOUND ( 'NONE', #3173, .T. ) ;
#17957 = DIRECTION ( 'NONE',  ( 0.000000000000000000, -1.000000000000000000, 0.000000000000000000 ) ) ;
#17958 = DIRECTION ( 'NONE',  ( 0.7071067811865475727, 0.000000000000000000, 0.7071067811865475727 ) ) ;
#17959 = ORIENTED_EDGE ( 'NONE', *, *, #3072, .F. ) ;
#17960 = CARTESIAN_POINT ( 'NONE',  ( -3.610293368829999849, -18.50000000000000000, -24.43613445369999937 ) ) ;
#17961 = CARTESIAN_POINT ( 'NONE',  ( 15.11062958683252511, -101.1604341566294920, 2.739549772153475615 ) ) ;
#17962 = DIRECTION ( 'NONE',  ( 1.000000000000000000, 0.000000000000000000, 0.000000000000000000 ) ) ;
#17963 = AXIS2_PLACEMENT_3D ( 'NONE', #7923, #16807, #18997 ) ;
#17964 = CARTESIAN_POINT ( 'NONE',  ( 23.09404321033341034, -92.49999999999997158, -19.92320476265976481 ) ) ;
#17965 = CARTESIAN_POINT ( 'NONE',  ( 18.38388831859999684, -93.67869433859999617, 16.94838898949999972 ) ) ;
#17966 = EDGE_CURVE ( 'NONE', #20274, #21210, #28478, .T. ) ;
#17967 = CARTESIAN_POINT ( 'NONE',  ( 22.76152370333024422, -19.47294761907691907, 1.041135354044837147 ) ) ;
#17968 = ORIENTED_EDGE ( 'NONE', *, *, #7540, .F. ) ;
#17969 = CARTESIAN_POINT ( 'NONE',  ( 27.02346536675331734, -72.26149772935862359, -11.39735799491197987 ) ) ;
#17970 = CARTESIAN_POINT ( 'NONE',  ( -12.45338840115624990, -101.3586211803998367, -10.39906174622668189 ) ) ;
#17971 = CARTESIAN_POINT ( 'NONE',  ( 9.289605485279999186, -35.98680449440000473, -20.22331461079999926 ) ) ;
#17972 = ADVANCED_FACE ( 'NONE', ( #22361 ), #21596, .T. ) ;
#17973 = DIRECTION ( 'NONE',  ( 1.000000000000000000, 0.000000000000000000, 0.000000000000000000 ) ) ;
#17974 = EDGE_CURVE ( 'NONE', #23734, #27321, #392, .T. ) ;
#17975 = DIRECTION ( 'NONE',  ( 0.000000000000000000, 1.000000000000000000, 0.000000000000000000 ) ) ;
#17976 = CARTESIAN_POINT ( 'NONE',  ( 24.41973528469999977, -18.87168159810000034, 1.581049218290000002 ) ) ;
#17977 = CARTESIAN_POINT ( 'NONE',  ( -2.004260180370000199, -97.53592492889998766, -19.96958033499999985 ) ) ;
#17978 = FACE_OUTER_BOUND ( 'NONE', #12982, .T. ) ;
#17979 = ORIENTED_EDGE ( 'NONE', *, *, #12413, .T. ) ;
#17980 = CARTESIAN_POINT ( 'NONE',  ( 11.78180866139999949, -101.1659666750000071, -10.84551784730000001 ) ) ;
#17981 = CARTESIAN_POINT ( 'NONE',  ( 28.22776569104305722, -69.76795196468695792, 2.414911384691903251 ) ) ;
#17982 = CARTESIAN_POINT ( 'NONE',  ( -19.03193910350634610, -98.07255008389248019, -7.553244766087960471 ) ) ;
#17983 = CARTESIAN_POINT ( 'NONE',  ( 7.019998623859999398, -53.29680639659999741, -22.12830645909999916 ) ) ;
#17984 = CARTESIAN_POINT ( 'NONE',  ( 20.82957722899999808, -36.00000000010000178, -9.510883249549999974 ) ) ;
#17985 = DIRECTION ( 'NONE',  ( -0.9704142011833034598, 0.000000000000000000, -0.2414462220490750932 ) ) ;
#17986 = LINE ( 'NONE', #17843, #1248 ) ;
#17987 = LINE ( 'NONE', #13606, #9033 ) ;
#17988 = CARTESIAN_POINT ( 'NONE',  ( 1.013794083399999955E-14, -69.50000000000000000, 33.25000000000000000 ) ) ;
#17989 = ORIENTED_EDGE ( 'NONE', *, *, #26947, .T. ) ;
#17990 = DIRECTION ( 'NONE',  ( 1.000000000000000000, 0.000000000000000000, 0.000000000000000000 ) ) ;
#17991 = CARTESIAN_POINT ( 'NONE',  ( 8.140397668380000340, -100.8869818179999953, 13.38618156149999905 ) ) ;
#17992 = ORIENTED_EDGE ( 'NONE', *, *, #14658, .F. ) ;
#17993 = CARTESIAN_POINT ( 'NONE',  ( -5.873418876839999747, -111.0000000000000000, 15.15334698740000086 ) ) ;
#17994 = CARTESIAN_POINT ( 'NONE',  ( -11.31498420849999853, -60.59635495490000778, 20.73642217629999962 ) ) ;
#17995 = CARTESIAN_POINT ( 'NONE',  ( 7.244146985818051832, -74.18164516875302184, 40.29126735535029269 ) ) ;
#17996 = CARTESIAN_POINT ( 'NONE',  ( 0.000000000000000000, 0.000000000000000000, 0.000000000000000000 ) ) ;
#17997 = CARTESIAN_POINT ( 'NONE',  ( 21.85900874260000037, -37.33604033319999616, -8.605626153620001162 ) ) ;
#17998 = CARTESIAN_POINT ( 'NONE',  ( -12.06048066911961492, -66.52142429456056050, -24.43994840845913075 ) ) ;
#17999 = EDGE_CURVE ( 'NONE', #23425, #6357, #20168, .T. ) ;
#18000 = CARTESIAN_POINT ( 'NONE',  ( 16.78330657029999884, -99.55609327400000552, 4.537757829670000298 ) ) ;
#18001 = ORIENTED_EDGE ( 'NONE', *, *, #16717, .T. ) ;
#18002 = DIRECTION ( 'NONE',  ( 1.738658080640003812E-17, 0.000000000000000000, -1.000000000000000000 ) ) ;
#18003 = EDGE_CURVE ( 'NONE', #23692, #3267, #27114, .T. ) ;
#18004 = CARTESIAN_POINT ( 'NONE',  ( -19.68882303210000018, -96.97547176739999486, -6.799171120899999643 ) ) ;
#18005 = ORIENTED_EDGE ( 'NONE', *, *, #17487, .F. ) ;
#18006 = CARTESIAN_POINT ( 'NONE',  ( -13.17060483900000101, -68.28989248250000799, -23.12790341000000183 ) ) ;
#18007 = CARTESIAN_POINT ( 'NONE',  ( 0.4174863123245782792, -99.84800943039545018, -17.32495207964082695 ) ) ;
#18008 = DIRECTION ( 'NONE',  ( 0.4794255386042040046, 0.000000000000000000, 0.8775825618903722036 ) ) ;
#18009 = CARTESIAN_POINT ( 'NONE',  ( 19.74600256529999953, -32.73130089770000239, 10.78004968070000125 ) ) ;
#18010 = CARTESIAN_POINT ( 'NONE',  ( -0.5856137342820000313, -19.46510053389999939, -22.02591827759999887 ) ) ;
#18011 = CARTESIAN_POINT ( 'NONE',  ( 0.000000000000000000, -17.89999999999999858, 0.000000000000000000 ) ) ;
#18012 = CARTESIAN_POINT ( 'NONE',  ( 22.16736984139999933, -65.04750180880000698, 11.85329599529999989 ) ) ;
#18013 = CARTESIAN_POINT ( 'NONE',  ( -32.76786048424294506, -79.86746516107372429, -22.38819307479873544 ) ) ;
#18014 = CARTESIAN_POINT ( 'NONE',  ( -16.14916233553648794, -99.20418361269911145, 7.582005830281769221 ) ) ;
#18015 = B_SPLINE_SURFACE_WITH_KNOTS ( 'NONE', 5, 5, ( 
 ( #2710, #24850, #27184, #9095, #9239, #16090 ),
 ( #5027, #13915, #689, #11717, #9541, #18443 ),
 ( #27329, #2570, #11418, #7371, #27040, #7531 ),
 ( #25147, #3010, #16387, #20320, #17997, #18141 ),
 ( #15945, #4888, #6916, #237, #15783, #26877 ),
 ( #9082, #17984, #26504, #9146, #2036, #8700 ) ),
 .UNSPECIFIED., .F., .F., .F.,
 ( 6, 6 ),
 ( 6, 6 ),
 ( 3.491867373409999864, 4.007730545210000273 ),
 ( 0.000000000000000000, 2.000000000000000000 ),
 .UNSPECIFIED. ) ;
#18016 = EDGE_LOOP ( 'NONE', ( #26902, #28306, #23485, #10870 ) ) ;
#18017 = CARTESIAN_POINT ( 'NONE',  ( -15.50938051129999984, -101.3150705480000084, 4.855933523060000034 ) ) ;
#18018 = CARTESIAN_POINT ( 'NONE',  ( -3.363116624290108270, -98.28141829459690371, 19.92205903335984374 ) ) ;
#18019 = CARTESIAN_POINT ( 'NONE',  ( -12.86641141129999966, -100.1981337080000003, -11.08525741000000053 ) ) ;
#18020 = CARTESIAN_POINT ( 'NONE',  ( 0.000000000000000000, -23.30310889129999907, 0.000000000000000000 ) ) ;
#18021 = CARTESIAN_POINT ( 'NONE',  ( -40.03809227510000568, -73.97913911409999344, -7.260235792849999648 ) ) ;
#18022 = EDGE_LOOP ( 'NONE', ( #5169, #8479, #15806, #18901 ) ) ;
#18023 = EDGE_CURVE ( 'NONE', #17343, #23088, #10400, .T. ) ;
#18024 = CARTESIAN_POINT ( 'NONE',  ( 26.68762699244526004, -92.64884742711814170, -14.76556618572936763 ) ) ;
#18025 = ORIENTED_EDGE ( 'NONE', *, *, #4441, .F. ) ;
#18026 = DIRECTION ( 'NONE',  ( 0.000000000000000000, 1.000000000000000000, 0.000000000000000000 ) ) ;
#18027 = AXIS2_PLACEMENT_3D ( 'NONE', #21563, #16625, #6104 ) ;
#18028 = CARTESIAN_POINT ( 'NONE',  ( -7.910521386969999291, -107.1975888269999899, -14.48011227119999944 ) ) ;
#18029 = CARTESIAN_POINT ( 'NONE',  ( 11.26951408729999926, -92.92894616350000092, 27.60410696470000147 ) ) ;
#18030 = ORIENTED_EDGE ( 'NONE', *, *, #16021, .F. ) ;
#18031 = EDGE_CURVE ( 'NONE', #23988, #18741, #17881, .T. ) ;
#18032 = CARTESIAN_POINT ( 'NONE',  ( -14.93121066289999987, -82.25000000000000000, 36.29905574720000061 ) ) ;
#18033 = VERTEX_POINT ( 'NONE', #22958 ) ;
#18034 = CARTESIAN_POINT ( 'NONE',  ( -27.45034045483756913, -93.45279863387368380, 0.06712639151115551428 ) ) ;
#18035 = CARTESIAN_POINT ( 'NONE',  ( 19.57843401649999748, -94.59276292120000562, 13.52682122920000118 ) ) ;
#18036 = DIRECTION ( 'NONE',  ( 0.9982470477219616001, 0.000000000000000000, 0.05918472534689760839 ) ) ;
#18037 = ORIENTED_EDGE ( 'NONE', *, *, #7604, .T. ) ;
#18038 = CARTESIAN_POINT ( 'NONE',  ( 0.000000000000000000, -110.0000000000000000, 5.500000000000000000 ) ) ;
#18039 = CARTESIAN_POINT ( 'NONE',  ( 38.62788938250000115, -74.00000000000000000, 7.627566167509999495 ) ) ;
#18040 = VECTOR ( 'NONE', #9207, 1000.000000000000000 ) ;
#18041 = ADVANCED_FACE ( 'NONE', ( #27621 ), #25289, .T. ) ;
#18042 = CARTESIAN_POINT ( 'NONE',  ( -0.7205257401510000159, -111.0000000000000000, -15.98376809950000066 ) ) ;
#18043 = CARTESIAN_POINT ( 'NONE',  ( 0.000000000000000000, -16.50000000000000000, 0.000000000000000000 ) ) ;
#18044 = CARTESIAN_POINT ( 'NONE',  ( 7.460698725479999927E-15, -73.50000000000000000, 40.00000000000000000 ) ) ;
#18045 = ORIENTED_EDGE ( 'NONE', *, *, #13073, .T. ) ;
#18046 = CARTESIAN_POINT ( 'NONE',  ( -2.876553231629999985, -100.0000000000000000, -5.265495371340000119 ) ) ;
#18047 = CARTESIAN_POINT ( 'NONE',  ( -2.583988331150000040, -57.40875702419999982, -25.23271569440000306 ) ) ;
#18048 = DIRECTION ( 'NONE',  ( 0.000000000000000000, 1.000000000000000000, 0.000000000000000000 ) ) ;
#18049 = CARTESIAN_POINT ( 'NONE',  ( -22.02869148110000452, -74.01492597349999869, -32.14913059759999214 ) ) ;
#18050 = CARTESIAN_POINT ( 'NONE',  ( 8.988996100299999625, -34.66800400750000222, -19.43643858049999906 ) ) ;
#18051 = CYLINDRICAL_SURFACE ( 'NONE', #8733, 5.000000000000000000 ) ;
#18052 = CARTESIAN_POINT ( 'NONE',  ( 1.080755419719999999, -99.91102932019998661, -16.89321760849999876 ) ) ;
#18053 = CARTESIAN_POINT ( 'NONE',  ( 21.75659477429999811, -93.00000000000000000, -13.30039788230000042 ) ) ;
#18054 = ORIENTED_EDGE ( 'NONE', *, *, #20660, .F. ) ;
#18055 = DIRECTION ( 'NONE',  ( 0.000000000000000000, 1.000000000000000000, 0.000000000000000000 ) ) ;
#18056 = EDGE_CURVE ( 'NONE', #26990, #13393, #691, .T. ) ;
#18057 = CARTESIAN_POINT ( 'NONE',  ( -11.16118678780000018, -74.00000000000000000, 46.75000000000000000 ) ) ;
#18058 = CARTESIAN_POINT ( 'NONE',  ( 3.116266000930000057, -91.00000000000000000, 5.704286652290000426 ) ) ;
#18059 = CARTESIAN_POINT ( 'NONE',  ( -23.77086693186838318, -92.96960399591381474, -19.11009903990889569 ) ) ;
#18060 = CARTESIAN_POINT ( 'NONE',  ( 40.50000000000000000, -11.00000000000000000, 4.500000000000000000 ) ) ;
#18061 = CARTESIAN_POINT ( 'NONE',  ( 47.25083273380000293, -79.30142995810000173, -0.9228940748419999229 ) ) ;
#18062 = CARTESIAN_POINT ( 'NONE',  ( 13.45981261770000081, -71.49302942239999936, 24.63802173330000045 ) ) ;
#18063 = AXIS2_PLACEMENT_3D ( 'NONE', #26148, #19011, #12291 ) ;
#18064 = PRODUCT_CONTEXT ( 'NONE', #11440, 'mechanical' ) ;
#18065 = AXIS2_PLACEMENT_3D ( 'NONE', #4201, #4053, #12920 ) ;
#18066 = CARTESIAN_POINT ( 'NONE',  ( 23.42789392040000251, -57.47571038070000782, 0.04069498556230000119 ) ) ;
#18067 = ADVANCED_FACE ( 'NONE', ( #15933 ), #16223, .F. ) ;
#18068 = VERTEX_POINT ( 'NONE', #9952 ) ;
#18069 = CARTESIAN_POINT ( 'NONE',  ( 14.28941763439999946, -93.00000000000000000, -3.575252188409999921 ) ) ;
#18070 = CARTESIAN_POINT ( 'NONE',  ( 46.91398284789494966, -74.02346682147648949, -2.186286367158106980 ) ) ;
#18071 = ORIENTED_EDGE ( 'NONE', *, *, #16593, .T. ) ;
#18072 = CARTESIAN_POINT ( 'NONE',  ( -14.15885437638525168, -18.49999999992862953, 20.15290185130359291 ) ) ;
#18073 = FACE_OUTER_BOUND ( 'NONE', #20360, .T. ) ;
#18074 = ORIENTED_EDGE ( 'NONE', *, *, #22784, .T. ) ;
#18075 = CARTESIAN_POINT ( 'NONE',  ( 9.476129726560001743, -36.00000000000000000, -20.06309461059999677 ) ) ;
#18076 = DIRECTION ( 'NONE',  ( 0.000000000000000000, 1.000000000000000000, 0.000000000000000000 ) ) ;
#18077 = CARTESIAN_POINT ( 'NONE',  ( 22.02882315030000271, -19.46510050329999686, -0.4636558402470000173 ) ) ;
#18078 = DIRECTION ( 'NONE',  ( 1.000000000000000000, 0.000000000000000000, 0.000000000000000000 ) ) ;
#18079 = CARTESIAN_POINT ( 'NONE',  ( -18.07120458720000045, -98.58299283580001315, 4.768611213479999833 ) ) ;
#18080 = CARTESIAN_POINT ( 'NONE',  ( 27.13958276158709282, -67.66819096094158681, 1.745391524347732704 ) ) ;
#18081 = ORIENTED_EDGE ( 'NONE', *, *, #24232, .T. ) ;
#18082 = VECTOR ( 'NONE', #13818, 1000.000000000000000 ) ;
#18083 = CARTESIAN_POINT ( 'NONE',  ( 8.660164454169999360, -92.99999854809999533, -27.14861362650000132 ) ) ;
#18084 = CARTESIAN_POINT ( 'NONE',  ( -2.578307999469999778, -19.50000000000000000, -25.11373953509999879 ) ) ;
#18085 = CARTESIAN_POINT ( 'NONE',  ( -32.32657687519999712, -74.05570514439999386, -21.80503578329999925 ) ) ;
#18086 = ORIENTED_EDGE ( 'NONE', *, *, #21392, .T. ) ;
#18087 = CARTESIAN_POINT ( 'NONE',  ( 3.907985046679999924E-15, -73.50000000000000000, -40.00000000000000000 ) ) ;
#18088 = DIRECTION ( 'NONE',  ( 0.000000000000000000, 1.000000000000000000, 0.000000000000000000 ) ) ;
#18089 = CARTESIAN_POINT ( 'NONE',  ( -21.88268327719999817, -66.31484486759998731, 16.13005244970000263 ) ) ;
#18090 = ORIENTED_EDGE ( 'NONE', *, *, #10305, .T. ) ;
#18091 = CARTESIAN_POINT ( 'NONE',  ( 37.29611236860000645, -80.00000000000000000, -13.75000000000000000 ) ) ;
#18092 = CARTESIAN_POINT ( 'NONE',  ( -18.78215030510000005, -19.46363745430000236, 11.52009539260000004 ) ) ;
#18093 = CARTESIAN_POINT ( 'NONE',  ( 24.27323469296766234, -74.17273658677886772, -30.68895570800956918 ) ) ;
#18094 = DIRECTION ( 'NONE',  ( 0.000000000000000000, 1.000000000000000000, 0.000000000000000000 ) ) ;
#18095 = EDGE_CURVE ( 'NONE', #11312, #18883, #5591, .T. ) ;
#18096 = DIRECTION ( 'NONE',  ( 0.000000000000000000, -1.000000000000000000, 0.000000000000000000 ) ) ;
#18097 = EDGE_CURVE ( 'NONE', #8116, #20323, #11824, .T. ) ;
#18098 = B_SPLINE_CURVE_WITH_KNOTS ( 'NONE', 5,
 ( #18017, #28779, #10982, #22103, #118, #15216 ),
 .UNSPECIFIED., .F., .F.,
 ( 6, 6 ),
 ( 0.000000000000000000, 1.000000000000000000 ),
 .UNSPECIFIED. ) ;
#18099 = CARTESIAN_POINT ( 'NONE',  ( 8.235816542629999560E-15, -69.50000000000000000, -40.00000000000000000 ) ) ;
#18100 = VECTOR ( 'NONE', #16995, 1000.000000000000000 ) ;
#18101 = DIRECTION ( 'NONE',  ( -0.000000000000000000, 1.000000000000000000, 0.000000000000000000 ) ) ;
#18102 = EDGE_CURVE ( 'NONE', #15244, #26586, #17397, .T. ) ;
#18103 = ADVANCED_FACE ( 'NONE', ( #3282 ), #13758, .F. ) ;
#18104 = AXIS2_PLACEMENT_3D ( 'NONE', #23320, #21409, #5818 ) ;
#18105 = AXIS2_PLACEMENT_3D ( 'NONE', #23704, #12468, #14939 ) ;
#18106 = VERTEX_POINT ( 'NONE', #25138 ) ;
#18107 = CIRCLE ( 'NONE', #15757, 11.00000000000000000 ) ;
#18108 = CARTESIAN_POINT ( 'NONE',  ( 10.29737924729999854, -36.00000000000000000, -20.64806254930000051 ) ) ;
#18109 = DIRECTION ( 'NONE',  ( 0.000000000000000000, 1.000000000000000000, 0.000000000000000000 ) ) ;
#18110 = CARTESIAN_POINT ( 'NONE',  ( 15.71723844345814669, -101.4628082233788007, 2.849527662385800575 ) ) ;
#18111 = AXIS2_PLACEMENT_3D ( 'NONE', #1324, #14697, #11945 ) ;
#18112 = CARTESIAN_POINT ( 'NONE',  ( 8.069589370679999263, -101.0685846549999951, 13.92289990319999937 ) ) ;
#18113 = EDGE_LOOP ( 'NONE', ( #3418, #8012, #19802, #1422 ) ) ;
#18114 = CARTESIAN_POINT ( 'NONE',  ( 7.440556932049999794, -74.12472287219999600, 39.45553247920000217 ) ) ;
#18115 = CARTESIAN_POINT ( 'NONE',  ( 9.273485931230000645, -94.57749572790000059, -22.35124366870000046 ) ) ;
#18116 = CARTESIAN_POINT ( 'NONE',  ( 9.872833180276398224, -95.57586223587027519, -20.31377284688967322 ) ) ;
#18117 = CARTESIAN_POINT ( 'NONE',  ( -3.730706907091303481, -79.99999997488282588, 46.61318877841384989 ) ) ;
#18118 = CARTESIAN_POINT ( 'NONE',  ( 8.390131615779999663, -37.63096262599999875, -21.73500566539999923 ) ) ;
#18119 = CARTESIAN_POINT ( 'NONE',  ( -37.75000000000000000, -65.63577453799999262, -0.7216878364849999006 ) ) ;
#18120 = ORIENTED_EDGE ( 'NONE', *, *, #25959, .T. ) ;
#18121 = DIRECTION ( 'NONE',  ( 0.000000000000000000, -1.000000000000000000, 0.000000000000000000 ) ) ;
#18122 = DIRECTION ( 'NONE',  ( 1.000000000000000000, 0.000000000000000000, 0.000000000000000000 ) ) ;
#18123 = DIRECTION ( 'NONE',  ( -0.000000000000000000, 1.000000000000000000, 0.000000000000000000 ) ) ;
#18124 = CARTESIAN_POINT ( 'NONE',  ( -15.44795072159999982, -101.4309506800000094, 4.757508573860000034 ) ) ;
#18125 = CARTESIAN_POINT ( 'NONE',  ( 27.76234330132245276, -68.29340503348747404, 2.076308288554540304 ) ) ;
#18126 = CARTESIAN_POINT ( 'NONE',  ( 12.69538180190852295, -96.41991180888999224, 17.27318304392874282 ) ) ;
#18127 = AXIS2_PLACEMENT_3D ( 'NONE', #426, #7561, #27071 ) ;
#18128 = VECTOR ( 'NONE', #8355, 1000.000000000000000 ) ;
#18129 = CARTESIAN_POINT ( 'NONE',  ( -26.69293917519999937, -29.89689110870000022, -48.86109741659999628 ) ) ;
#18130 = DIRECTION ( 'NONE',  ( 0.000000000000000000, 1.000000000000000000, 0.000000000000000000 ) ) ;
#18131 = CARTESIAN_POINT ( 'NONE',  ( 20.06309763089999620, -36.00000000000000000, -9.476129751679998492 ) ) ;
#18132 = CARTESIAN_POINT ( 'NONE',  ( -10.60770804610000084, -19.15810967940000253, 19.29995473580000009 ) ) ;
#18133 = ORIENTED_EDGE ( 'NONE', *, *, #4842, .T. ) ;
#18134 = EDGE_CURVE ( 'NONE', #22342, #11594, #11286, .T. ) ;
#18135 = CARTESIAN_POINT ( 'NONE',  ( 36.29507663750000290, -74.81267993790000048, -14.94134320780000103 ) ) ;
#18136 = EDGE_CURVE ( 'NONE', #1612, #18945, #9668, .T. ) ;
#18137 = CARTESIAN_POINT ( 'NONE',  ( 22.48362994130000203, -95.75647260700000629, -0.6182000987479999710 ) ) ;
#18138 = CARTESIAN_POINT ( 'NONE',  ( -41.00000000000000000, -74.00000000000000000, -10.20110288159999890 ) ) ;
#18139 = CARTESIAN_POINT ( 'NONE',  ( 0.000000000000000000, -57.47855601759999900, 0.000000000000000000 ) ) ;
#18140 = PLANE ( 'NONE',  #19498 ) ;
#18141 = CARTESIAN_POINT ( 'NONE',  ( 21.87044453209999872, -37.95525411010000028, -8.597789012979999868 ) ) ;
#18142 = AXIS2_PLACEMENT_3D ( 'NONE', #8442, #14991, #26238 ) ;
#18143 = AXIS2_PLACEMENT_3D ( 'NONE', #8927, #26872, #22507 ) ;
#18144 = DIRECTION ( 'NONE',  ( 0.000000000000000000, 0.000000000000000000, -1.000000000000000000 ) ) ;
#18145 = ORIENTED_EDGE ( 'NONE', *, *, #27784, .F. ) ;
#18146 = CARTESIAN_POINT ( 'NONE',  ( -7.215414233289999757, -74.50000000000000000, -40.70731707320000226 ) ) ;
#18147 = DIRECTION ( 'NONE',  ( 0.000000000000000000, 1.000000000000000000, 0.000000000000000000 ) ) ;
#18148 = CARTESIAN_POINT ( 'NONE',  ( -21.85149396670000144, -95.71128647580000859, -5.653426733619999922 ) ) ;
#18149 = EDGE_LOOP ( 'NONE', ( #8988, #5899, #15765, #10113 ) ) ;
#18150 = CARTESIAN_POINT ( 'NONE',  ( -13.04239910971960015, -66.15241698556883421, -22.07654756397324292 ) ) ;
#18151 = B_SPLINE_CURVE_WITH_KNOTS ( 'NONE', 3,
 ( #10562, #7859, #25777, #21259, #25493, #3900, #16741, #16887, #28366, #16600, #12482, #25635, #12763, #21674, #14546, #17157, #8258, #23452, #1724, #3353, #19351, #5932, #26046, #10155, #12217, #19074, #3489, #10295, #21395, #14953, #1452, #1185, #5666, #12349, #23860, #6073 ),
 .UNSPECIFIED., .F., .F.,
 ( 4, 2, 2, 1, 1, 1, 1, 2, 2, 2, 1, 1, 1, 1, 2, 2, 2, 1, 1, 1, 1, 2, 2, 4 ),
 ( 0.000000000000000000, 0.1250000000000244804, 0.1875000000000347777, 0.2187500000000399125, 0.2343750000000394962, 0.2421875000000392741, 0.2460937500000396905, 0.2480468750000404121, 0.2500000000000411338, 0.3750000000000714429, 0.4375000000000848766, 0.4687500000000905942, 0.4843750000000933142, 0.4921875000000928702, 0.4960937500000925926, 0.5000000000000922595, 0.6250000000000517364, 0.6875000000000291989, 0.7187500000000193179, 0.7343750000000142109, 0.7421875000000096589, 0.7460937500000072164, 0.7500000000000047740, 1.000000000000000000 ),
 .UNSPECIFIED. ) ;
#18152 = CARTESIAN_POINT ( 'NONE',  ( 7.457144889719999448, -101.1889999979999999, 15.05426816870000017 ) ) ;
#18153 = DIRECTION ( 'NONE',  ( 0.000000000000000000, 1.000000000000000000, 0.000000000000000000 ) ) ;
#18154 = DIRECTION ( 'NONE',  ( 0.000000000000000000, 1.000000000000000000, 0.000000000000000000 ) ) ;
#18155 = B_SPLINE_CURVE_WITH_KNOTS ( 'NONE', 5,
 ( #2455, #10706, #28512, #132, #6362, #4626, #17593, #8678, #12899, #17886, #15227, #9127 ),
 .UNSPECIFIED., .F., .F.,
 ( 6, 3, 3, 6 ),
 ( 0.000000000000000000, 0.1767099789820964495, 0.4698587576253994702, 1.000000000000000000 ),
 .UNSPECIFIED. ) ;
#18156 = CARTESIAN_POINT ( 'NONE',  ( 0.000000000000000000, -12.64149019679999952, 0.000000000000000000 ) ) ;
#18157 = CARTESIAN_POINT ( 'NONE',  ( -7.221517031004696108, -73.63371395845983614, -39.35783505872542776 ) ) ;
#18158 = CARTESIAN_POINT ( 'NONE',  ( 19.61197036049999909, -18.61786835250000038, 9.515235106480000482 ) ) ;
#18159 = CARTESIAN_POINT ( 'NONE',  ( -21.43328945980000100, -64.24504445130001784, 15.59674557630000180 ) ) ;
#18160 = CARTESIAN_POINT ( 'NONE',  ( -16.72707404650564200, -98.26662831810237719, 9.119458534568265051 ) ) ;
#18161 = ORIENTED_EDGE ( 'NONE', *, *, #23439, .T. ) ;
#18163 = EDGE_CURVE ( 'NONE', #26221, #9130, #9450, .T. ) ;
#18162 = CARTESIAN_POINT ( 'NONE',  ( -12.63785399150000011, -72.17920235959999786, -25.42231943180000187 ) ) ;
#18164 = DIRECTION ( 'NONE',  ( 0.000000000000000000, -1.000000000000000000, 0.000000000000000000 ) ) ;
#18165 = CARTESIAN_POINT ( 'NONE',  ( 22.35420107259999867, -19.50000000000000000, 9.881343484100000296 ) ) ;
#18166 = AXIS2_PLACEMENT_3D ( 'NONE', #2184, #11, #8858 ) ;
#18167 = CARTESIAN_POINT ( 'NONE',  ( 15.48443774817907581, -95.52016638765006462, 17.06274023349215341 ) ) ;
#18168 = EDGE_LOOP ( 'NONE', ( #16598, #1457, #19213, #975 ) ) ;
#18169 = TOROIDAL_SURFACE ( 'NONE', #26542, 60.85000000000000142, 0.5000000000000000000 ) ;
#18170 = EDGE_CURVE ( 'NONE', #12644, #1175, #26657, .T. ) ;
#18171 = DIRECTION ( 'NONE',  ( 0.000000000000000000, 0.000000000000000000, 1.000000000000000000 ) ) ;
#18172 = ORIENTED_EDGE ( 'NONE', *, *, #14844, .T. ) ;
#18173 = DIRECTION ( 'NONE',  ( 0.000000000000000000, 1.000000000000000000, 0.000000000000000000 ) ) ;
#18174 = DIRECTION ( 'NONE',  ( 0.000000000000000000, -1.000000000000000000, 0.000000000000000000 ) ) ;
#18175 = CARTESIAN_POINT ( 'NONE',  ( -0.6492686798639999424, -95.71128647790000343, 22.56163718579999866 ) ) ;
#18176 = CARTESIAN_POINT ( 'NONE',  ( 2.585535234560000006, -94.10359775160000595, 25.24649707500000062 ) ) ;
#18177 = EDGE_LOOP ( 'NONE', ( #24464, #25934, #24244, #22164 ) ) ;
#18178 = FACE_OUTER_BOUND ( 'NONE', #2413, .T. ) ;
#18179 = ORIENTED_EDGE ( 'NONE', *, *, #21386, .F. ) ;
#18180 = CARTESIAN_POINT ( 'NONE',  ( -22.84072196045827496, -70.62850378349290281, 15.63790239815233996 ) ) ;
#18181 = FACE_OUTER_BOUND ( 'NONE', #16810, .T. ) ;
#18182 = CARTESIAN_POINT ( 'NONE',  ( 47.08865343609999599, -74.38949312799999802, -1.581891583850000060 ) ) ;
#18183 = EDGE_LOOP ( 'NONE', ( #9354, #27346, #5772, #23296 ) ) ;
#18184 = AXIS2_PLACEMENT_3D ( 'NONE', #2725, #27200, #15961 ) ;
#18185 = PLANE ( 'NONE',  #7124 ) ;
#18186 = CARTESIAN_POINT ( 'NONE',  ( -11.77059236524900676, -63.22433976061354599, 21.39084228963605483 ) ) ;
#18187 = AXIS2_PLACEMENT_3D ( 'NONE', #4067, #21705, #1756 ) ;
#18188 = AXIS2_PLACEMENT_3D ( 'NONE', #14268, #1446, #14409 ) ;
#18189 = ADVANCED_FACE ( 'NONE', ( #20769 ), #8068, .F. ) ;
#18190 = CARTESIAN_POINT ( 'NONE',  ( 30.45033996220000105, -72.00000000000000000, 1.805359716810000181 ) ) ;
#18191 = CARTESIAN_POINT ( 'NONE',  ( -13.23488380210000059, -93.86380869100000268, -21.19624334839999946 ) ) ;
#18192 = DIRECTION ( 'NONE',  ( 0.000000000000000000, -1.000000000000000000, 0.000000000000000000 ) ) ;
#18193 = ORIENTED_EDGE ( 'NONE', *, *, #3226, .F. ) ;
#18194 = CARTESIAN_POINT ( 'NONE',  ( 36.80494456599999609, -74.39262779950000493, -14.59792775669999898 ) ) ;
#18195 = CARTESIAN_POINT ( 'NONE',  ( -2.790536503729999840, -64.24504439390000243, -26.36014981959999659 ) ) ;
#18196 = CARTESIAN_POINT ( 'NONE',  ( -40.70731707320000226, -74.50000000000000000, 7.215414233289999757 ) ) ;
#18197 = CARTESIAN_POINT ( 'NONE',  ( -21.98017993790000091, -74.00000000020000357, -32.02104148659999794 ) ) ;
#18198 = EDGE_LOOP ( 'NONE', ( #16043, #4820, #6480, #20377 ) ) ;
#18199 = CARTESIAN_POINT ( 'NONE',  ( 11.87191034930000022, -15.14308496720000008, 21.73138612759999688 ) ) ;
#18200 = CARTESIAN_POINT ( 'NONE',  ( -38.48433347315514652, -65.11310065233233502, 2.895796419436823754 ) ) ;
#18201 = CARTESIAN_POINT ( 'NONE',  ( -18.19560383140000326, -18.61776472269999871, 11.73914725620000077 ) ) ;
#18202 = ORIENTED_EDGE ( 'NONE', *, *, #23094, .T. ) ;
#18204 = ADVANCED_FACE ( 'NONE', ( #7518 ), #21322, .T. ) ;
#18203 = CARTESIAN_POINT ( 'NONE',  ( -13.14594991939999957, -93.06131880550000801, -23.62747753289999864 ) ) ;
#18205 = CARTESIAN_POINT ( 'NONE',  ( 23.63615965700000032, -94.63960343439998724, -2.179844538739999837 ) ) ;
#18206 = DIRECTION ( 'NONE',  ( 0.3390050494208429743, 0.7071067811866730279, 0.6205445805637129775 ) ) ;
#18207 = CARTESIAN_POINT ( 'NONE',  ( 15.64127366367332961, -101.5409490182698136, 3.743084204742448851 ) ) ;
#18208 = CARTESIAN_POINT ( 'NONE',  ( 45.84677419350000349, -73.50000000000000000, -4.286925650119999709 ) ) ;
#18209 = ORIENTED_EDGE ( 'NONE', *, *, #4159, .F. ) ;
#18210 = CARTESIAN_POINT ( 'NONE',  ( 47.25120369400000442, -79.35618804639999269, -0.8986897406489999796 ) ) ;
#18211 = AXIS2_PLACEMENT_3D ( 'NONE', #18992, #18861, #16522 ) ;
#18212 = LINE ( 'NONE', #464, #11707 ) ;
#18213 = CIRCLE ( 'NONE', #26125, 3.750000000000000000 ) ;
#18214 = AXIS2_PLACEMENT_3D ( 'NONE', #20156, #226, #18122 ) ;
#18215 = CARTESIAN_POINT ( 'NONE',  ( -11.76511348380000044, -63.41220263479998920, -21.95613077419999826 ) ) ;
#18216 = FACE_OUTER_BOUND ( 'NONE', #27332, .T. ) ;
#18217 = CARTESIAN_POINT ( 'NONE',  ( 7.561439849066408314, -93.25520180122281033, 27.12672954078378851 ) ) ;
#18218 = EDGE_LOOP ( 'NONE', ( #23879, #19496, #20083, #6939 ) ) ;
#18219 = CARTESIAN_POINT ( 'NONE',  ( -12.00297273912186391, -70.31047685921210189, -25.86267369459898191 ) ) ;
#18220 = VERTEX_POINT ( 'NONE', #8064 ) ;
#18221 = CARTESIAN_POINT ( 'NONE',  ( -11.04737574249999987, -49.87551312379999757, 20.28213158860000220 ) ) ;
#18222 = CARTESIAN_POINT ( 'NONE',  ( 7.105427357599999217E-15, -69.00000000000000000, -33.25000000000000000 ) ) ;
#18223 = ORIENTED_EDGE ( 'NONE', *, *, #331, .T. ) ;
#18224 = CARTESIAN_POINT ( 'NONE',  ( -9.356041104380000917, -74.00000000000000000, 37.60355029590000697 ) ) ;
#18225 = EDGE_CURVE ( 'NONE', #27146, #18344, #5731, .T. ) ;
#18226 = CARTESIAN_POINT ( 'NONE',  ( 3.258717473867890124, -93.08494709823048652, -28.91753983529492444 ) ) ;
#18227 = CARTESIAN_POINT ( 'NONE',  ( -25.14533482850000112, -93.65023913320000304, -2.072137388280000270 ) ) ;
#18228 = CARTESIAN_POINT ( 'NONE',  ( -17.05468887140000334, -99.57787288160000116, 3.230412712340000159 ) ) ;
#18229 = CARTESIAN_POINT ( 'NONE',  ( -41.45000000000000284, -65.14977478849999670, -2.857883832489999776 ) ) ;
#18230 = VECTOR ( 'NONE', #18399, 1000.000000000000000 ) ;
#18231 = CARTESIAN_POINT ( 'NONE',  ( 11.63638030983188543, -98.17436949440750027, -16.68664549751153814 ) ) ;
#18232 = ORIENTED_EDGE ( 'NONE', *, *, #27023, .T. ) ;
#18233 = LINE ( 'NONE', #6575, #14832 ) ;
#18234 = CARTESIAN_POINT ( 'NONE',  ( -38.02515296818213386, -65.73345158630895924, -0.9555180510348912915 ) ) ;
#18235 = CARTESIAN_POINT ( 'NONE',  ( -12.51597748458882187, -92.53260370674736635, 27.81370878362392673 ) ) ;
#18236 = ORIENTED_EDGE ( 'NONE', *, *, #899, .F. ) ;
#18237 = B_SPLINE_CURVE_WITH_KNOTS ( 'NONE', 3,
 ( #17637, #15423, #24334, #11493, #18072, #2645 ),
 .UNSPECIFIED., .F., .F.,
 ( 4, 2, 4 ),
 ( 0.000000000000000000, 0.5000000000000000000, 1.000000000000000000 ),
 .UNSPECIFIED. ) ;
#18238 = EDGE_CURVE ( 'NONE', #15673, #25924, #19669, .T. ) ;
#18239 = CARTESIAN_POINT ( 'NONE',  ( -14.42556421679999978, -92.50000000000000000, -2.978755036369999942 ) ) ;
#18240 = DIRECTION ( 'NONE',  ( 0.8775825618903722036, 0.000000000000000000, 0.4794255386042040601 ) ) ;
#18241 = FACE_OUTER_BOUND ( 'NONE', #22516, .T. ) ;
#18242 = ORIENTED_EDGE ( 'NONE', *, *, #2092, .T. ) ;
#18243 = CARTESIAN_POINT ( 'NONE',  ( 3.883346862689999845, -16.50000000000000000, 7.108418751309999450 ) ) ;
#18244 = CARTESIAN_POINT ( 'NONE',  ( 0.4053730124380000022, -99.88067631459999518, -17.33742933230000105 ) ) ;
#18245 = CARTESIAN_POINT ( 'NONE',  ( -8.047735417340286190, -99.62767017965474281, 15.35597723112435986 ) ) ;
#18246 = CARTESIAN_POINT ( 'NONE',  ( -27.68682485439999752, -17.30000000000000071, -50.68039294919999804 ) ) ;
#18247 = CARTESIAN_POINT ( 'NONE',  ( -14.72614960323499922, -74.20703269541404268, 36.28169309294055012 ) ) ;
#18248 = CIRCLE ( 'NONE', #16436, 8.099999999999999645 ) ;
#18249 = CARTESIAN_POINT ( 'NONE',  ( 26.68454220230000118, -66.39602363720000255, 1.565571359830000064 ) ) ;
#18250 = AXIS2_PLACEMENT_3D ( 'NONE', #18631, #27374, #20522 ) ;
#18251 = AXIS2_PLACEMENT_3D ( 'NONE', #6746, #11382, #13731 ) ;
#18252 = ORIENTED_EDGE ( 'NONE', *, *, #11498, .T. ) ;
#18253 = CARTESIAN_POINT ( 'NONE',  ( -39.22862632829222918, -73.58711170889174014, -7.208933142661926752 ) ) ;
#18254 = CARTESIAN_POINT ( 'NONE',  ( 15.74335372269999844, -101.6484611540000031, 2.854262350110000401 ) ) ;
#18255 = CARTESIAN_POINT ( 'NONE',  ( 10.22067991429999978, -99.82967889459999355, 14.73214614719999815 ) ) ;
#18256 = ORIENTED_EDGE ( 'NONE', *, *, #12834, .T. ) ;
#18257 = CARTESIAN_POINT ( 'NONE',  ( 7.248115120159999591, -74.24284936579999794, 40.37845838710000379 ) ) ;
#18258 = CARTESIAN_POINT ( 'NONE',  ( 47.09727354990000237, -74.46036430799999550, -1.896414880740000086 ) ) ;
#18259 = DIRECTION ( 'NONE',  ( 0.000000000000000000, -1.000000000000000000, 0.000000000000000000 ) ) ;
#18260 = B_SPLINE_SURFACE_WITH_KNOTS ( 'NONE', 5, 5, ( 
 ( #21212, #28602, #18524, #4886, #14022, #5428, #7901, #22932, #949 ),
 ( #27444, #14313, #18696, #18972, #27595, #5141, #2971, #9641, #16779 ),
 ( #25675, #16636, #3390, #7489, #14586, #5292, #23487, #3118, #9502 ),
 ( #25530, #18548, #27295, #1088, #7635, #9788, #16198, #21164, #20887 ),
 ( #16502, #3527, #14453, #25111, #10060, #14178, #23073, #23208, #3258 ),
 ( #12111, #21029, #20590, #9926, #23345, #19384, #24036, #10600, #24189 ),
 ( #26237, #3938, #19246, #5839, #17198, #28552, #14722, #21574, #1630 ),
 ( #28404, #12943, #28135, #26374, #12802, #28262, #17490, #17344, #21856 ),
 ( #12522, #10749, #14990, #19519, #23759, #8295, #15127, #12662, #1907 ),
 ( #10468, #23902, #6263, #3659, #4075, #10331, #10195, #23617, #19661 ),
 ( #21434, #8587, #8441, #15269, #25816, #14856, #26087, #25947, #12384 ),
 ( #21712, #21296, #5970, #1347, #6115, #19111, #1761, #17055, #1493 ) ),
 .UNSPECIFIED., .F., .F., .F.,
 ( 6, 3, 3, 6 ),
 ( 6, 3, 6 ),
 ( 3.065779847589999996, 3.494148935390000155, 4.204781552860000104, 5.489916222159999748 ),
 ( 0.000000000000000000, 1.000000000000000000, 2.000000000000000000 ),
 .UNSPECIFIED. ) ;
#18261 = CARTESIAN_POINT ( 'NONE',  ( 22.17252228646381340, -19.46530601809573824, 0.2404182486420052278 ) ) ;
#18262 = CARTESIAN_POINT ( 'NONE',  ( -7.525338988669999729, -101.1976625110000043, 14.51486394580000017 ) ) ;
#18263 =( NAMED_UNIT ( * ) PLANE_ANGLE_UNIT ( ) SI_UNIT ( $, .RADIAN. ) );
#18264 = CARTESIAN_POINT ( 'NONE',  ( -20.69822367649999961, -60.21448500349999478, 14.94573686989999928 ) ) ;
#18265 = CARTESIAN_POINT ( 'NONE',  ( 8.509936819460000024, -37.33446438219999663, -21.72762629869999884 ) ) ;
#18266 = CARTESIAN_POINT ( 'NONE',  ( 8.613618054504685873, -19.47920864798205187, -19.98378909640561929 ) ) ;
#18267 = ORIENTED_EDGE ( 'NONE', *, *, #2181, .F. ) ;
#18268 = ADVANCED_FACE ( 'NONE', ( #3969 ), #1518, .T. ) ;
#18269 = CARTESIAN_POINT ( 'NONE',  ( 8.435807852960000019, -99.08524068509998983, 16.22846277789999903 ) ) ;
#18270 = AXIS2_PLACEMENT_3D ( 'NONE', #17497, #7943, #12298 ) ;
#18271 = DIRECTION ( 'NONE',  ( 0.000000000000000000, 1.000000000000000000, 0.000000000000000000 ) ) ;
#18272 = CARTESIAN_POINT ( 'NONE',  ( -5.478138399269999681, -95.60035679220000304, -21.87686786650000315 ) ) ;
#18273 = CARTESIAN_POINT ( 'NONE',  ( -2.557268395391378846, -19.48549492419126494, -23.46282872328029612 ) ) ;
#18274 = ADVANCED_FACE ( 'NONE', ( #8324 ), #7620, .F. ) ;
#18275 = CARTESIAN_POINT ( 'NONE',  ( 11.15108561449999947, -100.9197086960000007, -10.94438850839999944 ) ) ;
#18276 = CIRCLE ( 'NONE', #4774, 0.3500000000000003664 ) ;
#18277 = CARTESIAN_POINT ( 'NONE',  ( -29.41275679339999982, -25.00000000000000000, -53.83969017199999740 ) ) ;
#18278 = CARTESIAN_POINT ( 'NONE',  ( 12.70280709945315145, -96.41616466973447075, 17.27373141714811666 ) ) ;
#18279 = EDGE_CURVE ( 'NONE', #15375, #20678, #18445, .T. ) ;
#18280 = LINE ( 'NONE', #27169, #10436 ) ;
#18281 = CARTESIAN_POINT ( 'NONE',  ( -16.67828388959999941, -79.50000000000000000, 44.75374114529999758 ) ) ;
#18282 = CARTESIAN_POINT ( 'NONE',  ( -21.43329341219999762, -64.24504445130001784, 15.59675287610000005 ) ) ;
#18283 = CARTESIAN_POINT ( 'NONE',  ( 24.72975223188596061, -93.15741110475592279, -14.44177324630790871 ) ) ;
#18284 = CARTESIAN_POINT ( 'NONE',  ( 18.94592261899999741, -19.50000000000000000, -9.024080787800000891 ) ) ;
#18285 = ORIENTED_EDGE ( 'NONE', *, *, #4711, .T. ) ;
#18286 = CARTESIAN_POINT ( 'NONE',  ( 36.60104255959999620, -74.78622670140001105, -14.73083308719999884 ) ) ;
#18287 = CARTESIAN_POINT ( 'NONE',  ( -40.50000000000000000, -65.00000000000000000, 2.309401076760000393 ) ) ;
#18288 = CARTESIAN_POINT ( 'NONE',  ( -22.27690828497248887, -79.71584375156908209, -32.81592425880721464 ) ) ;
#18289 = CARTESIAN_POINT ( 'NONE',  ( 7.859829845370000179, -101.5882635180000051, 13.98896253659999900 ) ) ;
#18290 = CARTESIAN_POINT ( 'NONE',  ( -15.08135542309999977, -67.66819112809999126, 22.63088101159999610 ) ) ;
#18291 = CARTESIAN_POINT ( 'NONE',  ( 21.26630101029999764, -34.86445789710000298, -7.573067088439999317 ) ) ;
#18292 = FACE_OUTER_BOUND ( 'NONE', #18977, .T. ) ;
#18293 = COLOUR_RGB ( '', 0.66274510, 0.83137255, 0.94901961) ;
#18294 = TOROIDAL_SURFACE ( 'NONE', #21092, 33.64999999999999858, 1.250000000000000000 ) ;
#18295 = CARTESIAN_POINT ( 'NONE',  ( 26.22877582859999990, -72.82938648530000592, 11.61106434019999867 ) ) ;
#18296 = AXIS2_PLACEMENT_3D ( 'NONE', #24041, #10472, #19665 ) ;
#18297 = DIRECTION ( 'NONE',  ( 0.000000000000000000, -1.000000000000000000, 0.000000000000000000 ) ) ;
#18298 = CARTESIAN_POINT ( 'NONE',  ( -11.85289063449999958, -94.98812477599999227, -21.44324726029999795 ) ) ;
#18299 = CARTESIAN_POINT ( 'NONE',  ( 16.79922304909999653, -99.53431386179998697, 4.586272534879999974 ) ) ;
#18300 = VERTEX_POINT ( 'NONE', #10362 ) ;
#18301 = CARTESIAN_POINT ( 'NONE',  ( 29.56751773550223916, -74.29781185500684160, -25.75375116768845629 ) ) ;
#18302 = CARTESIAN_POINT ( 'NONE',  ( -23.85440681869999935, -94.57749834670001121, -4.067368795410000182 ) ) ;
#18303 = ORIENTED_EDGE ( 'NONE', *, *, #21108, .T. ) ;
#18304 = CARTESIAN_POINT ( 'NONE',  ( 9.139220208361530595, -92.82668962667709422, 29.09853360705717407 ) ) ;
#18305 = ADVANCED_FACE ( 'NONE', ( #3417 ), #11240, .T. ) ;
#18306 = CARTESIAN_POINT ( 'NONE',  ( 20.49588873659998356, -52.63280639819947737, 10.85734681379999067 ) ) ;
#18307 = B_SPLINE_CURVE_WITH_KNOTS ( 'NONE', 5,
 ( #18357, #18205, #7142, #4944, #13825, #22730 ),
 .UNSPECIFIED., .F., .F.,
 ( 6, 6 ),
 ( 0.000000000000000000, 1.000000000000000000 ),
 .UNSPECIFIED. ) ;
#18308 = CARTESIAN_POINT ( 'NONE',  ( -38.08919256720000135, -63.35440207070000440, 1.043878858160000034 ) ) ;
#18309 = AXIS2_PLACEMENT_3D ( 'NONE', #22978, #13632, #25161 ) ;
#18310 = CARTESIAN_POINT ( 'NONE',  ( 36.32450514027038935, -74.54297173968070922, -14.86961495641581266 ) ) ;
#18311 = CARTESIAN_POINT ( 'NONE',  ( 23.05497096699999915, -94.52419443349998573, -6.735187176270000187 ) ) ;
#18312 = EDGE_CURVE ( 'NONE', #103, #6607, #27625, .T. ) ;
#18313 = CARTESIAN_POINT ( 'NONE',  ( 20.68887087950000137, -111.0000000000000000, -4.764889194739999390 ) ) ;
#18314 = CARTESIAN_POINT ( 'NONE',  ( -21.88268327719999817, -66.31484486759998731, 16.13005244970000263 ) ) ;
#18315 = CARTESIAN_POINT ( 'NONE',  ( -17.53890950007582461, -96.04266803764619453, 13.15491836168024342 ) ) ;
#18316 = ORIENTED_EDGE ( 'NONE', *, *, #10785, .F. ) ;
#18317 = CARTESIAN_POINT ( 'NONE',  ( -13.03622110660000111, -71.76391764010000429, -25.00534121280000122 ) ) ;
#18318 = DIRECTION ( 'NONE',  ( 0.000000000000000000, -1.000000000000000000, 0.000000000000000000 ) ) ;
#18319 = CARTESIAN_POINT ( 'NONE',  ( -13.14566789610000086, -99.53431386179998697, -11.42099848439999832 ) ) ;
#18320 = AXIS2_PLACEMENT_3D ( 'NONE', #13805, #1021, #9865 ) ;
#18321 = CARTESIAN_POINT ( 'NONE',  ( 21.58303657365043904, -19.48524588020601556, 9.513186693407064354 ) ) ;
#18322 = CARTESIAN_POINT ( 'NONE',  ( -39.49501612540000650, -74.05258142259999943, -7.367357169149999940 ) ) ;
#18323 = ORIENTED_EDGE ( 'NONE', *, *, #8631, .F. ) ;
#18324 = CARTESIAN_POINT ( 'NONE',  ( 26.43197680980085451, -92.77481473413912738, -15.21859952970796037 ) ) ;
#18325 = ORIENTED_EDGE ( 'NONE', *, *, #18810, .T. ) ;
#18326 = DIRECTION ( 'NONE',  ( 1.000000000000000000, 0.000000000000000000, 0.000000000000000000 ) ) ;
#18327 = CIRCLE ( 'NONE', #11803, 1.000000000000000888 ) ;
#18328 = CARTESIAN_POINT ( 'NONE',  ( 9.915197167549999691, -36.54217832150000334, -22.83075791629999785 ) ) ;
#18329 = CARTESIAN_POINT ( 'NONE',  ( 21.92880676370000259, -37.95796630400000282, -8.677144394200000832 ) ) ;
#18330 = CARTESIAN_POINT ( 'NONE',  ( 11.26907854689999944, -92.50633975910000117, 27.15731767689999998 ) ) ;
#18331 = ORIENTED_EDGE ( 'NONE', *, *, #22245, .F. ) ;
#18332 = CARTESIAN_POINT ( 'NONE',  ( -25.41320261003370717, -94.27895761423600618, -2.788869183902775717 ) ) ;
#18333 = CARTESIAN_POINT ( 'NONE',  ( -14.05779758289999926, -93.65023913340000661, -20.95137093579999998 ) ) ;
#18334 = CARTESIAN_POINT ( 'NONE',  ( 47.16974587269999830, -74.50000000000000000, -1.075755842369999993 ) ) ;
#18335 = ORIENTED_EDGE ( 'NONE', *, *, #9964, .F. ) ;
#18336 = AXIS2_PLACEMENT_3D ( 'NONE', #5540, #12230, #23184 ) ;
#18337 = CARTESIAN_POINT ( 'NONE',  ( 7.247654292434177137, -73.86170940525964568, -39.81550290722874763 ) ) ;
#18338 = FACE_OUTER_BOUND ( 'NONE', #28172, .T. ) ;
#18339 = ADVANCED_FACE ( 'NONE', ( #28582 ), #22937, .F. ) ;
#18340 = CARTESIAN_POINT ( 'NONE',  ( -2.995163666639999889, -99.62704707150000161, -17.08389978359999972 ) ) ;
#18341 = DIRECTION ( 'NONE',  ( 0.9659258262889440783, 0.000000000000000000, -0.2588190451029840911 ) ) ;
#18342 = CARTESIAN_POINT ( 'NONE',  ( -2.266663600180000238, -67.98014023149998764, -26.53490553780000027 ) ) ;
#18343 = CARTESIAN_POINT ( 'NONE',  ( -14.57294834049999821, -70.03174454519999870, 23.21865845770000192 ) ) ;
#18344 = VERTEX_POINT ( 'NONE', #22772 ) ;
#18345 = EDGE_CURVE ( 'NONE', #5924, #24500, #159, .T. ) ;
#18346 = CARTESIAN_POINT ( 'NONE',  ( 0.000000000000000000, -82.25000000000000000, -40.00000000000000000 ) ) ;
#18347 = TOROIDAL_SURFACE ( 'NONE', #5767, 21.03431122519999974, 1.000000000000000000 ) ;
#18348 = CARTESIAN_POINT ( 'NONE',  ( 13.96614599839999826, -99.72202992580000114, -9.992871978760000218 ) ) ;
#18349 = FACE_OUTER_BOUND ( 'NONE', #16500, .T. ) ;
#18350 = CARTESIAN_POINT ( 'NONE',  ( -21.99985828019999801, -74.00000000000000000, -31.89935321680000158 ) ) ;
#18351 = ORIENTED_EDGE ( 'NONE', *, *, #26829, .F. ) ;
#18352 = AXIS2_PLACEMENT_3D ( 'NONE', #5617, #21217, #16839 ) ;
#18353 = CARTESIAN_POINT ( 'NONE',  ( 7.105427357599999217E-15, -69.00000000000000000, -46.75000000000000000 ) ) ;
#18354 = CARTESIAN_POINT ( 'NONE',  ( -7.879410208250000380, -99.92967571559999840, 15.46934584979999983 ) ) ;
#18355 = ORIENTED_EDGE ( 'NONE', *, *, #9744, .F. ) ;
#18356 = CARTESIAN_POINT ( 'NONE',  ( -8.359358578160000164, -94.05619169260000945, -23.03490865379999875 ) ) ;
#18357 = CARTESIAN_POINT ( 'NONE',  ( 23.70295537799999863, -94.59276292389999696, -2.111841813949999924 ) ) ;
#18358 = CARTESIAN_POINT ( 'NONE',  ( 8.986868621639999333, -35.35042264319999816, -19.48148203319999894 ) ) ;
#18359 = CARTESIAN_POINT ( 'NONE',  ( 16.62043402502380118, -100.1585711159323040, 4.330280467225621877 ) ) ;
#18360 = CARTESIAN_POINT ( 'NONE',  ( 0.000000000000000000, -82.25000000000000000, -40.00000000000000000 ) ) ;
#18361 = ORIENTED_EDGE ( 'NONE', *, *, #7055, .T. ) ;
#18362 = CARTESIAN_POINT ( 'NONE',  ( 46.55694345450000071, -80.05246764049999797, -3.671297399519999782 ) ) ;
#18363 = CIRCLE ( 'NONE', #11814, 7.249999999999999112 ) ;
#18364 = ITEM_DEFINED_TRANSFORMATION ( 'NONE', 'NONE', #23205,  #26433 ) ;
#18365 = CARTESIAN_POINT ( 'NONE',  ( -11.47349711059999855, -61.75794029829999943, -22.43277763900000110 ) ) ;
#18366 = VECTOR ( 'NONE', #210, 1000.000000000000000 ) ;
#18367 =( REPRESENTATION_RELATIONSHIP ('NONE','NONE', #26008, #19699 ) REPRESENTATION_RELATIONSHIP_WITH_TRANSFORMATION ( #16015 )SHAPE_REPRESENTATION_RELATIONSHIP( ) );
#18368 = CARTESIAN_POINT ( 'NONE',  ( 25.58501779599999892, -69.55030827429999363, -9.797057152780000777 ) ) ;
#18369 = CARTESIAN_POINT ( 'NONE',  ( 9.170936544316921513, -93.11246772311548625, 27.41354572203813689 ) ) ;
#18370 = ORIENTED_EDGE ( 'NONE', *, *, #25325, .F. ) ;
#18371 = CARTESIAN_POINT ( 'NONE',  ( 0.000000000000000000, -84.75000000000000000, 0.000000000000000000 ) ) ;
#18372 = ORIENTED_EDGE ( 'NONE', *, *, #9895, .T. ) ;
#18373 = CIRCLE ( 'NONE', #16496, 55.50192378860000275 ) ;
#18374 = CARTESIAN_POINT ( 'NONE',  ( 20.94731949980000252, -52.62618816519999854, 10.41165191600000028 ) ) ;
#18375 = CARTESIAN_POINT ( 'NONE',  ( 26.77683864449999973, -15.80000000000000071, 49.01467436490000296 ) ) ;
#18376 = VERTEX_POINT ( 'NONE', #23069 ) ;
#18377 = PLANE ( 'NONE',  #12654 ) ;
#18378 = ADVANCED_FACE ( 'NONE', ( #2813 ), #28510, .T. ) ;
#18379 = CARTESIAN_POINT ( 'NONE',  ( 7.784722820381165143, -93.99439547206506518, -24.91492963938277683 ) ) ;
#18380 = CARTESIAN_POINT ( 'NONE',  ( -10.90069029708386061, -19.46519145482681523, -19.29382020368896278 ) ) ;
#18381 = DIRECTION ( 'NONE',  ( 1.000000000000000000, 0.000000000000000000, 0.000000000000000000 ) ) ;
#18382 = ADVANCED_FACE ( 'NONE', ( #27435 ), #22486, .T. ) ;
#18383 = CARTESIAN_POINT ( 'NONE',  ( -10.47316257489999991, -19.17416318749999959, -21.16246808460000040 ) ) ;
#18384 = CARTESIAN_POINT ( 'NONE',  ( 47.22403540388852150, -79.22821869427725971, -0.7816738164049302773 ) ) ;
#18385 = ORIENTED_EDGE ( 'NONE', *, *, #15396, .T. ) ;
#18386 = FACE_OUTER_BOUND ( 'NONE', #5332, .T. ) ;
#18387 = CARTESIAN_POINT ( 'NONE',  ( -26.77683864449999973, -26.59999999999999787, -49.01467436490000296 ) ) ;
#18388 = CARTESIAN_POINT ( 'NONE',  ( 10.20110288159999890, -84.00000000000000000, -41.00000000000000000 ) ) ;
#18389 = ORIENTED_EDGE ( 'NONE', *, *, #2721, .T. ) ;
#18390 = CARTESIAN_POINT ( 'NONE',  ( -41.75000000000000000, -65.14977478849999670, 2.684678751729999480 ) ) ;
#18391 = CARTESIAN_POINT ( 'NONE',  ( 0.000000000000000000, -12.64149019679999952, 0.000000000000000000 ) ) ;
#18392 = CARTESIAN_POINT ( 'NONE',  ( 7.649154837969999399, -64.64960695860000328, -23.76019412080000137 ) ) ;
#18393 = ORIENTED_EDGE ( 'NONE', *, *, #15947, .F. ) ;
#18394 = CARTESIAN_POINT ( 'NONE',  ( -16.57262828550000222, -99.75088961650000385, 6.665555775249999648 ) ) ;
#18395 = B_SPLINE_CURVE_WITH_KNOTS ( 'NONE', 3,
 ( #12399, #25834, #5856, #8459 ),
 .UNSPECIFIED., .F., .F.,
 ( 4, 4 ),
 ( 0.000000000000000000, 1.000000000000000000 ),
 .UNSPECIFIED. ) ;
#18396 = AXIS2_PLACEMENT_3D ( 'NONE', #10357, #14742, #10220 ) ;
#18397 = CARTESIAN_POINT ( 'NONE',  ( -19.32502251940000448, -45.98073373379999396, 13.48194705230000068 ) ) ;
#18398 = CARTESIAN_POINT ( 'NONE',  ( -26.77683864449999973, -15.80000000000000071, -49.01467436490000296 ) ) ;
#18399 = DIRECTION ( 'NONE',  ( 0.000000000000000000, 1.000000000000000000, 0.000000000000000000 ) ) ;
#18400 = DIRECTION ( 'NONE',  ( 0.000000000000000000, 1.000000000000000000, 0.000000000000000000 ) ) ;
#18401 = ADVANCED_FACE ( 'NONE', ( #26997 ), #13160, .T. ) ;
#18402 = CARTESIAN_POINT ( 'NONE',  ( 9.119802927630001221, -98.28914429610000525, 16.69368728350000097 ) ) ;
#18403 = ORIENTED_EDGE ( 'NONE', *, *, #20275, .F. ) ;
#18404 = CARTESIAN_POINT ( 'NONE',  ( 10.41045773099999927, -35.99999999980000354, -21.22141853569999981 ) ) ;
#18405 = CARTESIAN_POINT ( 'NONE',  ( -19.47573906445313696, -18.50000000000000000, 15.05374977158872163 ) ) ;
#18406 = CONICAL_SURFACE ( 'NONE', #11894, 58.55000000000003979, 0.7853981633970000820 ) ;
#18407 = CARTESIAN_POINT ( 'NONE',  ( 8.099918789429999322, -100.8733985849999897, 13.47813349329999966 ) ) ;
#18408 = EDGE_LOOP ( 'NONE', ( #3890, #21145, #14547, #4259 ) ) ;
#18409 = CARTESIAN_POINT ( 'NONE',  ( -40.00000000000000000, -69.50000000000000000, 0.000000000000000000 ) ) ;
#18410 = CARTESIAN_POINT ( 'NONE',  ( 8.020103622739998883, -18.50000000000000000, -18.94130590319999996 ) ) ;
#18411 = DIRECTION ( 'NONE',  ( 0.000000000000000000, 1.000000000000000000, 0.000000000000000000 ) ) ;
#18412 = CARTESIAN_POINT ( 'NONE',  ( -13.25045755180000029, -111.0000000000000000, -10.32789304109999939 ) ) ;
#18413 = CARTESIAN_POINT ( 'NONE',  ( -11.18981136662480402, -93.70622791291684450, -23.36782803959924237 ) ) ;
#18414 = CARTESIAN_POINT ( 'NONE',  ( 9.212446728010000641, -35.92148816550000134, -19.60212694180000170 ) ) ;
#18415 = CARTESIAN_POINT ( 'NONE',  ( 7.734359568749999525, -19.46510050329999686, -20.63161913629999944 ) ) ;
#18416 = ORIENTED_EDGE ( 'NONE', *, *, #19311, .T. ) ;
#18417 = CARTESIAN_POINT ( 'NONE',  ( -40.01432744643470585, -73.98707088488757222, 7.250083186823315984 ) ) ;
#18418 = CARTESIAN_POINT ( 'NONE',  ( 24.52276133189999996, -18.50000000000000000, 2.134003991790000221 ) ) ;
#18419 = CARTESIAN_POINT ( 'NONE',  ( -3.701677221209999757, -96.58372172920000764, -20.98007619770000076 ) ) ;
#18420 = EDGE_LOOP ( 'NONE', ( #9429, #16998, #18431, #6113 ) ) ;
#18421 = CARTESIAN_POINT ( 'NONE',  ( 1.776356839399999804E-15, -82.50000000000000000, 2.375877272699999867E-15 ) ) ;
#18422 = CARTESIAN_POINT ( 'NONE',  ( 11.87346201969999981, -101.4334236450000049, -10.82497022220000105 ) ) ;
#18423 = CARTESIAN_POINT ( 'NONE',  ( -2.578307999469999778, -52.56313962710000709, -25.11373953509999879 ) ) ;
#18424 = CARTESIAN_POINT ( 'NONE',  ( -19.02660535542675646, -98.07566646017912149, -7.555665490820644870 ) ) ;
#18425 = CARTESIAN_POINT ( 'NONE',  ( -38.06642932020803016, -65.74109364176703707, 1.008752819234915332 ) ) ;
#18426 = CIRCLE ( 'NONE', #9570, 0.5000000000000004441 ) ;
#18427 = CARTESIAN_POINT ( 'NONE',  ( -40.00000000000000000, -63.40192378860000133, 0.000000000000000000 ) ) ;
#18428 = CARTESIAN_POINT ( 'NONE',  ( 22.02398067749999910, -53.29009989779999756, -7.952618468089998949 ) ) ;
#18429 = CARTESIAN_POINT ( 'NONE',  ( -41.00000000000000000, -84.00000000000000000, 10.20110288159999890 ) ) ;
#18430 = CARTESIAN_POINT ( 'NONE',  ( -14.81560312809999935, -101.2530993080000030, 3.374019831970000105 ) ) ;
#18431 = ORIENTED_EDGE ( 'NONE', *, *, #22382, .F. ) ;
#18432 = EDGE_CURVE ( 'NONE', #26232, #16270, #2447, .T. ) ;
#18433 = CARTESIAN_POINT ( 'NONE',  ( 6.638698704379999427, -101.1284992150000051, 13.90181459059999902 ) ) ;
#18434 = FACE_OUTER_BOUND ( 'NONE', #99, .T. ) ;
#18435 = CARTESIAN_POINT ( 'NONE',  ( 8.042004129799998680, -100.9405349759999950, 13.76814388520000065 ) ) ;
#18436 = AXIS2_PLACEMENT_3D ( 'NONE', #3307, #25595, #22985 ) ;
#18437 = EDGE_CURVE ( 'NONE', #1187, #24664, #19229, .T. ) ;
#18438 = CARTESIAN_POINT ( 'NONE',  ( 23.58467321619999879, -94.98812477769999418, -2.405347530869999861 ) ) ;
#18439 = CARTESIAN_POINT ( 'NONE',  ( 19.94240929510000271, -34.98557214560000261, -8.964904971799999345 ) ) ;
#18440 = CARTESIAN_POINT ( 'NONE',  ( 7.248366623731350877, -73.88016183364510425, 39.84605369636854988 ) ) ;
#18441 = EDGE_CURVE ( 'NONE', #12661, #22026, #25293, .T. ) ;
#18442 = DIRECTION ( 'NONE',  ( 0.000000000000000000, -1.000000000000000000, 0.000000000000000000 ) ) ;
#18443 = CARTESIAN_POINT ( 'NONE',  ( 21.81705090039999817, -37.95267571900000547, -8.514971793249999976 ) ) ;
#18444 = CARTESIAN_POINT ( 'NONE',  ( 0.4008318592790000578, -92.76843000840000286, -30.33740225879999741 ) ) ;
#18445 = B_SPLINE_CURVE_WITH_KNOTS ( 'NONE', 5,
 ( #6145, #3686, #21741, #27751, #12550, #21604, #1791, #12830, #21464 ),
 .UNSPECIFIED., .F., .F.,
 ( 6, 3, 6 ),
 ( 0.000000000000000000, 1.237573681330000008, 1.566718891470000097 ),
 .UNSPECIFIED. ) ;
#18446 = DIRECTION ( 'NONE',  ( 0.000000000000000000, -1.000000000000000000, 0.000000000000000000 ) ) ;
#18447 = CARTESIAN_POINT ( 'NONE',  ( 16.24108910990000254, -99.94549701829998867, 4.679412117860000109 ) ) ;
#18448 = VERTEX_POINT ( 'NONE', #12652 ) ;
#18449 = CARTESIAN_POINT ( 'NONE',  ( -32.56304129029999217, -80.37807044109999310, -21.91706417159999987 ) ) ;
#18450 = CARTESIAN_POINT ( 'NONE',  ( 0.000000000000000000, -65.07443093669999712, 0.000000000000000000 ) ) ;
#18451 = ORIENTED_EDGE ( 'NONE', *, *, #976, .T. ) ;
#18452 = CARTESIAN_POINT ( 'NONE',  ( -30.46635619948354190, -92.59033770620612813, 1.439011912417819783 ) ) ;
#18453 = VERTEX_POINT ( 'NONE', #3521 ) ;
#18454 = FACE_OUTER_BOUND ( 'NONE', #7507, .T. ) ;
#18455 = DIRECTION ( 'NONE',  ( -0.8775825618903722036, 0.000000000000000000, 0.4794255386042041156 ) ) ;
#18456 = DIRECTION ( 'NONE',  ( 0.3687499999999825917, 0.000000000000000000, -0.9295286103719523352 ) ) ;
#18457 = CARTESIAN_POINT ( 'NONE',  ( -7.249313954213982392, -73.91187068844764951, -39.89765284858961536 ) ) ;
#18458 = CARTESIAN_POINT ( 'NONE',  ( -14.59919359709999931, -74.45413981500000489, 36.80099833719999936 ) ) ;
#18459 = FACE_OUTER_BOUND ( 'NONE', #15517, .T. ) ;
#18460 = CARTESIAN_POINT ( 'NONE',  ( 23.82963719045704920, -92.77521214511682501, -19.03680056186108160 ) ) ;
#18461 = ORIENTED_EDGE ( 'NONE', *, *, #352, .T. ) ;
#18462 = CARTESIAN_POINT ( 'NONE',  ( -12.20941802519999975, -70.78179667580000967, -25.27574197309999704 ) ) ;
#18463 = CARTESIAN_POINT ( 'NONE',  ( 8.805378577759999104, -28.56548875780000074, -20.15266227960000123 ) ) ;
#18464 = DIRECTION ( 'NONE',  ( 1.000000000000000000, 0.000000000000000000, 0.000000000000000000 ) ) ;
#18465 = CARTESIAN_POINT ( 'NONE',  ( 19.69821314702292625, -19.46453794985196595, 10.02888976161207957 ) ) ;
#18466 = CARTESIAN_POINT ( 'NONE',  ( 15.89272830319999841, -101.5317765570000006, 2.499482219129999905 ) ) ;
#18467 = ORIENTED_EDGE ( 'NONE', *, *, #1032, .T. ) ;
#18468 = ORIENTED_EDGE ( 'NONE', *, *, #23659, .F. ) ;
#18469 = EDGE_CURVE ( 'NONE', #10333, #3863, #6235, .T. ) ;
#18470 = EDGE_CURVE ( 'NONE', #6607, #103, #12671, .T. ) ;
#18471 = B_SPLINE_CURVE_WITH_KNOTS ( 'NONE', 3,
 ( #983, #25570, #18877, #5743, #10092, #10371, #19010, #5463, #16671, #27630 ),
 .UNSPECIFIED., .F., .F.,
 ( 4, 2, 2, 2, 4 ),
 ( 0.000000000000000000, 0.2500000000000000555, 0.5000000000000001110, 0.7500000000000002220, 1.000000000000000000 ),
 .UNSPECIFIED. ) ;
#18472 = EDGE_CURVE ( 'NONE', #8384, #4012, #23607, .T. ) ;
#18473 = CARTESIAN_POINT ( 'NONE',  ( -36.23922253580000330, -80.00000000000000000, -27.04683438039999999 ) ) ;
#18474 = CARTESIAN_POINT ( 'NONE',  ( 1.338305831620000053, -94.89419512579999605, 24.43791469299999974 ) ) ;
#18475 = EDGE_CURVE ( 'NONE', #22947, #5288, #6647, .T. ) ;
#18476 = ORIENTED_EDGE ( 'NONE', *, *, #20906, .T. ) ;
#18477 = ORIENTED_EDGE ( 'NONE', *, *, #157, .F. ) ;
#18478 = CARTESIAN_POINT ( 'NONE',  ( -39.12241743810000116, -66.42264973080000345, 0.4794255386039999456 ) ) ;
#18479 = DIRECTION ( 'NONE',  ( 0.000000000000000000, 1.000000000000000000, 0.000000000000000000 ) ) ;
#18480 = CARTESIAN_POINT ( 'NONE',  ( 47.09802472229999637, -74.43779277660000560, -1.603613559539999844 ) ) ;
#18481 = EDGE_LOOP ( 'NONE', ( #25113, #4955, #9103, #10986 ) ) ;
#18482 = CARTESIAN_POINT ( 'NONE',  ( 7.248706349655917869, -74.07739338312913446, -40.14660266898284391 ) ) ;
#18483 = CARTESIAN_POINT ( 'NONE',  ( -11.72351936051625465, -62.99289890070036790, 21.32833123790344487 ) ) ;
#18484 = CARTESIAN_POINT ( 'NONE',  ( -7.325370793560000315, -74.00000000000000000, -24.94672208400000102 ) ) ;
#18485 = CARTESIAN_POINT ( 'NONE',  ( -3.546124265460000036, -70.16663891509999473, -27.89480033579999940 ) ) ;
#18486 = CARTESIAN_POINT ( 'NONE',  ( -15.33695941859999934, -70.78240035880001813, 23.26337115899999830 ) ) ;
#18487 = EDGE_LOOP ( 'NONE', ( #18576, #10602, #10013, #11640 ) ) ;
#18488 = CARTESIAN_POINT ( 'NONE',  ( 36.40080311519999867, -74.58594348169998511, -14.77956081080000139 ) ) ;
#18489 = CARTESIAN_POINT ( 'NONE',  ( -14.95917775459999888, -101.1625380809999939, 3.268662194040000024 ) ) ;
#18490 = DIRECTION ( 'NONE',  ( 0.000000000000000000, 1.000000000000000000, 0.000000000000000000 ) ) ;
#18491 = VERTEX_POINT ( 'NONE', #21425 ) ;
#18492 = DIRECTION ( 'NONE',  ( 0.2116638115179449164, 0.000000000000000000, -0.9773425350887455787 ) ) ;
#18493 = PLANE ( 'NONE',  #26711 ) ;
#18494 = CARTESIAN_POINT ( 'NONE',  ( -7.891227027390866233, -99.96200787829550904, 15.43388765503441462 ) ) ;
#18495 = ORIENTED_EDGE ( 'NONE', *, *, #14414, .F. ) ;
#18496 = CARTESIAN_POINT ( 'NONE',  ( -10.20110288159999890, -84.00000000000000000, 41.00000000000000000 ) ) ;
#18497 = CARTESIAN_POINT ( 'NONE',  ( 22.32971180670000066, -62.77692288629999240, 10.61393702059999988 ) ) ;
#18498 = DIRECTION ( 'NONE',  ( 0.000000000000000000, 1.000000000000000000, 0.000000000000000000 ) ) ;
#18499 = CARTESIAN_POINT ( 'NONE',  ( 28.07036528529999941, -39.41300778060000454, 51.38245899869999533 ) ) ;
#18500 = FACE_OUTER_BOUND ( 'NONE', #10031, .T. ) ;
#18501 = EDGE_LOOP ( 'NONE', ( #4931, #20705, #26941, #21585 ) ) ;
#18502 = CARTESIAN_POINT ( 'NONE',  ( 46.85827871259999711, -80.18254846009999426, -2.615703315070000201 ) ) ;
#18503 = EDGE_CURVE ( 'NONE', #19001, #10144, #10052, .T. ) ;
#18504 = B_SPLINE_SURFACE_WITH_KNOTS ( 'NONE', 5, 5, ( 
 ( #6668, #6363, #15681, #15534, #24586, #8679, #4336, #4627, #6521 ),
 ( #2456, #13208, #11311, #20213, #28513, #12900, #10708, #19626, #9709 ),
 ( #16422, #18029, #12036, #15831, #25182, #13654, #2742, #18330, #13796 ),
 ( #5213, #284, #13949, #6969, #7404, #14244, #20507, #427, #26927 ),
 ( #4777, #9128, #4919, #11450, #22700, #7563, #22562, #27217, #578 ),
 ( #24741, #24884, #22849, #7116, #2894, #11752, #16269, #25025, #27362 ),
 ( #25331, #7259, #9277, #20358, #16125, #11599, #5359, #5057, #20665 ),
 ( #722, #2602, #18176, #3179, #9423, #27073, #15978, #14098, #18622 ),
 ( #9573, #18474, #22996, #3047, #11898, #20808, #867, #27514, #23132 ) ),
 .UNSPECIFIED., .F., .F., .F.,
 ( 6, 3, 6 ),
 ( 6, 3, 6 ),
 ( 2.722996918069999772, 8.105704033360000338, 20.61863289369999919 ),
 ( 0.000000000000000000, 0.2500000000000000000, 0.5000000000000000000 ),
 .UNSPECIFIED. ) ;
#18505 = SHAPE_DEFINITION_REPRESENTATION ( #19666, #2018 ) ;
#18506 = CARTESIAN_POINT ( 'NONE',  ( -11.33865485209999946, -58.84796781909999908, -22.38742378179999903 ) ) ;
#18507 = CARTESIAN_POINT ( 'NONE',  ( 24.31832408829999892, -64.48635707210000589, -9.855635234570000236 ) ) ;
#18508 = CARTESIAN_POINT ( 'NONE',  ( 3.427474320454169110, -94.10913273187073003, 25.64827485542228658 ) ) ;
#18509 = EDGE_CURVE ( 'NONE', #7537, #3863, #1758, .T. ) ;
#18510 = ORIENTED_EDGE ( 'NONE', *, *, #28239, .F. ) ;
#18511 = AXIS2_PLACEMENT_3D ( 'NONE', #10378, #19295, #14898 ) ;
#18512 = CARTESIAN_POINT ( 'NONE',  ( 46.95741704872503419, -74.08013721110678773, -2.044574777238248764 ) ) ;
#18513 = VERTEX_POINT ( 'NONE', #27846 ) ;
#18514 = CARTESIAN_POINT ( 'NONE',  ( 22.48679802749999723, -53.79621871020000157, 10.10357420090000069 ) ) ;
#18515 = CARTESIAN_POINT ( 'NONE',  ( -5.641490680649999589, -101.0555477039999914, 14.43351876059999839 ) ) ;
#18516 = ORIENTED_EDGE ( 'NONE', *, *, #13572, .F. ) ;
#18517 = CARTESIAN_POINT ( 'NONE',  ( 0.000000000000000000, 0.000000000000000000, 0.000000000000000000 ) ) ;
#18518 = DIRECTION ( 'NONE',  ( -0.7071067811865474617, 0.000000000000000000, 0.7071067811865474617 ) ) ;
#18519 = ORIENTED_EDGE ( 'NONE', *, *, #357, .T. ) ;
#18520 = LINE ( 'NONE', #5816, #5980 ) ;
#18521 = CARTESIAN_POINT ( 'NONE',  ( 27.18988201479999844, -32.89844555429999673, 49.77074518290000071 ) ) ;
#18522 = FACE_OUTER_BOUND ( 'NONE', #10961, .T. ) ;
#18523 = CARTESIAN_POINT ( 'NONE',  ( -10.41327899729999906, -18.50000000000000000, -22.30433628020000114 ) ) ;
#18524 = CARTESIAN_POINT ( 'NONE',  ( 20.59810750560000159, -36.05978015090000355, -9.165578419380000952 ) ) ;
#18525 = CARTESIAN_POINT ( 'NONE',  ( 46.72518785275575937, -79.87994607672447955, -3.403393787862253550 ) ) ;
#18526 = ORIENTED_EDGE ( 'NONE', *, *, #6204, .F. ) ;
#18527 = CARTESIAN_POINT ( 'NONE',  ( 12.53708103959999853, -93.63284696309999333, -21.72543968509999956 ) ) ;
#18528 = DIRECTION ( 'NONE',  ( 0.000000000000000000, 1.000000000000000000, 0.000000000000000000 ) ) ;
#18529 = DIRECTION ( 'NONE',  ( 0.000000000000000000, 1.000000000000000000, 0.000000000000000000 ) ) ;
#18530 = ORIENTED_EDGE ( 'NONE', *, *, #22616, .T. ) ;
#18531 = B_SPLINE_CURVE_WITH_KNOTS ( 'NONE', 3,
 ( #3880, #14667, #19461, #21658, #1706, #23561, #6206, #15074 ),
 .UNSPECIFIED., .F., .F.,
 ( 4, 2, 2, 4 ),
 ( 0.000000000000000000, 0.2500000000000012212, 0.5000000000000024425, 1.000000000000000000 ),
 .UNSPECIFIED. ) ;
#18532 = CARTESIAN_POINT ( 'NONE',  ( -38.19158192515072869, -63.35070008007209452, -1.239942138225138990 ) ) ;
#18533 = DIRECTION ( 'NONE',  ( 0.4794255386042041156, 0.000000000000000000, 0.8775825618903720926 ) ) ;
#18534 = FACE_OUTER_BOUND ( 'NONE', #3605, .T. ) ;
#18535 = EDGE_LOOP ( 'NONE', ( #3770, #6306, #21625, #18635 ) ) ;
#18536 = CARTESIAN_POINT ( 'NONE',  ( -18.26810489620000055, -94.98812477769999418, 16.32728500220000001 ) ) ;
#18537 = CARTESIAN_POINT ( 'NONE',  ( -18.60084818170000176, -19.46563609400000061, 11.81582046800000008 ) ) ;
#18538 = CARTESIAN_POINT ( 'NONE',  ( 7.289196689104602278, -35.72560966896035239, -21.42683523805979462 ) ) ;
#18539 = CARTESIAN_POINT ( 'NONE',  ( 27.75394116159999669, -74.50000000000000000, -27.75394116159999669 ) ) ;
#18540 = CARTESIAN_POINT ( 'NONE',  ( -40.00000000000000000, -63.50000000000000000, 0.000000000000000000 ) ) ;
#18541 = EDGE_CURVE ( 'NONE', #16504, #4122, #15959, .T. ) ;
#18542 =( LENGTH_UNIT ( ) NAMED_UNIT ( * ) SI_UNIT ( .MILLI., .METRE. ) );
#18543 = TOROIDAL_SURFACE ( 'NONE', #3634, 6.750000000000000000, 0.5000000000000000000 ) ;
#18544 = EDGE_CURVE ( 'NONE', #6780, #4268, #6666, .T. ) ;
#18545 = ORIENTED_EDGE ( 'NONE', *, *, #8922, .T. ) ;
#18546 = CARTESIAN_POINT ( 'NONE',  ( -39.29494613580084916, -73.61009970501154953, -7.215638845197088536 ) ) ;
#18547 = CARTESIAN_POINT ( 'NONE',  ( 0.000000000000000000, -2.000000000000000000, 0.000000000000000000 ) ) ;
#18548 = CARTESIAN_POINT ( 'NONE',  ( 20.15734887640000039, -35.97442374919999963, -9.269656953000000144 ) ) ;
#18549 = CARTESIAN_POINT ( 'NONE',  ( 17.21463605679999986, -95.70830672179999965, 14.46803396139999975 ) ) ;
#18550 = ORIENTED_EDGE ( 'NONE', *, *, #23576, .F. ) ;
#18551 = DIRECTION ( 'NONE',  ( 0.000000000000000000, 1.000000000000000000, 0.000000000000000000 ) ) ;
#18552 = CARTESIAN_POINT ( 'NONE',  ( -11.21645807309999832, -18.61794787939999907, -18.51636674970000129 ) ) ;
#18553 = AXIS2_PLACEMENT_3D ( 'NONE', #13619, #15795, #22666 ) ;
#18554 = CIRCLE ( 'NONE', #901, 5.500000000000000000 ) ;
#18555 = CARTESIAN_POINT ( 'NONE',  ( 46.43423234700000535, -80.49808279690000745, -3.486565683130000259 ) ) ;
#18556 = CARTESIAN_POINT ( 'NONE',  ( 14.28941763439999946, -111.0000000000000000, -3.575252188409999921 ) ) ;
#18557 = CARTESIAN_POINT ( 'NONE',  ( -10.27834059868025207, -93.94676096557853384, -23.20073146982036860 ) ) ;
#18558 = CARTESIAN_POINT ( 'NONE',  ( 8.940781202869999333, -36.53304298860000188, -22.07739135909999817 ) ) ;
#18559 = DIRECTION ( 'NONE',  ( 0.000000000000000000, 1.000000000000000000, 0.000000000000000000 ) ) ;
#18560 = EDGE_LOOP ( 'NONE', ( #19180, #21452, #1274, #12895 ) ) ;
#18561 = CARTESIAN_POINT ( 'NONE',  ( -43.20000000000000284, -65.14977478849999670, 0.1732050807559999961 ) ) ;
#18562 = B_SPLINE_CURVE_WITH_KNOTS ( 'NONE', 3,
 ( #1748, #28392, #8575, #160, #9013, #26811 ),
 .UNSPECIFIED., .F., .F.,
 ( 4, 2, 4 ),
 ( 0.000000000000000000, 0.5000000000000000000, 1.000000000000000000 ),
 .UNSPECIFIED. ) ;
#18563 = EDGE_CURVE ( 'NONE', #4106, #11899, #17776, .T. ) ;
#18564 = CARTESIAN_POINT ( 'NONE',  ( 23.97060671510000063, -18.50000000000000000, 2.556446744250000069 ) ) ;
#18565 = CARTESIAN_POINT ( 'NONE',  ( 11.86104730819999986, -101.2306310700000012, -11.05401091329999907 ) ) ;
#18566 = ORIENTED_EDGE ( 'NONE', *, *, #21671, .T. ) ;
#18567 = CARTESIAN_POINT ( 'NONE',  ( -1.741759767157955219, -19.46809228179713713, -22.35565690618285828 ) ) ;
#18568 = PRODUCT_DEFINITION_FORMATION_WITH_SPECIFIED_SOURCE ( 'ANY', '', #13159, .NOT_KNOWN. ) ;
#18569 = CARTESIAN_POINT ( 'NONE',  ( 27.18988201479999844, -34.70155444569999759, 49.77074518290000071 ) ) ;
#18570 = CARTESIAN_POINT ( 'NONE',  ( -1.993723132860000025, -52.61368720120000120, -23.68602550419999986 ) ) ;
#18571 = CARTESIAN_POINT ( 'NONE',  ( -17.05193907084168004, -92.82668962665341894, 25.28796903711848643 ) ) ;
#18572 = DIRECTION ( 'NONE',  ( 0.9993816408608721114, 0.000000000000000000, -0.03516156865429537204 ) ) ;
#18573 = CARTESIAN_POINT ( 'NONE',  ( 20.85226889350772339, -36.17942473021693672, -9.018047964458704158 ) ) ;
#18574 = CARTESIAN_POINT ( 'NONE',  ( 21.61346702620000215, -40.75181153009999946, -7.194012074159999770 ) ) ;
#18575 = CARTESIAN_POINT ( 'NONE',  ( -40.70731707320000226, -74.50000000000000000, -7.215414233289999757 ) ) ;
#18576 = ORIENTED_EDGE ( 'NONE', *, *, #18731, .T. ) ;
#18577 = TOROIDAL_SURFACE ( 'NONE', #10152, 55.85192378860000417, 0.3499999999999999778 ) ;
#18578 = ADVANCED_FACE ( 'NONE', ( #22146 ), #15414, .T. ) ;
#18579 = EDGE_CURVE ( 'NONE', #22634, #8616, #23994, .T. ) ;
#18580 = AXIS2_PLACEMENT_3D ( 'NONE', #18819, #21271, #11949 ) ;
#18581 = CARTESIAN_POINT ( 'NONE',  ( -32.77174708420000115, -74.50000000069999828, -21.60034937769999885 ) ) ;
#18582 = CARTESIAN_POINT ( 'NONE',  ( -18.34989813179999985, -93.00000000000000000, 23.56346505449999995 ) ) ;
#18583 = AXIS2_PLACEMENT_3D ( 'NONE', #26977, #9172, #8875 ) ;
#18584 = CARTESIAN_POINT ( 'NONE',  ( -13.91383203010000003, -65.33610288280000589, 21.79517489670000074 ) ) ;
#18585 = CARTESIAN_POINT ( 'NONE',  ( 20.45837631639999898, -35.09297533480000908, -8.783856190409998987 ) ) ;
#18586 = DIRECTION ( 'NONE',  ( 0.8775825618903722036, 0.000000000000000000, -0.4794255386042041156 ) ) ;
#18587 = B_SPLINE_CURVE_WITH_KNOTS ( 'NONE', 5,
 ( #14948, #25771, #27812, #10290, #21256, #12346 ),
 .UNSPECIFIED., .F., .F.,
 ( 6, 6 ),
 ( 0.000000000000000000, 1.000000000000000000 ),
 .UNSPECIFIED. ) ;
#18588 = DIRECTION ( 'NONE',  ( -0.1770468907230370870, 0.000000000000000000, -0.9842024174352068666 ) ) ;
#18589 = CARTESIAN_POINT ( 'NONE',  ( 0.2881167279619999966, -92.51542729400000553, -30.06300816579999946 ) ) ;
#18590 = B_SPLINE_CURVE_WITH_KNOTS ( 'NONE', 3,
 ( #17879, #13644, #19756, #26779, #22400, #123, #11442, #9267, #26472, #24874, #6959, #2147, #15672, #278, #8820, #10846, #13196, #26620, #13337, #2445, #11301, #20348, #15971, #19901, #4909, #21958, #8672, #2007 ),
 .UNSPECIFIED., .F., .F.,
 ( 4, 2, 1, 1, 1, 1, 2, 2, 2, 2, 1, 1, 1, 1, 2, 2, 2, 4 ),
 ( 0.000000000000000000, 0.1250000000000460465, 0.1875000000000690559, 0.2187500000000805744, 0.2343750000000861811, 0.2421875000000865696, 0.2460937500000842382, 0.2500000000000818789, 0.3750000000000255351, 0.4374999999999959477, 0.4687499999999797939, 0.4843749999999705791, 0.4921874999999659717, 0.4960937499999635292, 0.4980468749999634737, 0.4999999999999634182, 0.7499999999999816813, 1.000000000000000000 ),
 .UNSPECIFIED. ) ;
#18591 = DIRECTION ( 'NONE',  ( 0.000000000000000000, 1.000000000000000000, 0.000000000000000000 ) ) ;
#18592 = CARTESIAN_POINT ( 'NONE',  ( 0.000000000000000000, -37.50000000000000000, 0.000000000000000000 ) ) ;
#18593 = ORIENTED_EDGE ( 'NONE', *, *, #22206, .F. ) ;
#18594 = VECTOR ( 'NONE', #22260, 1000.000000000000000 ) ;
#18595 = FILL_AREA_STYLE_COLOUR ( '', #24545 ) ;
#18596 = CARTESIAN_POINT ( 'NONE',  ( -15.60055607610000195, -99.82967635429999120, -8.838619376430001395 ) ) ;
#18597 = ORIENTED_EDGE ( 'NONE', *, *, #17702, .F. ) ;
#18598 = CARTESIAN_POINT ( 'NONE',  ( -30.42316450781055792, -92.75430643196618519, 2.164184228886041339 ) ) ;
#18599 = ORIENTED_EDGE ( 'NONE', *, *, #11114, .F. ) ;
#18600 = CIRCLE ( 'NONE', #23688, 16.00000000000000000 ) ;
#18601 = AXIS2_PLACEMENT_3D ( 'NONE', #9141, #2031, #10871 ) ;
#18602 = AXIS2_PLACEMENT_3D ( 'NONE', #283, #26926, #13206 ) ;
#18603 = CARTESIAN_POINT ( 'NONE',  ( 0.4681305316614765566, -101.2021794473764658, -16.33959806313605512 ) ) ;
#18604 = ADVANCED_FACE ( 'NONE', ( #26365 ), #8578, .T. ) ;
#18605 = CARTESIAN_POINT ( 'NONE',  ( -7.227599506459999823, -73.59185047150000969, 39.32706724020000877 ) ) ;
#18606 = CARTESIAN_POINT ( 'NONE',  ( -10.04487041370000000, -18.50000000000000000, -22.35700885240000346 ) ) ;
#18607 = DIRECTION ( 'NONE',  ( 1.000000000000000000, 0.000000000000000000, 0.000000000000000000 ) ) ;
#18608 = CARTESIAN_POINT ( 'NONE',  ( -21.83717417439999764, -67.94514003989999651, 15.21749783979999826 ) ) ;
#18609 = CARTESIAN_POINT ( 'NONE',  ( 14.19394574969999923, -96.53848370309999893, -15.96642820140000296 ) ) ;
#18610 = ORIENTED_EDGE ( 'NONE', *, *, #24844, .F. ) ;
#18611 = DIRECTION ( 'NONE',  ( 1.000000000000000000, 0.000000000000000000, 0.000000000000000000 ) ) ;
#18612 = CARTESIAN_POINT ( 'NONE',  ( 8.124863382020000913, -28.53805538430000155, -20.82664772909999940 ) ) ;
#18613 = CARTESIAN_POINT ( 'NONE',  ( -1.981473163719889241, -57.45864759319265147, -23.83876219059375501 ) ) ;
#18614 = EDGE_CURVE ( 'NONE', #8093, #23133, #16000, .T. ) ;
#18615 = CARTESIAN_POINT ( 'NONE',  ( 13.12744653600000078, -94.59276292389999696, -19.84842857619999990 ) ) ;
#18616 = ORIENTED_EDGE ( 'NONE', *, *, #14301, .T. ) ;
#18617 = VERTEX_POINT ( 'NONE', #15565 ) ;
#18618 = AXIS2_PLACEMENT_3D ( 'NONE', #10644, #19557, #24226 ) ;
#18619 = VECTOR ( 'NONE', #872, 1000.000000000000000 ) ;
#18620 = CARTESIAN_POINT ( 'NONE',  ( 27.68682485439999752, -28.69999999999999929, 50.68039294919999804 ) ) ;
#18621 = CARTESIAN_POINT ( 'NONE',  ( 1.495914020609999895, -94.52293512119999264, 23.88472631159999793 ) ) ;
#18622 = CARTESIAN_POINT ( 'NONE',  ( 2.842132195609999634, -93.86302664969998943, 24.60248089030000074 ) ) ;
#18623 = EDGE_LOOP ( 'NONE', ( #15064, #15761 ) ) ;
#18624 = DIRECTION ( 'NONE',  ( 1.000000000000000000, 0.000000000000000000, 0.000000000000000000 ) ) ;
#18625 = CARTESIAN_POINT ( 'NONE',  ( 20.64806783649999744, -36.00000000000000000, -10.29738622729999875 ) ) ;
#18626 = CARTESIAN_POINT ( 'NONE',  ( 46.84462288190000123, -73.99960224719998791, -2.454903744640000163 ) ) ;
#18627 = ORIENTED_EDGE ( 'NONE', *, *, #24110, .T. ) ;
#18628 = CARTESIAN_POINT ( 'NONE',  ( 0.000000000000000000, -91.50000000000000000, 0.000000000000000000 ) ) ;
#18629 = CARTESIAN_POINT ( 'NONE',  ( -11.43090272393724227, -61.14595846210385588, 20.91059242002400254 ) ) ;
#18630 = CARTESIAN_POINT ( 'NONE',  ( -14.69254889179999957, -80.02777972779999516, 36.39670833679999618 ) ) ;
#18631 = CARTESIAN_POINT ( 'NONE',  ( 0.000000000000000000, -91.50000000000000000, 0.000000000000000000 ) ) ;
#18632 = CARTESIAN_POINT ( 'NONE',  ( -2.733878092589999920, -65.50583529140000394, -26.26633881939999782 ) ) ;
#18633 = AXIS2_PLACEMENT_3D ( 'NONE', #17484, #24625, #4814 ) ;
#18634 = CARTESIAN_POINT ( 'NONE',  ( -15.42363691649999957, -67.46051858619999564, 22.84488648889999851 ) ) ;
#18635 = ORIENTED_EDGE ( 'NONE', *, *, #25179, .F. ) ;
#18637 = EDGE_CURVE ( 'NONE', #11899, #2616, #13199, .T. ) ;
#18636 = AXIS2_PLACEMENT_3D ( 'NONE', #23209, #3528, #12385 ) ;
#18638 = CARTESIAN_POINT ( 'NONE',  ( 36.69073705870000168, -74.41569028729999502, -14.60033862030000051 ) ) ;
#18639 = CARTESIAN_POINT ( 'NONE',  ( -16.69495928710000143, -99.99921705949999762, 3.045998530109999880 ) ) ;
#18640 = CARTESIAN_POINT ( 'NONE',  ( 24.75430904529999765, -58.88258727490000410, 1.309835822719999987 ) ) ;
#18641 = CARTESIAN_POINT ( 'NONE',  ( 19.46230083649999898, -35.13262238679999427, -8.987746796310000619 ) ) ;
#18642 = ORIENTED_EDGE ( 'NONE', *, *, #8427, .T. ) ;
#18643 = DIRECTION ( 'NONE',  ( 0.000000000000000000, -1.000000000000000000, 0.000000000000000000 ) ) ;
#18644 = EDGE_CURVE ( 'NONE', #6664, #23028, #17817, .T. ) ;
#18645 = CARTESIAN_POINT ( 'NONE',  ( -2.587000173290000316, -19.48534420260000033, -23.45837883329999940 ) ) ;
#18646 = CARTESIAN_POINT ( 'NONE',  ( 36.75513477746535074, -74.61502060571835671, -14.67454940403652586 ) ) ;
#18647 = ORIENTED_EDGE ( 'NONE', *, *, #13034, .T. ) ;
#18648 = ADVANCED_FACE ( 'NONE', ( #2636 ), #851, .T. ) ;
#18649 = CARTESIAN_POINT ( 'NONE',  ( -12.77207206940000006, -18.50000000000000000, 18.29965927990000196 ) ) ;
#18650 = DIRECTION ( 'NONE',  ( -0.9952295494196654602, 0.000000000000000000, 0.09756097560976667582 ) ) ;
#18651 = CARTESIAN_POINT ( 'NONE',  ( 8.770435442900000211, -35.38531402059999920, -20.52569425229999922 ) ) ;
#18652 = CARTESIAN_POINT ( 'NONE',  ( 16.71390024897803883, -100.0559847775274704, 4.300018913473477866 ) ) ;
#18653 = CARTESIAN_POINT ( 'NONE',  ( 19.64032610941312740, -94.52419745022692155, 13.82579366131591847 ) ) ;
#18654 = ORIENTED_EDGE ( 'NONE', *, *, #16855, .T. ) ;
#18655 = ITEM_DEFINED_TRANSFORMATION ( 'NONE', 'NONE', #21782,  #26433 ) ;
#18656 = CARTESIAN_POINT ( 'NONE',  ( -7.325370793560000315, -72.00000000000000000, -24.94672208400000102 ) ) ;
#18657 = CIRCLE ( 'NONE', #11159, 58.54999999999999716 ) ;
#18658 = DIRECTION ( 'NONE',  ( 0.000000000000000000, -1.000000000000000000, 0.000000000000000000 ) ) ;
#18659 = CARTESIAN_POINT ( 'NONE',  ( 1.731887814557739880, -94.79127258004355383, 24.69986651471424821 ) ) ;
#18660 = TOROIDAL_SURFACE ( 'NONE', #6053, 29.91857981989999971, 10.00000000000000000 ) ;
#18661 = ORIENTED_EDGE ( 'NONE', *, *, #16657, .T. ) ;
#18662 = CIRCLE ( 'NONE', #13988, 2.999999999999998224 ) ;
#18663 = CARTESIAN_POINT ( 'NONE',  ( 25.09792694589999940, -15.00000000000000000, 45.94144711499999545 ) ) ;
#18664 = FACE_OUTER_BOUND ( 'NONE', #2312, .T. ) ;
#18665 = VERTEX_POINT ( 'NONE', #22593 ) ;
#18666 = CARTESIAN_POINT ( 'NONE',  ( -17.94180966909999597, -45.73899999920000425, 18.81731824139999887 ) ) ;
#18667 = CARTESIAN_POINT ( 'NONE',  ( -6.179359521840000369, -101.4254868690000109, 14.72527176150000017 ) ) ;
#18668 = ORIENTED_EDGE ( 'NONE', *, *, #10462, .T. ) ;
#18669 = CARTESIAN_POINT ( 'NONE',  ( -19.92984078955770499, -19.50000000000000000, 15.63765909864717152 ) ) ;
#18670 = CARTESIAN_POINT ( 'NONE',  ( 4.500000000000000000, -11.00000000000000000, -50.00000000000000000 ) ) ;
#18671 = CARTESIAN_POINT ( 'NONE',  ( -10.52744371402527790, -19.48510007433630520, -21.09691113857233802 ) ) ;
#18672 = CARTESIAN_POINT ( 'NONE',  ( -12.94585355959999973, -101.6484611540000031, -9.402386697720000797 ) ) ;
#18673 = CARTESIAN_POINT ( 'NONE',  ( 2.876553231629999985, -100.0000000000000000, 5.265495371340000119 ) ) ;
#18674 = DIRECTION ( 'NONE',  ( 0.000000000000000000, -1.000000000000000000, 0.000000000000000000 ) ) ;
#18675 = ORIENTED_EDGE ( 'NONE', *, *, #3085, .T. ) ;
#18676 = ADVANCED_FACE ( 'NONE', ( #27250 ), #25267, .T. ) ;
#18677 = CARTESIAN_POINT ( 'NONE',  ( -32.77174707999999725, -79.50000000000000000, -21.60034937969999902 ) ) ;
#18678 = CARTESIAN_POINT ( 'NONE',  ( 16.79920482320000019, -99.53431242750001218, 4.586287493060000386 ) ) ;
#18679 = CARTESIAN_POINT ( 'NONE',  ( -4.500000000000000000, -12.50000000000000000, 40.50000000000000000 ) ) ;
#18680 = ORIENTED_EDGE ( 'NONE', *, *, #25228, .F. ) ;
#18681 = CIRCLE ( 'NONE', #7044, 6.000000000000000000 ) ;
#18682 = CARTESIAN_POINT ( 'NONE',  ( 29.71503696804588657, -92.89593097428453916, 6.875073252006978386 ) ) ;
#18683 = CARTESIAN_POINT ( 'NONE',  ( 9.356041104380000917, -84.00000000000000000, 37.60355029590000697 ) ) ;
#18684 = ORIENTED_EDGE ( 'NONE', *, *, #26258, .T. ) ;
#18685 = AXIS2_PLACEMENT_3D ( 'NONE', #16775, #5698, #14581 ) ;
#18686 = EDGE_CURVE ( 'NONE', #20283, #14297, #26320, .T. ) ;
#18687 = CARTESIAN_POINT ( 'NONE',  ( 4.882943008269999509E-15, -69.50000000000000000, -40.00000000000000000 ) ) ;
#18688 = CONICAL_SURFACE ( 'NONE', #22389, 1.732050807582486307, 1.047197551199999799 ) ;
#18689 = CARTESIAN_POINT ( 'NONE',  ( -20.03437290520000147, -32.66150190460000147, 14.54837859389999899 ) ) ;
#18690 = FACE_OUTER_BOUND ( 'NONE', #5469, .T. ) ;
#18691 = CARTESIAN_POINT ( 'NONE',  ( 27.75394116159999669, -74.50000000000000000, -27.75394116159999669 ) ) ;
#18692 = AXIS2_PLACEMENT_3D ( 'NONE', #4459, #13633, #9110 ) ;
#18693 = CARTESIAN_POINT ( 'NONE',  ( 23.71521856880000101, -60.21977178070000036, -9.629174062080000596 ) ) ;
#18694 = ORIENTED_EDGE ( 'NONE', *, *, #10109, .F. ) ;
#18695 = DIRECTION ( 'NONE',  ( 1.000000000000000000, 0.000000000000000000, 0.000000000000000000 ) ) ;
#18696 = CARTESIAN_POINT ( 'NONE',  ( 20.54661061919999554, -36.04663673480000341, -9.151657597179999826 ) ) ;
#18697 = DIRECTION ( 'NONE',  ( 0.000000000000000000, 1.000000000000000000, 0.000000000000000000 ) ) ;
#18698 = VERTEX_POINT ( 'NONE', #24272 ) ;
#18699 = AXIS2_PLACEMENT_3D ( 'NONE', #26578, #2115, #15330 ) ;
#18700 = PLANE ( 'NONE',  #10165 ) ;
#18701 = CARTESIAN_POINT ( 'NONE',  ( -11.34376786329999831, -18.85523522049999912, -18.72653253400000040 ) ) ;
#18702 = CIRCLE ( 'NONE', #21927, 7.249999999999999112 ) ;
#18703 = CIRCLE ( 'NONE', #1050, 21.14285714289999873 ) ;
#18704 = CYLINDRICAL_SURFACE ( 'NONE', #23752, 7.999999999999998224 ) ;
#18705 = CARTESIAN_POINT ( 'NONE',  ( 1.509903313490000218E-14, -80.00000000000000000, 40.00000000000000000 ) ) ;
#18706 = CARTESIAN_POINT ( 'NONE',  ( 0.000000000000000000, -10.50000000000000000, 0.000000000000000000 ) ) ;
#18707 = CARTESIAN_POINT ( 'NONE',  ( 10.20110288159999890, -74.00000000000000000, 41.00000000000000000 ) ) ;
#18708 = ORIENTED_EDGE ( 'NONE', *, *, #27969, .T. ) ;
#18709 = EDGE_CURVE ( 'NONE', #26262, #21465, #3472, .T. ) ;
#18710 = CARTESIAN_POINT ( 'NONE',  ( -40.53346806335466113, -74.36482065553560972, 7.230685509125985178 ) ) ;
#18711 = DIRECTION ( 'NONE',  ( 0.09756097560976997873, 0.000000000000000000, 0.9952295494196653491 ) ) ;
#18712 = FACE_OUTER_BOUND ( 'NONE', #16919, .T. ) ;
#18713 = VERTEX_POINT ( 'NONE', #12017 ) ;
#18714 = CARTESIAN_POINT ( 'NONE',  ( 19.75624615420000296, -18.86343728519999985, -8.697936434349999857 ) ) ;
#18715 = CARTESIAN_POINT ( 'NONE',  ( -29.41275679339999982, -11.79999999999999893, -53.83969017199999740 ) ) ;
#18716 = CARTESIAN_POINT ( 'NONE',  ( -0.8522615965990000264, -39.36582103130000121, -22.71500442319999991 ) ) ;
#18717 = FACE_OUTER_BOUND ( 'NONE', #1725, .T. ) ;
#18718 = ADVANCED_FACE ( 'NONE', ( #23118 ), #3164, .F. ) ;
#18719 = CARTESIAN_POINT ( 'NONE',  ( -17.94180966909999597, -72.00000000000000000, 18.81731824139999887 ) ) ;
#18720 = CONICAL_SURFACE ( 'NONE', #11294, 5.999999999999999112, 0.7853981633970000820 ) ;
#18721 = FACE_OUTER_BOUND ( 'NONE', #26820, .T. ) ;
#18722 = CARTESIAN_POINT ( 'NONE',  ( 22.46104921339999905, -40.70401306749999293, -9.175396146790001595 ) ) ;
#18723 = CARTESIAN_POINT ( 'NONE',  ( -38.79561088340664554, -74.00013394023025626, -7.600490370241675286 ) ) ;
#18724 = DIRECTION ( 'NONE',  ( 0.000000000000000000, 1.000000000000000000, 0.000000000000000000 ) ) ;
#18725 = CIRCLE ( 'NONE', #17301, 55.50192378860000275 ) ;
#18726 = EDGE_LOOP ( 'NONE', ( #2358, #19156, #26654, #10291, #15314 ) ) ;
#18727 = CARTESIAN_POINT ( 'NONE',  ( 6.882913241140000693, -101.1292389600000092, 13.89502594439999861 ) ) ;
#18728 = CARTESIAN_POINT ( 'NONE',  ( -22.00249031559999935, -74.50000000000000000, -32.67527180329999936 ) ) ;
#18729 = CARTESIAN_POINT ( 'NONE',  ( 7.588618361450000016, -101.1629257550000034, 13.79088284649999885 ) ) ;
#18730 = CARTESIAN_POINT ( 'NONE',  ( -11.23282768690000033, -95.05242829889999712, -21.31919490279999962 ) ) ;
#18731 = EDGE_CURVE ( 'NONE', #21679, #26473, #5272, .T. ) ;
#18732 = CARTESIAN_POINT ( 'NONE',  ( 21.24009719620000070, -34.72971490739999467, -7.623606132409999958 ) ) ;
#18733 = CARTESIAN_POINT ( 'NONE',  ( 36.67694313739999501, -80.46520755129999714, -13.97975614370000130 ) ) ;
#18734 = CARTESIAN_POINT ( 'NONE',  ( -7.639093477879999483, -98.53908914310000000, 17.11999108210000031 ) ) ;
#18735 = DIRECTION ( 'NONE',  ( -0.8775825618903722036, 0.000000000000000000, 0.4794255386042041156 ) ) ;
#18736 = CARTESIAN_POINT ( 'NONE',  ( -20.38264025652998512, -93.09721478938070049, -20.64447115935058719 ) ) ;
#18737 = DIRECTION ( 'NONE',  ( 1.000000000000000000, 0.000000000000000000, 0.000000000000000000 ) ) ;
#18738 = ORIENTED_EDGE ( 'NONE', *, *, #3723, .T. ) ;
#18739 = DIRECTION ( 'NONE',  ( -0.04116274481150321296, -0.9430444279530652008, 0.3301103381390215752 ) ) ;
#18740 = DIRECTION ( 'NONE',  ( -1.000000000000000000, 0.000000000000000000, 1.203338504110000538E-16 ) ) ;
#18741 = VERTEX_POINT ( 'NONE', #16103 ) ;
#18742 = CIRCLE ( 'NONE', #3387, 32.39999999999999858 ) ;
#18743 = CARTESIAN_POINT ( 'NONE',  ( -16.86265888959999870, -77.00000000000000000, 45.21850545039999503 ) ) ;
#18744 = EDGE_CURVE ( 'NONE', #3120, #21366, #16425, .T. ) ;
#18745 = EDGE_CURVE ( 'NONE', #6793, #25061, #3129, .T. ) ;
#18746 = CARTESIAN_POINT ( 'NONE',  ( -0.1779554536940000098, -101.6484611540000031, -15.99901033990000165 ) ) ;
#18747 = CARTESIAN_POINT ( 'NONE',  ( -7.588109730960000299, -73.99999952349999432, 38.87068334559999983 ) ) ;
#18748 = LINE ( 'NONE', #20794, #21533 ) ;
#18749 = CARTESIAN_POINT ( 'NONE',  ( -11.76876591429999941, -94.80026553589999594, -21.40431208230000237 ) ) ;
#18750 = CARTESIAN_POINT ( 'NONE',  ( 0.000000000000000000, -37.57799544290000426, 0.000000000000000000 ) ) ;
#18751 = PLANE ( 'NONE',  #24386 ) ;
#18752 = CARTESIAN_POINT ( 'NONE',  ( 23.90217122411711159, -92.89593097429802526, -18.94561334467121938 ) ) ;
#18753 = B_SPLINE_SURFACE_WITH_KNOTS ( 'NONE', 5, 5, ( 
 ( #4537, #28704, #26697, #24060, #8892, #15012 ),
 ( #21883, #13415, #22318, #2365, #8610, #197 ),
 ( #24501, #24359, #15447, #20127, #8464, #11219 ),
 ( #6737, #1934, #19686, #15602, #17951, #9046 ),
 ( #2080, #17806, #3963, #10920, #26543, #13120 ),
 ( #6139, #10629, #23925, #19974, #19827, #12824 ) ),
 .UNSPECIFIED., .F., .F., .F.,
 ( 6, 6 ),
 ( 6, 6 ),
 ( 13.75713939520000118, 20.91598888789999933 ),
 ( 0.000000000000000000, 2.000000000000000000 ),
 .UNSPECIFIED. ) ;
#18754 = DIRECTION ( 'NONE',  ( 1.000000000000000000, 0.000000000000000000, 0.000000000000000000 ) ) ;
#18755 = DIRECTION ( 'NONE',  ( 0.000000000000000000, 1.000000000000000000, 0.000000000000000000 ) ) ;
#18756 = FACE_OUTER_BOUND ( 'NONE', #22347, .T. ) ;
#18757 = SURFACE_STYLE_FILL_AREA ( #3172 ) ;
#18758 = ORIENTED_EDGE ( 'NONE', *, *, #3806, .F. ) ;
#18759 = LINE ( 'NONE', #27920, #3688 ) ;
#18760 = AXIS2_PLACEMENT_3D ( 'NONE', #27448, #2975, #7493 ) ;
#18761 = ORIENTED_EDGE ( 'NONE', *, *, #9705, .T. ) ;
#18762 = VECTOR ( 'NONE', #8799, 1000.000000000000000 ) ;
#18763 = EDGE_CURVE ( 'NONE', #19846, #3448, #18748, .T. ) ;
#18764 = CARTESIAN_POINT ( 'NONE',  ( -1.979299272550000266, -58.31202229489999667, -23.87650549820000023 ) ) ;
#18765 = DIRECTION ( 'NONE',  ( 0.000000000000000000, 1.000000000000000000, 0.000000000000000000 ) ) ;
#18766 = CARTESIAN_POINT ( 'NONE',  ( -0.7622684235660001084, -96.16784751140001219, 23.03987708760000075 ) ) ;
#18767 = CARTESIAN_POINT ( 'NONE',  ( -0.7193305230537280215, -101.4628082233789002, -15.95725401771322005 ) ) ;
#18768 = ORIENTED_EDGE ( 'NONE', *, *, #18003, .T. ) ;
#18769 = CARTESIAN_POINT ( 'NONE',  ( -3.841884380821040335, -98.73470582036235044, 18.09326313051193225 ) ) ;
#18770 = AXIS2_PLACEMENT_3D ( 'NONE', #22625, #18400, #795 ) ;
#18771 = DIRECTION ( 'NONE',  ( 1.000000000000000000, 0.000000000000000000, 0.000000000000000000 ) ) ;
#18772 = CARTESIAN_POINT ( 'NONE',  ( -22.40618160359999678, -92.50425969839999141, -19.26308860609999840 ) ) ;
#18773 = DIRECTION ( 'NONE',  ( 1.000000000000000000, 0.000000000000000000, 0.000000000000000000 ) ) ;
#18774 = VERTEX_POINT ( 'NONE', #27340 ) ;
#18775 = CARTESIAN_POINT ( 'NONE',  ( -10.54736184929999965, -12.25000000000000000, -19.30681636159999925 ) ) ;
#18776 = CARTESIAN_POINT ( 'NONE',  ( 0.000000000000000000, -15.80000000000000071, 0.000000000000000000 ) ) ;
#18777 = ORIENTED_EDGE ( 'NONE', *, *, #8829, .F. ) ;
#18778 = CARTESIAN_POINT ( 'NONE',  ( -14.53416873709999990, -79.85300529469999731, 36.65982618790000203 ) ) ;
#18779 = DIRECTION ( 'NONE',  ( 0.000000000000000000, 1.000000000000000000, 0.000000000000000000 ) ) ;
#18780 = B_SPLINE_CURVE_WITH_KNOTS ( 'NONE', 3,
 ( #18165, #15521, #22689, #277, #8818, #9119, #26918, #24431, #11138, #27063, #4469, #18321, #11588, #22242, #4908, #7107, #122, #15970, #6958, #8973, #15820, #26778, #24732, #4614, #13489, #4767, #13788, #12313, #9700, #23407, #714, #18465, #7555, #27918 ),
 .UNSPECIFIED., .F., .F.,
 ( 4, 2, 2, 2, 1, 1, 2, 2, 2, 2, 1, 1, 2, 2, 2, 2, 2, 2, 4 ),
 ( 0.000000000000000000, 0.1249999999998953615, 0.1874999999998430145, 0.2187499999998188394, 0.2343749999998089584, 0.2421874999998039901, 0.2460937499998017697, 0.2499999999997995492, 0.3749999999998058220, 0.4374999999998089306, 0.4687499999998105404, 0.4843749999998114841, 0.4921874999998120392, 0.4999999999998125944, 0.6249999999998588907, 0.6874999999998817612, 0.7187499999998936406, 0.7499999999999054090, 1.000000000000000000 ),
 .UNSPECIFIED. ) ;
#18781 = CARTESIAN_POINT ( 'NONE',  ( -4.234949299229999298, -72.18744871750000414, -28.56489076020000439 ) ) ;
#18782 = AXIS2_PLACEMENT_3D ( 'NONE', #1228, #5577, #21038 ) ;
#18783 = DIRECTION ( 'NONE',  ( 0.000000000000000000, 1.000000000000000000, 0.000000000000000000 ) ) ;
#18784 = ORIENTED_EDGE ( 'NONE', *, *, #5287, .T. ) ;
#18785 = CARTESIAN_POINT ( 'NONE',  ( 36.28164463560000286, -74.50000004449999835, -14.97346875809999922 ) ) ;
#18786 = CARTESIAN_POINT ( 'NONE',  ( -15.92767415050000146, -101.0452850540000043, 3.185060022200000063 ) ) ;
#18787 = CARTESIAN_POINT ( 'NONE',  ( 25.16410386810000333, -61.75794029819999764, 1.280048851440000135 ) ) ;
#18788 = CARTESIAN_POINT ( 'NONE',  ( -20.33184189050000157, -61.83390236249999816, 14.43150019080000135 ) ) ;
#18789 = ORIENTED_EDGE ( 'NONE', *, *, #7502, .T. ) ;
#18790 = DIRECTION ( 'NONE',  ( 1.000000000000000000, 0.000000000000000000, 0.000000000000000000 ) ) ;
#18791 = CARTESIAN_POINT ( 'NONE',  ( -2.647422304290000472, -19.49009541680000268, -23.73806674440000108 ) ) ;
#18792 = CARTESIAN_POINT ( 'NONE',  ( 23.06813085299999955, -94.22763312370000222, -7.559806761219999949 ) ) ;
#18793 = ORIENTED_EDGE ( 'NONE', *, *, #15543, .F. ) ;
#18794 = AXIS2_PLACEMENT_3D ( 'NONE', #26803, #18048, #26945 ) ;
#18795 = LINE ( 'NONE', #7987, #1901 ) ;
#18796 = CARTESIAN_POINT ( 'NONE',  ( -31.99666054769999946, -74.00000000000000000, -22.02415758960000147 ) ) ;
#18797 = CARTESIAN_POINT ( 'NONE',  ( 15.85540327669583327, -101.1553309671668330, 4.123844213901046274 ) ) ;
#18798 = DIRECTION ( 'NONE',  ( 0.000000000000000000, -1.000000000000000000, 0.000000000000000000 ) ) ;
#18799 = EDGE_LOOP ( 'NONE', ( #11476, #172, #3001, #422 ) ) ;
#18800 = UNCERTAINTY_MEASURE_WITH_UNIT (LENGTH_MEASURE( 1.000000000000000082E-05 ), #5697, 'distance_accuracy_value', 'NONE');
#18801 = ADVANCED_FACE ( 'NONE', ( #27644 ), #846, .T. ) ;
#18802 = VECTOR ( 'NONE', #15286, 1000.000000000000114 ) ;
#18803 = CARTESIAN_POINT ( 'NONE',  ( 3.724765212310714446, -94.01599395605515497, 25.79154880062783306 ) ) ;
#18804 = EDGE_CURVE ( 'NONE', #3592, #5336, #4333, .T. ) ;
#18805 = ORIENTED_EDGE ( 'NONE', *, *, #3041, .T. ) ;
#18806 = CARTESIAN_POINT ( 'NONE',  ( 46.18304991175620700, -73.53220734123081570, -3.800088742014810173 ) ) ;
#18807 = EDGE_LOOP ( 'NONE', ( #4325, #3555, #20977, #3435 ) ) ;
#18808 = CARTESIAN_POINT ( 'NONE',  ( -13.33147262089999963, -42.22514961549999413, 20.36865418349999857 ) ) ;
#18809 = CARTESIAN_POINT ( 'NONE',  ( -5.884304964390000059, -101.1461874320000049, 15.04985543319999941 ) ) ;
#18810 = EDGE_CURVE ( 'NONE', #11457, #10298, #18327, .T. ) ;
#18811 = VERTEX_POINT ( 'NONE', #16550 ) ;
#18812 = CARTESIAN_POINT ( 'NONE',  ( -18.11577714932429828, -92.50000100535636705, -23.66412518367106088 ) ) ;
#18813 = EDGE_CURVE ( 'NONE', #13063, #16727, #23943, .T. ) ;
#18814 = VECTOR ( 'NONE', #1617, 1000.000000000000000 ) ;
#18815 = CONICAL_SURFACE ( 'NONE', #6219, 55.67692378859999280, 1.047197551199999799 ) ;
#18816 = CARTESIAN_POINT ( 'NONE',  ( 40.37851622870000057, -74.24288085019999528, 7.248115061030000028 ) ) ;
#18817 = DIRECTION ( 'NONE',  ( 1.000000000000000000, 0.000000000000000000, 0.000000000000000000 ) ) ;
#18818 = CARTESIAN_POINT ( 'NONE',  ( -11.70907145606914135, -62.05375851120123087, -23.11666430726260657 ) ) ;
#18819 = CARTESIAN_POINT ( 'NONE',  ( -40.00000000000000000, -84.00000000000000000, 0.000000000000000000 ) ) ;
#18820 = ORIENTED_EDGE ( 'NONE', *, *, #5933, .F. ) ;
#18821 = FACE_OUTER_BOUND ( 'NONE', #28059, .T. ) ;
#18822 = CARTESIAN_POINT ( 'NONE',  ( 8.113043078722281365, -34.60505764027403330, -21.05852217749055555 ) ) ;
#18823 = DIRECTION ( 'NONE',  ( 0.000000000000000000, 1.000000000000000000, 0.000000000000000000 ) ) ;
#18824 = CARTESIAN_POINT ( 'NONE',  ( 14.81927149150000034, -101.2530993010000060, 3.356308434120000239 ) ) ;
#18825 = ORIENTED_EDGE ( 'NONE', *, *, #7185, .F. ) ;
#18826 = AXIS2_PLACEMENT_3D ( 'NONE', #3786, #11017, #17767 ) ;
#18827 = DIRECTION ( 'NONE',  ( 0.000000000000000000, 1.000000000000000000, 0.000000000000000000 ) ) ;
#18828 = CARTESIAN_POINT ( 'NONE',  ( 11.40881661680000114, -94.59276292389999696, 20.88369873619999950 ) ) ;
#18829 = ORIENTED_EDGE ( 'NONE', *, *, #13232, .F. ) ;
#18830 = DIRECTION ( 'NONE',  ( 1.000000000000000000, 0.000000000000000000, 0.000000000000000000 ) ) ;
#18831 = DIRECTION ( 'NONE',  ( 0.000000000000000000, 1.000000000000000000, 0.000000000000000000 ) ) ;
#18832 = CARTESIAN_POINT ( 'NONE',  ( 7.426814492070000107, -35.28814190290000141, -21.34788074219999743 ) ) ;
#18833 = CARTESIAN_POINT ( 'NONE',  ( 27.75394116159999669, -74.50000000000000000, -27.75394116159999669 ) ) ;
#18834 = CARTESIAN_POINT ( 'NONE',  ( 0.000000000000000000, -14.30000000000000071, 0.000000000000000000 ) ) ;
#18835 = AXIS2_PLACEMENT_3D ( 'NONE', #19744, #17721, #15354 ) ;
#18836 = EDGE_CURVE ( 'NONE', #20440, #24292, #15976, .T. ) ;
#18837 = VERTEX_POINT ( 'NONE', #20333 ) ;
#18838 = CARTESIAN_POINT ( 'NONE',  ( 5.326862811529999898E-15, -73.00000000000000000, -47.25000000000000000 ) ) ;
#18839 = CARTESIAN_POINT ( 'NONE',  ( -13.17060483900000101, -68.28989248250000799, -23.12790341000000183 ) ) ;
#18840 = EDGE_CURVE ( 'NONE', #12917, #22615, #2871, .T. ) ;
#18841 = ORIENTED_EDGE ( 'NONE', *, *, #8798, .F. ) ;
#18842 = CARTESIAN_POINT ( 'NONE',  ( 47.13608539959999888, -74.52720457959999578, -1.647993573179999949 ) ) ;
#18843 = LINE ( 'NONE', #23350, #9418 ) ;
#18844 = EDGE_CURVE ( 'NONE', #3331, #21528, #9256, .T. ) ;
#18845 = DIRECTION ( 'NONE',  ( 0.4794255386042040046, 0.000000000000000000, 0.8775825618903722036 ) ) ;
#18846 = CARTESIAN_POINT ( 'NONE',  ( -7.878839520130000551, -100.4650220110000021, 14.87768963799999966 ) ) ;
#18847 = AXIS2_PLACEMENT_3D ( 'NONE', #17885, #26627, #28792 ) ;
#18848 = CARTESIAN_POINT ( 'NONE',  ( -18.77458274581442765, -19.20927481204605769, 11.51544471821851445 ) ) ;
#18849 = CARTESIAN_POINT ( 'NONE',  ( 7.156454249440000304, -36.57019169040000151, -21.47211211410000331 ) ) ;
#18850 = CARTESIAN_POINT ( 'NONE',  ( 40.00000000000000000, -79.00000000000000000, 4.898587196589999938E-15 ) ) ;
#18851 = ORIENTED_EDGE ( 'NONE', *, *, #25423, .F. ) ;
#18852 = CARTESIAN_POINT ( 'NONE',  ( -39.74699101870318430, -73.82038814073398214, 7.246150394361534630 ) ) ;
#18853 = CARTESIAN_POINT ( 'NONE',  ( -22.23129158500000102, -94.79581646409999962, -8.137667245660001214 ) ) ;
#18854 = CARTESIAN_POINT ( 'NONE',  ( 26.30230850349999727, -72.70510570390000282, 11.30503913470000121 ) ) ;
#18855 = CARTESIAN_POINT ( 'NONE',  ( 22.97877291159999658, -37.99999999279999230, -9.393614097370001303 ) ) ;
#18856 = ORIENTED_EDGE ( 'NONE', *, *, #4711, .F. ) ;
#18857 = TOROIDAL_SURFACE ( 'NONE', #3934, 6.750000000000000000, 2.000000000000000000 ) ;
#18858 = CARTESIAN_POINT ( 'NONE',  ( 20.50116792230000229, -18.85523517670000260, -7.685455265189999885 ) ) ;
#18859 = FACE_OUTER_BOUND ( 'NONE', #21419, .T. ) ;
#18860 = CARTESIAN_POINT ( 'NONE',  ( -2.572575538410000195, -45.92926717529999792, -24.95080834190000019 ) ) ;
#18861 = DIRECTION ( 'NONE',  ( 0.000000000000000000, 1.000000000000000000, 0.000000000000000000 ) ) ;
#18862 = DIRECTION ( 'NONE',  ( 0.000000000000000000, 1.000000000000000000, 0.000000000000000000 ) ) ;
#18863 = CARTESIAN_POINT ( 'NONE',  ( 11.94375585680425367, -101.6174239712916574, -10.68122429318817268 ) ) ;
#18864 = CARTESIAN_POINT ( 'NONE',  ( 7.202169761539999548, -101.2530994060000040, 13.37848089600000101 ) ) ;
#18865 = CARTESIAN_POINT ( 'NONE',  ( 16.01855245282755646, -96.92941831232313632, 15.11027898058047647 ) ) ;
#18866 = DIRECTION ( 'NONE',  ( 0.000000000000000000, 1.000000000000000000, 0.000000000000000000 ) ) ;
#18867 = ORIENTED_EDGE ( 'NONE', *, *, #2050, .T. ) ;
#18868 = CARTESIAN_POINT ( 'NONE',  ( -32.75442352089999787, -74.37394555080000202, -21.60834384349999837 ) ) ;
#18869 = CARTESIAN_POINT ( 'NONE',  ( -2.876553231629999985, -108.5000000000000000, -5.265495371340000119 ) ) ;
#18870 = VECTOR ( 'NONE', #23454, 1000.000000000000000 ) ;
#18871 = EDGE_CURVE ( 'NONE', #28370, #25772, #1567, .T. ) ;
#18872 = CARTESIAN_POINT ( 'NONE',  ( 7.695130988680000783, -101.4135462429999990, 14.00070023930000040 ) ) ;
#18873 = EDGE_CURVE ( 'NONE', #26586, #18106, #27430, .T. ) ;
#18874 = CARTESIAN_POINT ( 'NONE',  ( -11.49982146049999976, -94.92598208000001136, -21.36427486740000248 ) ) ;
#18875 = CARTESIAN_POINT ( 'NONE',  ( 19.92119995959999912, -34.82099949419999518, -8.965452275210001432 ) ) ;
#18876 = CARTESIAN_POINT ( 'NONE',  ( 7.249276399906878332, -74.06318173168557450, 40.12703402721685109 ) ) ;
#18877 = CARTESIAN_POINT ( 'NONE',  ( 26.54817965250783018, -93.04141874247987687, -10.31287963464188451 ) ) ;
#18878 = CARTESIAN_POINT ( 'NONE',  ( -20.59500362320578049, -93.08384138314025336, -20.57120710345400383 ) ) ;
#18879 = EDGE_CURVE ( 'NONE', #10296, #20072, #14585, .T. ) ;
#18880 = EDGE_LOOP ( 'NONE', ( #599, #19315, #26497, #21605 ) ) ;
#18881 = CARTESIAN_POINT ( 'NONE',  ( -1.283023294879999998, -111.0000000000000000, -16.20107482390000087 ) ) ;
#18882 = CARTESIAN_POINT ( 'NONE',  ( 31.00000000000000000, -15.00000000000000000, -4.500000000000000000 ) ) ;
#18883 = VERTEX_POINT ( 'NONE', #6023 ) ;
#18884 = CARTESIAN_POINT ( 'NONE',  ( 25.86648696739999664, -67.35799165719998882, -10.65566759900000093 ) ) ;
#18885 = ORIENTED_EDGE ( 'NONE', *, *, #12503, .T. ) ;
#18886 = CARTESIAN_POINT ( 'NONE',  ( 0.5233167930302693449, -100.1585711159247722, -17.16730309748452399 ) ) ;
#18887 = CARTESIAN_POINT ( 'NONE',  ( -11.29440317008408101, -19.46531115638632059, 19.08176919539176097 ) ) ;
#18888 = CARTESIAN_POINT ( 'NONE',  ( -29.16815472389999897, -80.00000000000000000, -29.16815472389999897 ) ) ;
#18889 = AXIS2_PLACEMENT_3D ( 'NONE', #2200, #11356, #18078 ) ;
#18890 = CARTESIAN_POINT ( 'NONE',  ( 13.16431709405246764, -92.87422005961725802, 27.51274203059175605 ) ) ;
#18891 = CARTESIAN_POINT ( 'NONE',  ( -13.24982249700000025, -93.87552273890000265, -20.99014450399999987 ) ) ;
#18892 = CARTESIAN_POINT ( 'NONE',  ( 21.99462582090000140, -74.00072165509999422, -32.20449087679999423 ) ) ;
#18893 = CARTESIAN_POINT ( 'NONE',  ( -22.94161197439999711, -72.70510790119999456, 17.12593288190000251 ) ) ;
#18894 = CARTESIAN_POINT ( 'NONE',  ( -18.48852190589999722, -96.16769445330000110, 13.76947523039999943 ) ) ;
#18895 = CARTESIAN_POINT ( 'NONE',  ( -36.05087847149999902, -63.50000000000000000, 2.157414923720000210 ) ) ;
#18896 = CARTESIAN_POINT ( 'NONE',  ( 0.000000000000000000, -108.5000000000000000, 0.000000000000000000 ) ) ;
#18897 = CARTESIAN_POINT ( 'NONE',  ( 40.00000000000000000, -69.50000000000000000, 2.433892081919999696E-15 ) ) ;
#18898 = DIRECTION ( 'NONE',  ( 0.000000000000000000, 1.000000000000000000, 0.000000000000000000 ) ) ;
#18899 = ORIENTED_EDGE ( 'NONE', *, *, #12805, .F. ) ;
#18900 = CARTESIAN_POINT ( 'NONE',  ( 9.476129726560001743, -36.00000000000000000, -20.06309461059999677 ) ) ;
#18901 = ORIENTED_EDGE ( 'NONE', *, *, #20433, .F. ) ;
#18902 = EDGE_CURVE ( 'NONE', #19419, #640, #19161, .T. ) ;
#18903 = FACE_OUTER_BOUND ( 'NONE', #12113, .T. ) ;
#18904 = EDGE_CURVE ( 'NONE', #15453, #258, #25996, .T. ) ;
#18905 = FACE_OUTER_BOUND ( 'NONE', #19543, .T. ) ;
#18906 = EDGE_CURVE ( 'NONE', #11916, #3127, #10385, .T. ) ;
#18907 = CARTESIAN_POINT ( 'NONE',  ( -0.6915678686394176600, -101.1604341566293925, -15.34138172876354389 ) ) ;
#18908 = CARTESIAN_POINT ( 'NONE',  ( -11.23277242420000022, -95.05245081340000013, -21.31917440760000204 ) ) ;
#18909 = ORIENTED_EDGE ( 'NONE', *, *, #5573, .T. ) ;
#18910 = CARTESIAN_POINT ( 'NONE',  ( -37.75000000000000000, -65.63577453799999262, 0.7216878364859999895 ) ) ;
#18911 = VERTEX_POINT ( 'NONE', #28047 ) ;
#18912 = CIRCLE ( 'NONE', #16086, 20.64285714289999873 ) ;
#18913 = DIRECTION ( 'NONE',  ( 0.4794255386042000078, 0.000000000000000000, 0.8775825618903743131 ) ) ;
#18914 = CARTESIAN_POINT ( 'NONE',  ( 8.904194151329999585, -35.90042246200000164, -20.44172831670000079 ) ) ;
#18915 = CARTESIAN_POINT ( 'NONE',  ( 26.33711340400000367, -92.75885938639999040, -7.868255112059999945 ) ) ;
#18916 = APPLICATION_CONTEXT ( 'automotive_design' ) ;
#18917 = CARTESIAN_POINT ( 'NONE',  ( -15.08135663260000037, -67.66819252530000028, 22.63088120529999969 ) ) ;
#18918 = ORIENTED_EDGE ( 'NONE', *, *, #28313, .T. ) ;
#18919 = CARTESIAN_POINT ( 'NONE',  ( -14.80203930059999884, -101.0554840979999938, 4.588568860439999675 ) ) ;
#18920 = CARTESIAN_POINT ( 'NONE',  ( -16.12855232609999945, -100.3665383609999964, 2.616550526240000174 ) ) ;
#18921 = CARTESIAN_POINT ( 'NONE',  ( 25.30470987589999865, -63.24100619570000248, 1.147374915679999940 ) ) ;
#18922 = CARTESIAN_POINT ( 'NONE',  ( 19.45083578249999690, -34.98500792359999423, -8.988292418119998572 ) ) ;
#18923 = B_SPLINE_SURFACE_WITH_KNOTS ( 'NONE', 5, 5, ( 
 ( #8941, #26593, #26890, #26449, #387, #2264, #20317, #15496, #15344 ),
 ( #2566, #24260, #7080, #22663, #8792, #2707, #24405, #11561, #20025 ),
 ( #17994, #6929, #4299, #17707, #17851, #20177, #22523, #6481, #9234 ),
 ( #4442, #26749, #15939, #11415, #17556, #15792, #24846, #20470, #19872 ),
 ( #11107, #24702, #11268, #22081, #13171, #2127, #24548, #248, #13613 ),
 ( #13314, #8652, #10962, #6782, #4736, #93, #6634, #28752, #22218 ) ),
 .UNSPECIFIED., .F., .F., .F.,
 ( 6, 6 ),
 ( 6, 3, 6 ),
 ( 20.62672786149999737, 31.13134626069999911 ),
 ( 0.000000000000000000, 1.000000000000000000, 2.000000000000000000 ),
 .UNSPECIFIED. ) ;
#18924 = EDGE_CURVE ( 'NONE', #17438, #11909, #28127, .T. ) ;
#18925 = VERTEX_POINT ( 'NONE', #10104 ) ;
#18926 = CARTESIAN_POINT ( 'NONE',  ( 9.334872109610000362E-16, -74.00000000000000000, -2.419703924680000090E-15 ) ) ;
#18927 = CARTESIAN_POINT ( 'NONE',  ( -7.249922261819999214, -74.00000000000000000, 40.03357376379999977 ) ) ;
#18928 = CARTESIAN_POINT ( 'NONE',  ( 23.85918062689999886, -92.51331408429999215, -17.09634816450000017 ) ) ;
#18929 = ORIENTED_EDGE ( 'NONE', *, *, #4882, .F. ) ;
#18930 = CARTESIAN_POINT ( 'NONE',  ( -41.75000000000000000, -65.14977478849999670, -2.684678751739999925 ) ) ;
#18931 = CARTESIAN_POINT ( 'NONE',  ( 7.426814476920000629, -35.28814186609999837, -21.34788074160000093 ) ) ;
#18932 = CARTESIAN_POINT ( 'NONE',  ( 37.00594063530000000, -79.99129919269999789, -13.97169134750000019 ) ) ;
#18933 = ORIENTED_EDGE ( 'NONE', *, *, #8902, .T. ) ;
#18934 = EDGE_CURVE ( 'NONE', #24982, #23662, #5291, .T. ) ;
#18935 = CARTESIAN_POINT ( 'NONE',  ( 37.01148927991571469, -79.86867281223175041, -14.24953229101417840 ) ) ;
#18936 = LINE ( 'NONE', #23578, #20872 ) ;
#18937 = ORIENTED_EDGE ( 'NONE', *, *, #26640, .T. ) ;
#18938 = CARTESIAN_POINT ( 'NONE',  ( -18.22105428487606460, -98.38508418248619591, 5.014634119382404442 ) ) ;
#18939 = EDGE_CURVE ( 'NONE', #17051, #21547, #4356, .T. ) ;
#18940 = ORIENTED_EDGE ( 'NONE', *, *, #19423, .T. ) ;
#18941 = DIRECTION ( 'NONE',  ( 0.000000000000000000, 1.000000000000000000, 0.000000000000000000 ) ) ;
#18942 = CARTESIAN_POINT ( 'NONE',  ( -5.973279726580000393, -101.5317765570000006, 14.93807730569999848 ) ) ;
#18943 = ORIENTED_EDGE ( 'NONE', *, *, #13069, .F. ) ;
#18944 = CARTESIAN_POINT ( 'NONE',  ( 13.31770606849999972, -100.4792519539999915, -9.213118301410000655 ) ) ;
#18945 = VERTEX_POINT ( 'NONE', #19433 ) ;
#18946 = CARTESIAN_POINT ( 'NONE',  ( 38.62788781560000473, -74.00000025069999765, 7.627567457969999687 ) ) ;
#18947 = CARTESIAN_POINT ( 'NONE',  ( -13.15875165482993303, -101.5703832412493455, -9.204769674458903594 ) ) ;
#18948 = DIRECTION ( 'NONE',  ( 0.000000000000000000, 1.000000000000000000, 0.000000000000000000 ) ) ;
#18949 = CARTESIAN_POINT ( 'NONE',  ( 46.74944134502681692, -79.86660166543690309, -3.328368085118203368 ) ) ;
#18950 = EDGE_LOOP ( 'NONE', ( #9915, #22366, #13686, #5030, #19380, #8846, #19843 ) ) ;
#18951 = CARTESIAN_POINT ( 'NONE',  ( -32.38674382290000153, -80.50000054920000991, -22.17565024390000161 ) ) ;
#18952 = CARTESIAN_POINT ( 'NONE',  ( -37.75000000000000000, -65.63577453799999262, -0.7216878364849999006 ) ) ;
#18953 = EDGE_CURVE ( 'NONE', #19757, #22747, #21120, .T. ) ;
#18954 = CARTESIAN_POINT ( 'NONE',  ( 14.82033914870000046, -101.2010924020000004, 3.644636806539999885 ) ) ;
#18955 = ORIENTED_EDGE ( 'NONE', *, *, #8574, .F. ) ;
#18956 = CARTESIAN_POINT ( 'NONE',  ( -2.303924720019999928, -79.89639594039999793, 47.10762694129999772 ) ) ;
#18957 = CARTESIAN_POINT ( 'NONE',  ( 4.314829847440000421, -17.50000000000000000, 7.898243057010000179 ) ) ;
#18958 = ORIENTED_EDGE ( 'NONE', *, *, #9703, .T. ) ;
#18959 = DIRECTION ( 'NONE',  ( 0.000000000000000000, -1.000000000000000000, 0.000000000000000000 ) ) ;
#18960 = DIRECTION ( 'NONE',  ( 0.000000000000000000, -1.000000000000000000, 0.000000000000000000 ) ) ;
#18961 = CARTESIAN_POINT ( 'NONE',  ( 6.054273664322402659, -92.50000267096280027, 29.18077564220382314 ) ) ;
#18962 = CARTESIAN_POINT ( 'NONE',  ( 29.87432578229999791, -73.33171065870000405, -25.19102557209999915 ) ) ;
#18963 = EDGE_CURVE ( 'NONE', #24336, #22763, #1359, .T. ) ;
#18964 = CARTESIAN_POINT ( 'NONE',  ( -15.78701020529999965, -72.82938648530000592, 23.94860758700000147 ) ) ;
#18965 = AXIS2_PLACEMENT_3D ( 'NONE', #4489, #15994, #6831 ) ;
#18966 = TOROIDAL_SURFACE ( 'NONE', #17554, 38.75000000000000000, 0.5000000000000000000 ) ;
#18967 = DIRECTION ( 'NONE',  ( -0.8775825618903722036, 0.000000000000000000, 0.4794255386042041156 ) ) ;
#18968 = CIRCLE ( 'NONE', #19411, 7.250000000000000000 ) ;
#18969 = ORIENTED_EDGE ( 'NONE', *, *, #21053, .F. ) ;
#18970 = CARTESIAN_POINT ( 'NONE',  ( -40.26982517637422632, -74.16605908757436794, -7.244980372376159217 ) ) ;
#18971 = AXIS2_PLACEMENT_3D ( 'NONE', #21189, #17222, #14743 ) ;
#18972 = CARTESIAN_POINT ( 'NONE',  ( 20.80917882690000198, -36.16278974830000692, -9.004964305669998836 ) ) ;
#18973 = ORIENTED_EDGE ( 'NONE', *, *, #10586, .T. ) ;
#18974 = CARTESIAN_POINT ( 'NONE',  ( -13.19529713839999907, -101.1659666750000071, -9.073059359340000185 ) ) ;
#18975 = B_SPLINE_SURFACE_WITH_KNOTS ( 'NONE', 5, 5, ( 
 ( #28739, #13006, #24094, #8775, #15328, #19721, #4132, #25619, #21917 ),
 ( #1968, #16723, #5648, #14526, #10811, #24245, #8638, #19055, #15478 ),
 ( #6461, #4282, #21242, #13155, #10947, #26576, #23433, #17688, #16867 ),
 ( #1292, #1166, #18919, #3469, #10136, #25756, #12334, #7977, #14669 ),
 ( #23563, #11091, #7205, #374, #15776, #27167, #6770, #9217, #18124 ),
 ( #11401, #13447, #20455, #16072, #11253, #27312, #24974, #15631, #24529 ) ),
 .UNSPECIFIED., .F., .F., .F.,
 ( 6, 6 ),
 ( 6, 3, 6 ),
 ( 5.000411456039999258, 6.439463439139999856 ),
 ( 0.000000000000000000, 0.2500000000000000000, 0.5000000000000000000 ),
 .UNSPECIFIED. ) ;
#18976 = CARTESIAN_POINT ( 'NONE',  ( 46.85827871259999711, -80.18254846009999426, -2.615703315070000201 ) ) ;
#18977 = EDGE_LOOP ( 'NONE', ( #7614, #18937, #1302, #10411, #11445 ) ) ;
#18978 = CARTESIAN_POINT ( 'NONE',  ( 14.28941763439999946, -92.50000000000000000, -3.575252188409999921 ) ) ;
#18979 = DIRECTION ( 'NONE',  ( -1.000000000000000000, 0.000000000000000000, -1.095614826932720052E-15 ) ) ;
#18980 = CARTESIAN_POINT ( 'NONE',  ( 0.000000000000000000, -57.47855601759999900, 0.000000000000000000 ) ) ;
#18981 = ORIENTED_EDGE ( 'NONE', *, *, #1308, .T. ) ;
#18982 = VECTOR ( 'NONE', #25881, 1000.000000000000000 ) ;
#18983 = CARTESIAN_POINT ( 'NONE',  ( -11.91266501540000000, -74.50000000000000000, 46.64429291560000479 ) ) ;
#18984 = CARTESIAN_POINT ( 'NONE',  ( 10.54736184929999965, -12.25000000000000000, 19.30681636159999925 ) ) ;
#18985 = CARTESIAN_POINT ( 'NONE',  ( 26.22877567449999958, -72.82938648530000592, 11.61106382910000079 ) ) ;
#18986 = DIRECTION ( 'NONE',  ( 1.000000000000000000, 0.000000000000000000, 0.000000000000000000 ) ) ;
#18987 = VERTEX_POINT ( 'NONE', #8774 ) ;
#18988 = CARTESIAN_POINT ( 'NONE',  ( -27.18988201479999844, -23.90155444570000043, -49.77074518290000071 ) ) ;
#18989 = EDGE_CURVE ( 'NONE', #6736, #731, #2995, .T. ) ;
#18990 = CARTESIAN_POINT ( 'NONE',  ( -14.59012856380000045, -74.40829841730000282, 36.78913623730000637 ) ) ;
#18991 = CARTESIAN_POINT ( 'NONE',  ( -41.45000000000000284, -63.07912966450000880, -2.857883832489999776 ) ) ;
#18992 = CARTESIAN_POINT ( 'NONE',  ( 5.258016244619999627E-13, -84.00000000000000000, -5.364597654989999396E-13 ) ) ;
#18993 = EDGE_CURVE ( 'NONE', #19454, #15088, #25715, .T. ) ;
#18994 = CARTESIAN_POINT ( 'NONE',  ( -1.179554765616546597, -74.20448909913940838, 47.15348454221184227 ) ) ;
#18995 = AXIS2_PLACEMENT_3D ( 'NONE', #11021, #4362, #9 ) ;
#18996 = CARTESIAN_POINT ( 'NONE',  ( -0.02543935853460000188, -101.2530993010000060, -15.19457030269999898 ) ) ;
#18997 = DIRECTION ( 'NONE',  ( 0.4794255386042041156, 0.000000000000000000, 0.8775825618903722036 ) ) ;
#18998 = CARTESIAN_POINT ( 'NONE',  ( 15.52047986989999906, -100.9763228559999959, 2.247276725389999896 ) ) ;
#18999 = EDGE_CURVE ( 'NONE', #8881, #5109, #22512, .T. ) ;
#19000 = CARTESIAN_POINT ( 'NONE',  ( 19.98296175649999995, -94.98812477599999227, 14.17692170039999944 ) ) ;
#19001 = VERTEX_POINT ( 'NONE', #8925 ) ;
#19002 = EDGE_CURVE ( 'NONE', #4316, #18713, #28086, .T. ) ;
#19003 = CARTESIAN_POINT ( 'NONE',  ( 6.775498823059999509, -101.2927714249999980, 14.55524442019999931 ) ) ;
#19004 = CARTESIAN_POINT ( 'NONE',  ( -32.73892504640000567, -79.50000000000048317, -22.13232332860000184 ) ) ;
#19005 = AXIS2_PLACEMENT_3D ( 'NONE', #4646, #307, #13676 ) ;
#19006 = CARTESIAN_POINT ( 'NONE',  ( -11.36607352380000080, -94.98911577330000000, -21.34235610950000250 ) ) ;
#19007 = CARTESIAN_POINT ( 'NONE',  ( 7.936589523510000355, -35.30313553290000073, -21.23424061160000065 ) ) ;
#19008 = CARTESIAN_POINT ( 'NONE',  ( 36.60240428190000017, -80.39630767040000592, -14.17343997929999944 ) ) ;
#19009 = AXIS2_PLACEMENT_3D ( 'NONE', #11013, #21555, #24314 ) ;
#19010 = CARTESIAN_POINT ( 'NONE',  ( 25.00739163952697908, -93.86980009079698561, -5.047071168415053322 ) ) ;
#19011 = DIRECTION ( 'NONE',  ( 0.000000000000000000, 1.000000000000000000, 0.000000000000000000 ) ) ;
#19012 = DIRECTION ( 'NONE',  ( 1.000000000000000000, 0.000000000000000000, 0.000000000000000000 ) ) ;
#19013 = CARTESIAN_POINT ( 'NONE',  ( 19.43643821180000231, -34.66800313659999944, -8.988996541680000618 ) ) ;
#19014 = DIRECTION ( 'NONE',  ( 1.000000000000000000, 0.000000000000000000, 0.000000000000000000 ) ) ;
#19015 = ORIENTED_EDGE ( 'NONE', *, *, #19493, .F. ) ;
#19016 = FACE_OUTER_BOUND ( 'NONE', #24860, .T. ) ;
#19017 = DIRECTION ( 'NONE',  ( 0.000000000000000000, -1.000000000000000000, 0.000000000000000000 ) ) ;
#19018 = ORIENTED_EDGE ( 'NONE', *, *, #5188, .T. ) ;
#19019 = CARTESIAN_POINT ( 'NONE',  ( 26.88013615959999925, -70.45756328170000415, -11.38838332670000142 ) ) ;
#19020 = CARTESIAN_POINT ( 'NONE',  ( 0.4922916842733655596, -101.1553309671229357, -16.37551687936611344 ) ) ;
#19021 = CARTESIAN_POINT ( 'NONE',  ( 0.000000000000000000, -1.000000000000000000, 0.000000000000000000 ) ) ;
#19022 = CARTESIAN_POINT ( 'NONE',  ( 13.75150794455260161, -92.56772982772069724, 27.22406583199860108 ) ) ;
#19023 = CARTESIAN_POINT ( 'NONE',  ( -40.00000000000000000, -73.50000000000000000, 3.397282455350000038E-15 ) ) ;
#19024 = EDGE_CURVE ( 'NONE', #25924, #15673, #16922, .T. ) ;
#19025 = CARTESIAN_POINT ( 'NONE',  ( 21.86871528920000074, -73.56645110550000766, -31.55443393359999504 ) ) ;
#19026 = EDGE_CURVE ( 'NONE', #25651, #8949, #23581, .T. ) ;
#19027 = AXIS2_PLACEMENT_3D ( 'NONE', #28469, #15634, #22208 ) ;
#19028 = CARTESIAN_POINT ( 'NONE',  ( -22.65660754319999626, -72.37489965160000338, 17.66159453560000259 ) ) ;
#19029 = CIRCLE ( 'NONE', #24589, 0.5000000000000004441 ) ;
#19030 = CARTESIAN_POINT ( 'NONE',  ( -11.85905031950000144, -65.11419048950000388, -23.43762659500000112 ) ) ;
#19031 = CARTESIAN_POINT ( 'NONE',  ( -2.583988331150000040, -57.40875702419999982, -25.23271569440000306 ) ) ;
#19032 = CARTESIAN_POINT ( 'NONE',  ( 0.000000000000000000, -65.07443093669999712, 0.000000000000000000 ) ) ;
#19033 = ORIENTED_EDGE ( 'NONE', *, *, #26724, .T. ) ;
#19034 = EDGE_CURVE ( 'NONE', #26062, #8713, #11762, .T. ) ;
#19035 = CARTESIAN_POINT ( 'NONE',  ( 4.534235129290000123E-15, -84.50000000000000000, -36.25000000000000000 ) ) ;
#19036 = ORIENTED_EDGE ( 'NONE', *, *, #13690, .F. ) ;
#19037 = CARTESIAN_POINT ( 'NONE',  ( -12.61948338259999858, -101.6484611540000031, -9.836088610590000059 ) ) ;
#19038 = CIRCLE ( 'NONE', #13443, 20.64285714289999873 ) ;
#19039 = CARTESIAN_POINT ( 'NONE',  ( -28.04810641310000108, -92.68289710869998999, 1.703742907849999932 ) ) ;
#19040 = CARTESIAN_POINT ( 'NONE',  ( -19.65068252670000248, -52.63280639840000674, 12.32128691209999971 ) ) ;
#19041 = CIRCLE ( 'NONE', #13451, 4.750000000000000888 ) ;
#19042 = CIRCLE ( 'NONE', #23689, 0.5000000000000004441 ) ;
#19043 = FACE_OUTER_BOUND ( 'NONE', #13719, .T. ) ;
#19044 = AXIS2_PLACEMENT_3D ( 'NONE', #15466, #22056, #6308 ) ;
#19045 = ORIENTED_EDGE ( 'NONE', *, *, #7396, .F. ) ;
#19046 = DIRECTION ( 'NONE',  ( 0.4794255386042036715, 0.000000000000000000, 0.8775825618903724257 ) ) ;
#19047 = CARTESIAN_POINT ( 'NONE',  ( 40.50000000000000000, -12.50000000000000000, -4.500000000000000000 ) ) ;
#19048 = ORIENTED_EDGE ( 'NONE', *, *, #12704, .F. ) ;
#19049 = DIRECTION ( 'NONE',  ( 1.000000000000000000, 0.000000000000000000, 0.000000000000000000 ) ) ;
#19050 = CARTESIAN_POINT ( 'NONE',  ( 7.766330995219999700, -36.89698705200000006, -21.49508235269999901 ) ) ;
#19051 = ORIENTED_EDGE ( 'NONE', *, *, #22382, .T. ) ;
#19052 = CARTESIAN_POINT ( 'NONE',  ( -41.75000000000000000, -65.21397798589998729, 2.551096136580000007 ) ) ;
#19053 = CARTESIAN_POINT ( 'NONE',  ( -12.94585355959999973, -111.0000000000000000, -9.402386697720000797 ) ) ;
#19054 = ORIENTED_EDGE ( 'NONE', *, *, #26039, .F. ) ;
#19055 = CARTESIAN_POINT ( 'NONE',  ( -15.39251811099999934, -101.5369809019999963, 4.368436383219999719 ) ) ;
#19056 = EDGE_CURVE ( 'NONE', #26186, #14188, #26705, .T. ) ;
#19057 = CARTESIAN_POINT ( 'NONE',  ( -16.75827440639999821, -100.1995464040000030, 3.211019438220000133 ) ) ;
#19058 = CARTESIAN_POINT ( 'NONE',  ( -20.66721530050000055, -63.24178865179999320, 14.64673528719999851 ) ) ;
#19059 = VERTEX_POINT ( 'NONE', #7508 ) ;
#19060 = DIRECTION ( 'NONE',  ( 0.000000000000000000, -1.000000000000000000, 0.000000000000000000 ) ) ;
#19061 = CARTESIAN_POINT ( 'NONE',  ( 0.000000000000000000, -30.20000000000000284, 0.000000000000000000 ) ) ;
#19062 = EDGE_CURVE ( 'NONE', #25324, #8136, #5877, .T. ) ;
#19063 = CARTESIAN_POINT ( 'NONE',  ( -2.319540309899999819, -19.47458110719999880, -22.80676616219999886 ) ) ;
#19064 = CARTESIAN_POINT ( 'NONE',  ( -7.895689786979841251, -100.4166221067068960, 15.01891590590622627 ) ) ;
#19065 = EDGE_LOOP ( 'NONE', ( #6223, #24112, #3646, #16154 ) ) ;
#19066 = AXIS2_PLACEMENT_3D ( 'NONE', #16567, #8101, #5904 ) ;
#19067 = AXIS2_PLACEMENT_3D ( 'NONE', #27020, #2398, #7063 ) ;
#19068 = CARTESIAN_POINT ( 'NONE',  ( -41.45000000000000284, -65.14977478849999670, -2.857883832489999776 ) ) ;
#19069 = CARTESIAN_POINT ( 'NONE',  ( -41.78768228154088860, -65.71847493511117477, -1.315734964531388718 ) ) ;
#19070 = CARTESIAN_POINT ( 'NONE',  ( 36.36273659750000320, -79.72376025959999879, -14.77704751070000100 ) ) ;
#19071 = VERTEX_POINT ( 'NONE', #20302 ) ;
#19072 = CARTESIAN_POINT ( 'NONE',  ( 36.90024110328112528, -79.72731463880091951, -14.43636043974571415 ) ) ;
#19073 = CARTESIAN_POINT ( 'NONE',  ( 7.059056192828962573, -100.0559847774587183, 15.74847134990731767 ) ) ;
#19074 = CARTESIAN_POINT ( 'NONE',  ( -2.342296125043147992, -80.31169701321654486, 46.86165116740200887 ) ) ;
#19075 = VERTEX_POINT ( 'NONE', #16070 ) ;
#19076 = CARTESIAN_POINT ( 'NONE',  ( -19.81272040990000249, -52.63293862049999916, 12.05498172269999912 ) ) ;
#19077 = CARTESIAN_POINT ( 'NONE',  ( 45.84677419350000349, -73.50000000000000000, -4.286925650119999709 ) ) ;
#19078 = EDGE_LOOP ( 'NONE', ( #22742, #360, #3468, #8511 ) ) ;
#19079 = CARTESIAN_POINT ( 'NONE',  ( 22.86992907279999798, -57.41946977150000464, 10.24154027049999982 ) ) ;
#19080 = CARTESIAN_POINT ( 'NONE',  ( -5.854053644989999583, -101.0685849509999912, 14.98984533339999992 ) ) ;
#19081 = ORIENTED_EDGE ( 'NONE', *, *, #27753, .T. ) ;
#19082 = DIRECTION ( 'NONE',  ( -0.000000000000000000, 1.000000000000000000, 0.000000000000000000 ) ) ;
#19083 = DIRECTION ( 'NONE',  ( 0.000000000000000000, -1.000000000000000000, 0.000000000000000000 ) ) ;
#19084 = AXIS2_PLACEMENT_3D ( 'NONE', #21297, #23074, #3119 ) ;
#19085 = CARTESIAN_POINT ( 'NONE',  ( 39.85902549349999902, -74.23956954010000686, 7.332363420190000092 ) ) ;
#19086 = CARTESIAN_POINT ( 'NONE',  ( 8.605625357259999220, -37.33604032199999523, -21.85900819109999915 ) ) ;
#19087 = CARTESIAN_POINT ( 'NONE',  ( 19.74602846389999655, -32.73217875680000333, 10.78006621239999951 ) ) ;
#19088 = CARTESIAN_POINT ( 'NONE',  ( 7.564829567879999012E-15, -73.00000000000000000, 47.25000000000000000 ) ) ;
#19089 = EDGE_LOOP ( 'NONE', ( #14241, #2866, #27583, #13545 ) ) ;
#19090 = CARTESIAN_POINT ( 'NONE',  ( -32.20769381950000110, -80.50000045429999318, -22.43272063739999922 ) ) ;
#19091 = EDGE_CURVE ( 'NONE', #9130, #13313, #14125, .T. ) ;
#19092 = CARTESIAN_POINT ( 'NONE',  ( 1.375225265779999928, -94.98812079580000045, 24.46248543800000164 ) ) ;
#19093 = CARTESIAN_POINT ( 'NONE',  ( 24.08726961439999670, -93.01125874769999768, -11.28467891660000078 ) ) ;
#19094 = CARTESIAN_POINT ( 'NONE',  ( -1.454765721469999828, -53.83744478090000030, -23.38761430650000150 ) ) ;
#19095 = CARTESIAN_POINT ( 'NONE',  ( 29.75248106235870793, -92.74292563049040439, 6.711207100695092187 ) ) ;
#19096 = CARTESIAN_POINT ( 'NONE',  ( 30.97095665689999677, -72.00000182920000213, -20.30102787789999752 ) ) ;
#19097 = ORIENTED_EDGE ( 'NONE', *, *, #17906, .F. ) ;
#19098 = CARTESIAN_POINT ( 'NONE',  ( -7.278395029380000381, -74.00000000000000000, 36.96243111169999906 ) ) ;
#19099 = CARTESIAN_POINT ( 'NONE',  ( 7.105427357599999217E-15, -69.00000000000000000, 40.00000000000000000 ) ) ;
#19100 = CARTESIAN_POINT ( 'NONE',  ( 0.000000000000000000, -16.10310889129999623, 0.000000000000000000 ) ) ;
#19101 = CARTESIAN_POINT ( 'NONE',  ( 31.22904256650000221, -73.17619182029999081, -21.84902289639999751 ) ) ;
#19102 = CARTESIAN_POINT ( 'NONE',  ( -13.96509519684253497, -74.00000000000328271, 36.21398730655364062 ) ) ;
#19103 = AXIS2_PLACEMENT_3D ( 'NONE', #23117, #1136, #25587 ) ;
#19104 = DIRECTION ( 'NONE',  ( 0.000000000000000000, -1.000000000000000000, 0.000000000000000000 ) ) ;
#19105 = CIRCLE ( 'NONE', #3742, 12.25068835559999947 ) ;
#19106 = CIRCLE ( 'NONE', #6533, 55.67692378859999991 ) ;
#19107 = B_SPLINE_CURVE_WITH_KNOTS ( 'NONE', 5,
 ( #4165, #28495, #8533, #17437, #26325, #6350, #15214, #24129, #13041 ),
 .UNSPECIFIED., .F., .F.,
 ( 6, 3, 6 ),
 ( 0.000000000000000000, 0.5000000000000000000, 1.000000000000000000 ),
 .UNSPECIFIED. ) ;
#19108 = EDGE_LOOP ( 'NONE', ( #25263, #6673, #20093, #25617, #411 ) ) ;
#19109 = EDGE_CURVE ( 'NONE', #3210, #8623, #2035, .T. ) ;
#19110 = CARTESIAN_POINT ( 'NONE',  ( 21.41825492180000268, -36.11004389149999838, -7.844212321469999694 ) ) ;
#19111 = CARTESIAN_POINT ( 'NONE',  ( 21.26282345629999782, -36.17810633689999378, -8.125022609230001081 ) ) ;
#19112 = CARTESIAN_POINT ( 'NONE',  ( 5.988482279510000053E-15, -69.00000000000000000, 40.00000000000000000 ) ) ;
#19113 = VERTEX_POINT ( 'NONE', #24829 ) ;
#19114 = CARTESIAN_POINT ( 'NONE',  ( -12.45166847509999997, -101.1411470200000053, -9.043467198420000130 ) ) ;
#19115 = CARTESIAN_POINT ( 'NONE',  ( -18.06179280869999815, -92.68584241069999052, -23.36148935179999953 ) ) ;
#19116 = CARTESIAN_POINT ( 'NONE',  ( -1.449827971759999778, -100.8733978449999995, -15.65780246259999764 ) ) ;
#19117 = DIRECTION ( 'NONE',  ( 1.000000000000000000, 0.000000000000000000, 0.000000000000000000 ) ) ;
#19118 = ORIENTED_EDGE ( 'NONE', *, *, #13450, .T. ) ;
#19119 = AXIS2_PLACEMENT_3D ( 'NONE', #20136, #17958, #12251 ) ;
#19120 = CARTESIAN_POINT ( 'NONE',  ( 13.19211279289052641, -101.0610180772251709, -9.838472424427759933 ) ) ;
#19121 = AXIS2_PLACEMENT_3D ( 'NONE', #5441, #3401, #18711 ) ;
#19122 = CARTESIAN_POINT ( 'NONE',  ( -25.71127254079999958, -93.01584738799999741, -6.102658843190000404 ) ) ;
#19123 = CARTESIAN_POINT ( 'NONE',  ( 11.70579551850000044, -99.56347590750000620, -13.08273371679999997 ) ) ;
#19124 = VERTEX_POINT ( 'NONE', #11987 ) ;
#19125 = CARTESIAN_POINT ( 'NONE',  ( 19.62439614639999874, -18.62065274400000092, -8.477761181410000901 ) ) ;
#19126 = B_SPLINE_CURVE_WITH_KNOTS ( 'NONE', 3,
 ( #13373, #13523, #2478, #15855, #24908, #4939, #22434, #11333, #6991, #24765, #4800, #13677, #11621, #13969, #7430, #22582, #2626, #22873, #11474, #9445, #2915, #24462, #4498, #22276, #23440, #20975, #1040, #7584, #27540, #5517, #1173, #27683, #18927 ),
 .UNSPECIFIED., .F., .F.,
 ( 4, 2, 2, 1, 1, 1, 2, 2, 2, 2, 1, 2, 2, 2, 2, 1, 2, 2, 4 ),
 ( 0.000000000000000000, 0.1250000000002373379, 0.1875000000003559930, 0.2187500000004060918, 0.2343750000004311274, 0.2421875000004436451, 0.2460937500004491962, 0.2500000000004547474, 0.3750000000005158096, 0.4375000000005400125, 0.4687500000005451750, 0.4843750000005399015, 0.5000000000005345724, 0.6250000000004063416, 0.6875000000003421707, 0.7187500000003028688, 0.7343750000002831069, 0.7500000000002633449, 1.000000000000000000 ),
 .UNSPECIFIED. ) ;
#19127 = CARTESIAN_POINT ( 'NONE',  ( 11.38410404060000047, -101.1848541600000004, -10.19697977679999923 ) ) ;
#19128 = CARTESIAN_POINT ( 'NONE',  ( -11.35954001540000036, -74.00000000000000000, 45.25000000000000000 ) ) ;
#19129 = CARTESIAN_POINT ( 'NONE',  ( -18.11956189529999861, -94.23919442010000580, 17.23487956379999630 ) ) ;
#19130 = DIRECTION ( 'NONE',  ( 0.000000000000000000, 1.000000000000000000, 0.000000000000000000 ) ) ;
#19131 = VERTEX_POINT ( 'NONE', #20900 ) ;
#19132 = CARTESIAN_POINT ( 'NONE',  ( -1.301749480425372862, -74.17765396621948071, 47.13223634305940379 ) ) ;
#19133 = FACE_OUTER_BOUND ( 'NONE', #16170, .T. ) ;
#19134 = CARTESIAN_POINT ( 'NONE',  ( 9.454036308939999245, -61.76794852879999809, -23.45130291470000117 ) ) ;
#19135 = CARTESIAN_POINT ( 'NONE',  ( 15.81799604060000064, -101.3350617309999961, 2.549317426419999588 ) ) ;
#19136 = CARTESIAN_POINT ( 'NONE',  ( 21.66730995129999826, -58.31202229489999667, 10.22412929740000109 ) ) ;
#19137 = ORIENTED_EDGE ( 'NONE', *, *, #10616, .F. ) ;
#19138 = CARTESIAN_POINT ( 'NONE',  ( 6.188549911610000009, -100.4808658609999981, 14.99463308189999999 ) ) ;
#19139 = CARTESIAN_POINT ( 'NONE',  ( -13.09441083470000144, -92.84549618469999643, -23.96915825600000005 ) ) ;
#19140 = AXIS2_PLACEMENT_3D ( 'NONE', #28467, #19722, #17690 ) ;
#19141 = CIRCLE ( 'NONE', #1479, 21.14285714289999873 ) ;
#19142 = AXIS2_PLACEMENT_3D ( 'NONE', #21219, #1271, #10110 ) ;
#19143 = CARTESIAN_POINT ( 'NONE',  ( -11.69298240589999871, -94.57749834670001121, -21.18608921030000047 ) ) ;
#19144 = ADVANCED_FACE ( 'NONE', ( #17978 ), #373, .F. ) ;
#19145 = DIRECTION ( 'NONE',  ( 1.000000000000000000, 0.000000000000000000, 0.000000000000000000 ) ) ;
#19146 = CARTESIAN_POINT ( 'NONE',  ( 4.486712595243870005, -92.80045754838597816, -30.16820788345101434 ) ) ;
#19147 = CARTESIAN_POINT ( 'NONE',  ( -7.446447301520000117, -98.65110728930000050, 17.10060481960000089 ) ) ;
#19148 = FACE_OUTER_BOUND ( 'NONE', #7073, .T. ) ;
#19149 = CARTESIAN_POINT ( 'NONE',  ( 8.098514114769999495, -93.99830544889998407, -24.56325495060000108 ) ) ;
#19150 = ADVANCED_FACE ( 'NONE', ( #13893 ), #9473, .T. ) ;
#19151 = CARTESIAN_POINT ( 'NONE',  ( 19.33939820260000175, -31.63434013299999847, -8.993759961960000382 ) ) ;
#19152 = CARTESIAN_POINT ( 'NONE',  ( -6.580578580030000957, -111.0000000000000000, 15.40319725099999992 ) ) ;
#19153 = ORIENTED_EDGE ( 'NONE', *, *, #17899, .T. ) ;
#19154 = DIRECTION ( 'NONE',  ( -0.09756097560976760563, 0.000000000000000000, -0.9952295494196654602 ) ) ;
#19155 = CARTESIAN_POINT ( 'NONE',  ( -5.884304964390000059, -101.1461874320000049, 15.04985543319999941 ) ) ;
#19156 = ORIENTED_EDGE ( 'NONE', *, *, #15825, .T. ) ;
#19157 = ADVANCED_FACE ( 'NONE', ( #2549, #9214 ), #22948, .F. ) ;
#19158 = EDGE_CURVE ( 'NONE', #25354, #16270, #15568, .T. ) ;
#19159 = CARTESIAN_POINT ( 'NONE',  ( -0.8378492781409999646, -101.1292389529999980, -15.48430704140000103 ) ) ;
#19160 = DIRECTION ( 'NONE',  ( 1.000000000000000000, 0.000000000000000000, 0.000000000000000000 ) ) ;
#19161 = LINE ( 'NONE', #12433, #17379 ) ;
#19162 = AXIS2_PLACEMENT_3D ( 'NONE', #12471, #28084, #24432 ) ;
#19163 = CARTESIAN_POINT ( 'NONE',  ( 20.31705537619999902, -73.45782167609999647, -31.51289803219999541 ) ) ;
#19164 = AXIS2_PLACEMENT_3D ( 'NONE', #20390, #14131, #1277 ) ;
#19165 = CARTESIAN_POINT ( 'NONE',  ( -15.42268928922951865, -101.5369814700000148, 4.259183639765225848 ) ) ;
#19166 = CARTESIAN_POINT ( 'NONE',  ( -11.90443934750000032, -64.24504445130001784, -23.68393507400000075 ) ) ;
#19167 = CARTESIAN_POINT ( 'NONE',  ( 6.948750308559999311, -36.56992524569999858, -21.53806860960000336 ) ) ;
#19168 = CARTESIAN_POINT ( 'NONE',  ( -12.61948338259999858, -101.1889999979999999, -9.836088610590000059 ) ) ;
#19169 = VERTEX_POINT ( 'NONE', #12129 ) ;
#19170 = CARTESIAN_POINT ( 'NONE',  ( -11.18243144779999909, -57.47855601759999900, 20.51090144570000007 ) ) ;
#19171 = ORIENTED_EDGE ( 'NONE', *, *, #19339, .T. ) ;
#19172 = CARTESIAN_POINT ( 'NONE',  ( -14.62235247615832456, -101.2530994837961487, 4.129102802680486128 ) ) ;
#19173 = CIRCLE ( 'NONE', #10774, 28.68388914670000034 ) ;
#19174 = CARTESIAN_POINT ( 'NONE',  ( -2.719187978309999920, -64.35840732030000311, -26.13123539399999729 ) ) ;
#19175 = CARTESIAN_POINT ( 'NONE',  ( -29.57792341260000057, -92.63555401869999173, 6.374619421190000246 ) ) ;
#19176 = AXIS2_PLACEMENT_3D ( 'NONE', #8577, #24178, #8707 ) ;
#19177 = DIRECTION ( 'NONE',  ( 0.000000000000000000, 1.000000000000000000, 0.000000000000000000 ) ) ;
#19178 = EDGE_CURVE ( 'NONE', #11758, #17518, #21182, .T. ) ;
#19179 = B_SPLINE_CURVE_WITH_KNOTS ( 'NONE', 3,
 ( #20077, #140, #6826, #15689 ),
 .UNSPECIFIED., .F., .F.,
 ( 4, 4 ),
 ( 0.000000000000000000, 1.000000000000000000 ),
 .UNSPECIFIED. ) ;
#19180 = ORIENTED_EDGE ( 'NONE', *, *, #2412, .F. ) ;
#19181 = CARTESIAN_POINT ( 'NONE',  ( 21.55427193970000133, -36.12241491659999326, -6.846103682259999879 ) ) ;
#19182 = EDGE_LOOP ( 'NONE', ( #7564, #2051, #5457 ) ) ;
#19183 = CARTESIAN_POINT ( 'NONE',  ( 7.665546204827036192, -37.34293801103260080, -21.51184040533545527 ) ) ;
#19184 = ADVANCED_FACE ( 'NONE', ( #3675 ), #21084, .T. ) ;
#19185 = CARTESIAN_POINT ( 'NONE',  ( -7.593125501599999438, -94.98812477769999418, -22.45811160230000070 ) ) ;
#19186 = CARTESIAN_POINT ( 'NONE',  ( -22.23129158500000102, -94.79581646409999962, -8.137667245660001214 ) ) ;
#19187 = CARTESIAN_POINT ( 'NONE',  ( -15.35318355849999961, -101.1568446010000031, 3.495320071769999704 ) ) ;
#19188 = CARTESIAN_POINT ( 'NONE',  ( -32.72541325773076437, -74.26385168283852067, -22.20255679915483782 ) ) ;
#19189 = CARTESIAN_POINT ( 'NONE',  ( -9.476764215410000247, -80.50000000000000000, 38.08875739639999836 ) ) ;
#19190 = CIRCLE ( 'NONE', #16871, 18.14285714289999873 ) ;
#19191 = ORIENTED_EDGE ( 'NONE', *, *, #23379, .F. ) ;
#19192 = CARTESIAN_POINT ( 'NONE',  ( 0.000000000000000000, -31.69999999999999929, 0.000000000000000000 ) ) ;
#19193 = CARTESIAN_POINT ( 'NONE',  ( -12.47640054220000039, -101.1976625110000043, -10.56652411019999960 ) ) ;
#19194 = AXIS2_PLACEMENT_3D ( 'NONE', #1732, #28524, #19488 ) ;
#19195 = CARTESIAN_POINT ( 'NONE',  ( -2.619606476369999992, -19.50000008899999671, -24.29997799710000095 ) ) ;
#19196 = CARTESIAN_POINT ( 'NONE',  ( -6.942134205095888078, -101.6297509123139662, 14.43170307226528593 ) ) ;
#19197 = ORIENTED_EDGE ( 'NONE', *, *, #10792, .F. ) ;
#19198 = DIRECTION ( 'NONE',  ( 0.4794255386042042266, 0.000000000000000000, 0.8775825618903720926 ) ) ;
#19199 = CARTESIAN_POINT ( 'NONE',  ( -31.89935321680000158, -74.00000000000000000, -21.99985828019999801 ) ) ;
#19200 = CARTESIAN_POINT ( 'NONE',  ( -20.56018235820000228, -57.40875686090000585, 14.85415984670000000 ) ) ;
#19201 = ORIENTED_EDGE ( 'NONE', *, *, #13610, .F. ) ;
#19202 = B_SPLINE_SURFACE_WITH_KNOTS ( 'NONE', 5, 5, ( 
 ( #3609, #3477, #14404, #23570, #20829, #19195 ),
 ( #25352, #16730, #14533, #23157, #5236, #16447 ),
 ( #16589, #25625, #5655, #5381, #3202, #18791 ),
 ( #25482, #23294, #12340, #25764, #10285, #18645 ),
 ( #14676, #14264, #21249, #10142, #3338, #19063 ),
 ( #14121, #889, #1442, #12205, #21117, #28083 ),
 ( #1300, #27947, #16295, #21381, #7984, #5793 ),
 ( #9732, #12470, #25205, #12060, #23019, #3069 ),
 ( #23706, #17146, #1581, #6062, #25897, #10422 ) ),
 .UNSPECIFIED., .F., .F., .F.,
 ( 6, 3, 6 ),
 ( 6, 6 ),
 ( 0.000000000000000000, 2.252774941520000240, 5.576981603780000185 ),
 ( 0.000000000000000000, 1.000000000000000000 ),
 .UNSPECIFIED. ) ;
#19203 = CARTESIAN_POINT ( 'NONE',  ( 36.72530057213035803, -79.26975512441563865, -14.72286002414454309 ) ) ;
#19204 = CARTESIAN_POINT ( 'NONE',  ( 6.817137268750544266, -100.4211561361777285, 15.53426013567950825 ) ) ;
#19205 = B_SPLINE_CURVE_WITH_KNOTS ( 'NONE', 3,
 ( #24893, #22570, #16131, #20516, #20962, #22859, #2901, #11759, #7413, #13804, #2751, #22709, #11458, #11607, #585, #20672, #18337, #9581, #27226, #7266, #732, #7570, #18482, #20813, #876, #16276, #25191, #5222, #16430, #14106, #3054, #9718 ),
 .UNSPECIFIED., .F., .F.,
 ( 4, 2, 1, 1, 1, 2, 2, 2, 1, 1, 1, 2, 2, 2, 1, 1, 1, 1, 2, 2, 4 ),
 ( 0.000000000000000000, 0.1250000000000754119, 0.1875000000001171285, 0.2187500000001439682, 0.2343750000001598166, 0.2421875000001667277, 0.2500000000001736389, 0.3750000000001862954, 0.4375000000001967315, 0.4687500000002018941, 0.4843750000002002842, 0.4921875000002037259, 0.5000000000002071676, 0.6250000000002902123, 0.6875000000003331779, 0.7187500000003561595, 0.7343750000003677059, 0.7421875000003733680, 0.7460937500003761436, 0.7500000000003789191, 1.000000000000000000 ),
 .UNSPECIFIED. ) ;
#19206 = ORIENTED_EDGE ( 'NONE', *, *, #11163, .F. ) ;
#19207 = EDGE_CURVE ( 'NONE', #14702, #6476, #12695, .T. ) ;
#19208 = CARTESIAN_POINT ( 'NONE',  ( -17.32209284807034422, -99.34292914276410613, 3.453906795064102031 ) ) ;
#19209 = AXIS2_PLACEMENT_3D ( 'NONE', #12357, #3632, #26207 ) ;
#19210 = CARTESIAN_POINT ( 'NONE',  ( 20.98165098409999985, -53.83744478090000030, 10.43394308190000075 ) ) ;
#19211 = CARTESIAN_POINT ( 'NONE',  ( -38.55000000000000426, -63.07912966450000880, 2.857883832489999776 ) ) ;
#19212 = CARTESIAN_POINT ( 'NONE',  ( -7.314390784529999578, -73.97626148509999666, -39.54176628510000313 ) ) ;
#19213 = ORIENTED_EDGE ( 'NONE', *, *, #5013, .T. ) ;
#19214 = EDGE_CURVE ( 'NONE', #20556, #19071, #180, .T. ) ;
#19215 = TOROIDAL_SURFACE ( 'NONE', #8054, 55.85192378860000417, 0.3499999999999999778 ) ;
#19216 = DIRECTION ( 'NONE',  ( 0.000000000000000000, 1.000000000000000000, 0.000000000000000000 ) ) ;
#19217 = CARTESIAN_POINT ( 'NONE',  ( 22.92823879609795057, -37.07368284069996633, -9.571688886919444528 ) ) ;
#19218 = EDGE_CURVE ( 'NONE', #4674, #28301, #16800, .T. ) ;
#19219 = ORIENTED_EDGE ( 'NONE', *, *, #27147, .F. ) ;
#19220 = FACE_OUTER_BOUND ( 'NONE', #826, .T. ) ;
#19221 = CARTESIAN_POINT ( 'NONE',  ( 22.97877291159999658, -37.99999999279999230, -9.393614097370001303 ) ) ;
#19222 = DIRECTION ( 'NONE',  ( -0.8775825618903722036, 0.000000000000000000, 0.4794255386042041156 ) ) ;
#19223 = ORIENTED_EDGE ( 'NONE', *, *, #20569, .F. ) ;
#19224 = CARTESIAN_POINT ( 'NONE',  ( -22.23129207539999896, -94.79581469870001342, -8.137668203089999608 ) ) ;
#19225 = CARTESIAN_POINT ( 'NONE',  ( 13.20150262729999824, -100.5717442099999914, -9.613817315349999504 ) ) ;
#19226 = CARTESIAN_POINT ( 'NONE',  ( -20.41946551879999561, -93.96465009399999246, 14.25054530959999965 ) ) ;
#19227 = CARTESIAN_POINT ( 'NONE',  ( 24.01103065379999890, -94.15497152590000951, -8.177649200119999406 ) ) ;
#19228 = EDGE_LOOP ( 'NONE', ( #4633, #7172, #15584, #12995 ) ) ;
#19229 = CIRCLE ( 'NONE', #26195, 0.9999999999999997780 ) ;
#19230 = CARTESIAN_POINT ( 'NONE',  ( -3.562216355159999903, -80.49999996399999702, 46.31451622859999873 ) ) ;
#19231 = CARTESIAN_POINT ( 'NONE',  ( -18.99880662649999863, -18.62181730670000235, 14.46168826759999959 ) ) ;
#19232 = ORIENTED_EDGE ( 'NONE', *, *, #6843, .F. ) ;
#19233 = FACE_OUTER_BOUND ( 'NONE', #1668, .T. ) ;
#19234 = FACE_OUTER_BOUND ( 'NONE', #27261, .T. ) ;
#19235 = CARTESIAN_POINT ( 'NONE',  ( 38.67409491847346459, -73.94611239985914608, 7.370697001239634005 ) ) ;
#19236 = DIRECTION ( 'NONE',  ( 1.000000000000000000, 0.000000000000000000, 0.000000000000000000 ) ) ;
#19237 = DIRECTION ( 'NONE',  ( 1.000000000000000000, 0.000000000000000000, 0.000000000000000000 ) ) ;
#19238 = CIRCLE ( 'NONE', #21567, 3.000000000000000000 ) ;
#19240 = EDGE_LOOP ( 'NONE', ( #15252, #5102, #12466, #21572 ) ) ;
#19239 = EDGE_CURVE ( 'NONE', #6357, #15974, #18395, .T. ) ;
#19241 = EDGE_CURVE ( 'NONE', #7122, #27225, #3872, .T. ) ;
#19242 = AXIS2_PLACEMENT_3D ( 'NONE', #1077, #5418, #5831 ) ;
#19243 = CARTESIAN_POINT ( 'NONE',  ( 19.54737287369999876, -35.65078480380000059, -9.004240688089998557 ) ) ;
#19244 = ORIENTED_EDGE ( 'NONE', *, *, #18813, .T. ) ;
#19245 = AXIS2_PLACEMENT_3D ( 'NONE', #2396, #17401, #20158 ) ;
#19246 = CARTESIAN_POINT ( 'NONE',  ( 20.25798860239999755, -35.94310217329999801, -9.093914510570000331 ) ) ;
#19247 = CARTESIAN_POINT ( 'NONE',  ( 19.57844007279999943, -94.59276583650000703, 13.52683266610000068 ) ) ;
#19248 = ORIENTED_EDGE ( 'NONE', *, *, #17367, .F. ) ;
#19249 = EDGE_CURVE ( 'NONE', #2258, #17070, #20164, .T. ) ;
#19250 = CARTESIAN_POINT ( 'NONE',  ( 10.49903398999999915, -97.54012249449999672, 17.04265490439999908 ) ) ;
#19251 = CARTESIAN_POINT ( 'NONE',  ( -15.08165013250000008, -92.59475633059999211, -24.08137820129999795 ) ) ;
#19252 = CARTESIAN_POINT ( 'NONE',  ( -2.770815202149999656, -99.67742714719999242, -17.41576461069999837 ) ) ;
#19253 = CARTESIAN_POINT ( 'NONE',  ( -7.593125501599999438, -94.98812477769999418, -22.45811160230000070 ) ) ;
#19254 = DIRECTION ( 'NONE',  ( 1.000000000000000000, 0.000000000000000000, 0.000000000000000000 ) ) ;
#19255 = TOROIDAL_SURFACE ( 'NONE', #28093, 7.750000000000000000, 0.5000000000000000000 ) ;
#19256 = DIRECTION ( 'NONE',  ( 1.000000000000000000, 0.000000000000000000, 0.000000000000000000 ) ) ;
#19257 = ORIENTED_EDGE ( 'NONE', *, *, #25919, .F. ) ;
#19258 = CARTESIAN_POINT ( 'NONE',  ( 13.13687359478633532, -101.1248211535440760, -9.828810838103104075 ) ) ;
#19259 = CARTESIAN_POINT ( 'NONE',  ( -27.33231135720000182, -92.65509162889999573, -4.521837785309999802 ) ) ;
#19260 = CARTESIAN_POINT ( 'NONE',  ( -13.07632843636527475, -19.48670010342060976, 19.73696929114215237 ) ) ;
#19261 = CARTESIAN_POINT ( 'NONE',  ( -15.58411797090000128, -101.6484611620000038, 3.625951500279999795 ) ) ;
#19262 = ORIENTED_EDGE ( 'NONE', *, *, #14508, .T. ) ;
#19263 = CARTESIAN_POINT ( 'NONE',  ( 19.70300571909999832, -18.50000000000000000, -8.011708434370000020 ) ) ;
#19264 = CARTESIAN_POINT ( 'NONE',  ( -14.58326278150000022, -74.39167553240000075, 36.61803022830000032 ) ) ;
#19265 = DIRECTION ( 'NONE',  ( 0.000000000000000000, 1.000000000000000000, 0.000000000000000000 ) ) ;
#19266 = LINE ( 'NONE', #28701, #27549 ) ;
#19267 = ORIENTED_EDGE ( 'NONE', *, *, #17934, .F. ) ;
#19268 = AXIS2_PLACEMENT_3D ( 'NONE', #28329, #16984, #17413 ) ;
#19269 = CARTESIAN_POINT ( 'NONE',  ( 2.842170943039999687E-14, -72.82938648530000592, 1.776356839399999804E-15 ) ) ;
#19270 = B_SPLINE_CURVE_WITH_KNOTS ( 'NONE', 5,
 ( #16152, #9740, #13974, #22879, #14127, #7589, #3076, #22438, #7143 ),
 .UNSPECIFIED., .F., .F.,
 ( 6, 3, 6 ),
 ( 0.000000000000000000, 1.237573681340000009, 1.566718891470000097 ),
 .UNSPECIFIED. ) ;
#19271 = ADVANCED_FACE ( 'NONE', ( #8313 ), #16640, .T. ) ;
#19272 = CIRCLE ( 'NONE', #22064, 21.14285714289999873 ) ;
#19273 = CARTESIAN_POINT ( 'NONE',  ( -0.09996363298640001394, -101.1716782170000073, -15.73370943089999763 ) ) ;
#19274 = FACE_OUTER_BOUND ( 'NONE', #24449, .T. ) ;
#19275 = CARTESIAN_POINT ( 'NONE',  ( 15.91666809940000071, -101.0685849509999912, 2.371725914449999806 ) ) ;
#19276 = CARTESIAN_POINT ( 'NONE',  ( 20.65722554970000147, -57.91738531389999878, 10.94680766110000114 ) ) ;
#19277 = DIRECTION ( 'NONE',  ( 0.000000000000000000, 1.000000000000000000, 0.000000000000000000 ) ) ;
#19278 = ORIENTED_EDGE ( 'NONE', *, *, #6922, .T. ) ;
#19279 = CARTESIAN_POINT ( 'NONE',  ( 6.166664293190000201, -100.8815367389999977, 14.41068211719999859 ) ) ;
#19280 = CARTESIAN_POINT ( 'NONE',  ( 15.16640347679999934, -101.0151300849999814, 3.812177866399999893 ) ) ;
#19281 = TOROIDAL_SURFACE ( 'NONE', #10412, 13.00000000000000000, 2.000000000000000000 ) ;
#19282 = ADVANCED_FACE ( 'NONE', ( #17214 ), #7634, .T. ) ;
#19283 = EDGE_CURVE ( 'NONE', #898, #21056, #9925, .T. ) ;
#19284 = CARTESIAN_POINT ( 'NONE',  ( -40.31103002510583622, -65.70299785167240714, -2.224975054963230114 ) ) ;
#19285 = DIRECTION ( 'NONE',  ( -0.8775825618903722036, 0.000000000000000000, 0.4794255386042041156 ) ) ;
#19286 = CIRCLE ( 'NONE', #6732, 2.500000000000000444 ) ;
#19287 = DIRECTION ( 'NONE',  ( 1.000000000000000000, 0.000000000000000000, 0.000000000000000000 ) ) ;
#19288 = ORIENTED_EDGE ( 'NONE', *, *, #21964, .T. ) ;
#19289 = CARTESIAN_POINT ( 'NONE',  ( 6.330503061179999946, -92.97898997910000674, -25.99767272040000066 ) ) ;
#19290 = LINE ( 'NONE', #15029, #25282 ) ;
#19291 = CARTESIAN_POINT ( 'NONE',  ( 0.000000000000000000, -39.50000000000000000, 0.000000000000000000 ) ) ;
#19292 = CARTESIAN_POINT ( 'NONE',  ( -37.75000000000000000, -63.00000000000000000, 0.7216878364859999895 ) ) ;
#19293 = ORIENTED_EDGE ( 'NONE', *, *, #1993, .F. ) ;
#19294 = CIRCLE ( 'NONE', #1171, 30.50000000000000000 ) ;
#19295 = DIRECTION ( 'NONE',  ( 0.000000000000000000, 1.000000000000000000, 0.000000000000000000 ) ) ;
#19296 = DIRECTION ( 'NONE',  ( 1.000000000000000000, 0.000000000000000000, 0.000000000000000000 ) ) ;
#19297 = ORIENTED_EDGE ( 'NONE', *, *, #1831, .F. ) ;
#19298 = ORIENTED_EDGE ( 'NONE', *, *, #18644, .T. ) ;
#19299 = CARTESIAN_POINT ( 'NONE',  ( -0.9785950990579999065, -101.1045726949999874, -15.50412976750000205 ) ) ;
#19300 = DIRECTION ( 'NONE',  ( 0.4794255386042036715, 0.000000000000000000, 0.8775825618903724257 ) ) ;
#19301 = CARTESIAN_POINT ( 'NONE',  ( -13.10652098802392373, -92.87497309988854965, -23.83816252673762293 ) ) ;
#19302 = CARTESIAN_POINT ( 'NONE',  ( 26.57254216609999986, -73.97490553219999754, -28.93874024099999787 ) ) ;
#19303 = SPHERICAL_SURFACE ( 'NONE', #11331, 2.000000035459999825 ) ;
#19304 = EDGE_CURVE ( 'NONE', #9596, #28564, #13650, .T. ) ;
#19305 = EDGE_CURVE ( 'NONE', #28456, #178, #25768, .T. ) ;
#19306 = CARTESIAN_POINT ( 'NONE',  ( -21.60034937969999902, -82.25000000000000000, -32.77174707999999725 ) ) ;
#19307 = CARTESIAN_POINT ( 'NONE',  ( -19.03439102309033260, -19.48534489991826746, 13.93933370342093170 ) ) ;
#19308 = CARTESIAN_POINT ( 'NONE',  ( 23.84064839501263933, -94.60934249635550941, -7.609331551989225950 ) ) ;
#19309 = CARTESIAN_POINT ( 'NONE',  ( 0.000000000000000000, -42.50000000000000000, 0.000000000000000000 ) ) ;
#19310 = ORIENTED_EDGE ( 'NONE', *, *, #2149, .T. ) ;
#19311 = EDGE_CURVE ( 'NONE', #4465, #26488, #19398, .T. ) ;
#19312 = FACE_OUTER_BOUND ( 'NONE', #8522, .T. ) ;
#19313 = CIRCLE ( 'NONE', #12316, 21.14285714289999873 ) ;
#19314 = B_SPLINE_CURVE_WITH_KNOTS ( 'NONE', 5,
 ( #19564, #19841, #15312, #1530, #13139, #10375 ),
 .UNSPECIFIED., .F., .F.,
 ( 6, 6 ),
 ( 0.000000000000000000, 1.000000000000000000 ),
 .UNSPECIFIED. ) ;
#19315 = ORIENTED_EDGE ( 'NONE', *, *, #21067, .F. ) ;
#19316 = CARTESIAN_POINT ( 'NONE',  ( 22.97877291129999833, -37.68584072819999875, -9.393614098449999616 ) ) ;
#19317 = ADVANCED_FACE ( 'NONE', ( #21729 ), #28534, .F. ) ;
#19318 = ORIENTED_EDGE ( 'NONE', *, *, #16193, .F. ) ;
#19319 = CARTESIAN_POINT ( 'NONE',  ( -2.618120360420000292, -61.37513324760000444, -25.61258802169999882 ) ) ;
#19320 = DIRECTION ( 'NONE',  ( 0.000000000000000000, 1.000000000000000000, 0.000000000000000000 ) ) ;
#19321 = DIRECTION ( 'NONE',  ( 0.000000000000000000, 1.000000000000000000, 0.000000000000000000 ) ) ;
#19322 = DIRECTION ( 'NONE',  ( 0.4794255386042036715, 0.000000000000000000, 0.8775825618903724257 ) ) ;
#19323 = B_SPLINE_CURVE_WITH_KNOTS ( 'NONE', 3,
 ( #20300, #11693, #665, #9212, #9073, #371, #27017, #11544, #9517, #16211 ),
 .UNSPECIFIED., .F., .F.,
 ( 4, 2, 2, 2, 4 ),
 ( 0.000000000000000000, 0.2500000000000000555, 0.5000000000000000000, 0.7500000000000000000, 1.000000000000000000 ),
 .UNSPECIFIED. ) ;
#19324 = DIRECTION ( 'NONE',  ( 1.000000000000000000, 0.000000000000000000, 0.000000000000000000 ) ) ;
#19326 = AXIS2_PLACEMENT_3D ( 'NONE', #25930, #28387, #17325 ) ;
#19325 = CARTESIAN_POINT ( 'NONE',  ( 15.51959124780000110, -100.8455998110000138, 4.065823162090000054 ) ) ;
#19327 = EDGE_LOOP ( 'NONE', ( #15035, #26531, #4417, #12726 ) ) ;
#19328 = CARTESIAN_POINT ( 'NONE',  ( -18.58472001550576991, -97.05288880472299695, -9.904339515219520607 ) ) ;
#19329 = CARTESIAN_POINT ( 'NONE',  ( 4.426600958609999879E-15, -79.00000000000000000, 43.75000000000000000 ) ) ;
#19330 = ORIENTED_EDGE ( 'NONE', *, *, #22180, .F. ) ;
#19331 = CARTESIAN_POINT ( 'NONE',  ( 0.000000000000000000, -15.80000000000000071, 0.000000000000000000 ) ) ;
#19332 = CARTESIAN_POINT ( 'NONE',  ( -7.384731607069999981, -94.63960343449998902, -22.55849074379999664 ) ) ;
#19333 = CARTESIAN_POINT ( 'NONE',  ( 21.70051260119999625, -18.62107711730000048, 9.116757753519999952 ) ) ;
#19334 = CARTESIAN_POINT ( 'NONE',  ( 23.35417726449999876, -57.47855601710000428, -0.5711878197419999470 ) ) ;
#19335 = DIRECTION ( 'NONE',  ( 1.000000000000000000, 0.000000000000000000, 0.000000000000000000 ) ) ;
#19336 = ORIENTED_EDGE ( 'NONE', *, *, #13238, .T. ) ;
#19337 = CARTESIAN_POINT ( 'NONE',  ( 19.90443298253104842, -98.49786007137258537, -0.8521435990548464900 ) ) ;
#19338 = CARTESIAN_POINT ( 'NONE',  ( -12.48549849059999950, -101.5964542560000012, -10.07002115010000054 ) ) ;
#19339 = EDGE_CURVE ( 'NONE', #2162, #10257, #23444, .T. ) ;
#19340 = CARTESIAN_POINT ( 'NONE',  ( 17.27104901786038837, -94.65677004888377155, 16.86278722961666077 ) ) ;
#19341 = CARTESIAN_POINT ( 'NONE',  ( -7.233742488672582738, -101.4728631013542497, 14.42332162610310853 ) ) ;
#19342 = ORIENTED_EDGE ( 'NONE', *, *, #17415, .F. ) ;
#19343 = ADVANCED_FACE ( 'NONE', ( #18349 ), #20840, .F. ) ;
#19344 = CARTESIAN_POINT ( 'NONE',  ( 0.000000000000000000, -17.50000000000000000, 0.000000000000000000 ) ) ;
#19345 = CARTESIAN_POINT ( 'NONE',  ( 37.06867693649999751, -79.93087181439999256, -14.15266191389999939 ) ) ;
#19346 = ORIENTED_EDGE ( 'NONE', *, *, #5830, .F. ) ;
#19347 = EDGE_CURVE ( 'NONE', #25813, #16909, #24302, .T. ) ;
#19348 = EDGE_CURVE ( 'NONE', #21477, #103, #5650, .T. ) ;
#19349 = CARTESIAN_POINT ( 'NONE',  ( 6.802592131508781392, -100.4507315472249331, 15.51479369704953371 ) ) ;
#19350 = VECTOR ( 'NONE', #9343, 1000.000000000000000 ) ;
#19351 = CARTESIAN_POINT ( 'NONE',  ( -1.780211689454020751, -80.14649671107554241, 47.02804128279894513 ) ) ;
#19352 = EDGE_LOOP ( 'NONE', ( #21841, #19558, #9279, #4207 ) ) ;
#19353 = DIRECTION ( 'NONE',  ( -0.4151946956541399669, 0.5000000000001689759, -0.7600087925152558821 ) ) ;
#19354 = ORIENTED_EDGE ( 'NONE', *, *, #26735, .F. ) ;
#19355 = CARTESIAN_POINT ( 'NONE',  ( 20.45876929980000369, -56.26715181569999658, 11.18963356429999934 ) ) ;
#19356 = FACE_OUTER_BOUND ( 'NONE', #12860, .T. ) ;
#19357 = CARTESIAN_POINT ( 'NONE',  ( -7.305170733980000719, -74.19145785139998850, -39.89387480210000092 ) ) ;
#19358 = EDGE_LOOP ( 'NONE', ( #15597, #23562, #26306, #13525 ) ) ;
#19359 = CARTESIAN_POINT ( 'NONE',  ( 9.807088892109998568, -36.00000000000000000, -20.27618918270000137 ) ) ;
#19360 = FACE_OUTER_BOUND ( 'NONE', #2390, .T. ) ;
#19361 = CARTESIAN_POINT ( 'NONE',  ( 22.70406349567018722, -37.99004392654882878, -9.315656979556900197 ) ) ;
#19362 = CARTESIAN_POINT ( 'NONE',  ( -23.42541176010000115, -92.63555401869999173, -19.15044151010000206 ) ) ;
#19363 = CARTESIAN_POINT ( 'NONE',  ( -2.481488253459999793, -18.50000000000000000, -21.63557997309999692 ) ) ;
#19364 = EDGE_LOOP ( 'NONE', ( #9612, #697, #25204, #23223 ) ) ;
#19365 = CARTESIAN_POINT ( 'NONE',  ( 19.55068592539999983, -35.72724453810000256, -9.038647860560001135 ) ) ;
#19366 = CARTESIAN_POINT ( 'NONE',  ( 13.56595000559999953, -100.1785804069999983, -9.651294529659999455 ) ) ;
#19367 = CARTESIAN_POINT ( 'NONE',  ( -19.58183770029999948, -93.00000000000000000, 20.70264511730000123 ) ) ;
#19368 = CARTESIAN_POINT ( 'NONE',  ( 24.19872769330000040, -92.53610956480000027, -16.95184105959999954 ) ) ;
#19369 = EDGE_CURVE ( 'NONE', #14137, #27440, #7657, .T. ) ;
#19370 = CARTESIAN_POINT ( 'NONE',  ( -38.40529884094686253, -65.09475709727961146, 2.889773311245127374 ) ) ;
#19371 = CARTESIAN_POINT ( 'NONE',  ( -38.25000000000000000, -65.21397798589998729, -2.551096136590000008 ) ) ;
#19372 = EDGE_LOOP ( 'NONE', ( #5795, #12218, #15011, #22694 ) ) ;
#19373 = EDGE_CURVE ( 'NONE', #15723, #9549, #17706, .T. ) ;
#19374 = CARTESIAN_POINT ( 'NONE',  ( -19.41104744409999938, -19.40610837510000053, 14.28697461880000041 ) ) ;
#19375 = CARTESIAN_POINT ( 'NONE',  ( 38.71640881029999548, -73.50000064450000536, 7.135467304789999687 ) ) ;
#19376 = CARTESIAN_POINT ( 'NONE',  ( 7.356933064080000584, -36.56811125840000187, -21.47791245320000186 ) ) ;
#19377 = CARTESIAN_POINT ( 'NONE',  ( -14.07395139057579669, -74.01137367045767235, 36.22381386828725169 ) ) ;
#19378 = ADVANCED_FACE ( 'NONE', ( #28351 ), #1603, .T. ) ;
#19379 = DIRECTION ( 'NONE',  ( -1.000000000000000000, 0.000000000000000000, 0.000000000000000000 ) ) ;
#19380 = ORIENTED_EDGE ( 'NONE', *, *, #2685, .T. ) ;
#19381 = DIRECTION ( 'NONE',  ( 0.000000000000000000, 1.000000000000000000, 0.000000000000000000 ) ) ;
#19382 = CARTESIAN_POINT ( 'NONE',  ( 20.12810827960000282, -35.68342701319999577, -8.993407668519999731 ) ) ;
#19383 = VERTEX_POINT ( 'NONE', #17003 ) ;
#19384 = CARTESIAN_POINT ( 'NONE',  ( 21.44636399800000248, -36.83820790320000782, -8.385252985220001065 ) ) ;
#19385 = DIRECTION ( 'NONE',  ( 0.000000000000000000, 1.000000000000000000, 0.000000000000000000 ) ) ;
#19386 = ORIENTED_EDGE ( 'NONE', *, *, #18345, .F. ) ;
#19387 = CARTESIAN_POINT ( 'NONE',  ( 9.335817441729998833, -98.58684426249999433, 16.46450815360000064 ) ) ;
#19388 = DIRECTION ( 'NONE',  ( 1.000000000000000000, 0.000000000000000000, 0.000000000000000000 ) ) ;
#19389 = CARTESIAN_POINT ( 'NONE',  ( 1.908610474560000103, -93.01085527740001169, 27.31676936940000289 ) ) ;
#19390 = CARTESIAN_POINT ( 'NONE',  ( 7.952618468089998949, -53.29009989829999938, -22.02398067749999910 ) ) ;
#19391 = CARTESIAN_POINT ( 'NONE',  ( -39.80530703708314633, -65.72848773095162755, 2.193893542354256709 ) ) ;
#19392 = ORIENTED_EDGE ( 'NONE', *, *, #5632, .F. ) ;
#19393 = CARTESIAN_POINT ( 'NONE',  ( 13.67589891821544867, -100.3266728693051704, -10.16527262647603891 ) ) ;
#19394 = CARTESIAN_POINT ( 'NONE',  ( 23.09634100869999784, -49.87554870529999818, -0.2593201272430000204 ) ) ;
#19395 = CARTESIAN_POINT ( 'NONE',  ( 23.44226622849999941, -65.21231684830000574, 10.79519211999999939 ) ) ;
#19396 = CARTESIAN_POINT ( 'NONE',  ( 9.374859430949999961, -94.98812769030000425, -22.63661719490000124 ) ) ;
#19397 = ORIENTED_EDGE ( 'NONE', *, *, #25295, .T. ) ;
#19398 = LINE ( 'NONE', #3957, #12254 ) ;
#19399 = ADVANCED_FACE ( 'NONE', ( #8114 ), #21517, .T. ) ;
#19400 = CARTESIAN_POINT ( 'NONE',  ( -14.59431547039999977, -74.43317772470001614, 36.62860707189999943 ) ) ;
#19401 = LINE ( 'NONE', #14605, #28317 ) ;
#19402 = DIRECTION ( 'NONE',  ( 0.000000000000000000, 1.000000000000000000, 0.000000000000000000 ) ) ;
#19403 = ORIENTED_EDGE ( 'NONE', *, *, #865, .T. ) ;
#19404 = VECTOR ( 'NONE', #8996, 1000.000000000000000 ) ;
#19405 = EDGE_CURVE ( 'NONE', #13313, #8306, #17576, .T. ) ;
#19406 = CARTESIAN_POINT ( 'NONE',  ( -1.240000067321601396, -74.19110756884491309, 47.14321378798046425 ) ) ;
#19407 = CARTESIAN_POINT ( 'NONE',  ( 0.1181328008709999905, -101.0956037589999994, -15.54443271709999941 ) ) ;
#19408 = CARTESIAN_POINT ( 'NONE',  ( 26.97200738714188617, -92.55389105862651888, -12.40203756692639558 ) ) ;
#19409 = CARTESIAN_POINT ( 'NONE',  ( -12.07234849260000153, -68.56747070539999811, -25.18735587219999772 ) ) ;
#19410 = CARTESIAN_POINT ( 'NONE',  ( 20.53475899579999719, -58.35721741809999941, 11.22800282539999905 ) ) ;
#19411 = AXIS2_PLACEMENT_3D ( 'NONE', #7889, #16912, #10183 ) ;
#19412 = DIRECTION ( 'NONE',  ( 0.000000000000000000, -1.000000000000000000, 0.000000000000000000 ) ) ;
#19413 = ORIENTED_EDGE ( 'NONE', *, *, #17123, .F. ) ;
#19414 = CARTESIAN_POINT ( 'NONE',  ( 6.390608560400000471, -100.1785804069999983, 15.37343838830000031 ) ) ;
#19415 = CARTESIAN_POINT ( 'NONE',  ( 15.58330902049999978, -101.3852859389999992, 3.598700821059999999 ) ) ;
#19416 = VECTOR ( 'NONE', #11856, 1000.000000000000000 ) ;
#19417 = CARTESIAN_POINT ( 'NONE',  ( 8.956866503930001500, -35.50841500800000716, -20.05333527200000177 ) ) ;
#19418 = CARTESIAN_POINT ( 'NONE',  ( 22.06868239059999937, -18.50000000000000000, 1.779150257960000037 ) ) ;
#19419 = VERTEX_POINT ( 'NONE', #10840 ) ;
#19420 = CARTESIAN_POINT ( 'NONE',  ( 8.893989049490000909, -94.22485739640001157, -23.02234954029999869 ) ) ;
#19421 = TOROIDAL_SURFACE ( 'NONE', #2684, 18.14285714289999873, 0.5000000000000000000 ) ;
#19422 = STYLED_ITEM ( 'NONE', ( #15171 ), #15722 ) ;
#19423 = EDGE_CURVE ( 'NONE', #2030, #10820, #21139, .T. ) ;
#19424 = FACE_OUTER_BOUND ( 'NONE', #22644, .T. ) ;
#19425 = CARTESIAN_POINT ( 'NONE',  ( -10.50000000000000000, -19.00000000000000000, 1.748601263780000010E-15 ) ) ;
#19426 = VERTEX_POINT ( 'NONE', #15363 ) ;
#19427 = DIRECTION ( 'NONE',  ( 0.000000000000000000, 1.000000000000000000, 0.000000000000000000 ) ) ;
#19428 = CARTESIAN_POINT ( 'NONE',  ( -12.48293756425525913, -101.2021794472807130, -10.55357194642999907 ) ) ;
#19429 = ORIENTED_EDGE ( 'NONE', *, *, #9552, .T. ) ;
#19430 = CARTESIAN_POINT ( 'NONE',  ( -1.179661616630000021, -101.0555477039999914, -15.45190212829999865 ) ) ;
#19431 = CARTESIAN_POINT ( 'NONE',  ( 22.02882266680000001, -19.46510059719999930, -0.4636565024600000084 ) ) ;
#19432 = CARTESIAN_POINT ( 'NONE',  ( 0.000000000000000000, -94.59276292389999696, 0.000000000000000000 ) ) ;
#19433 = CARTESIAN_POINT ( 'NONE',  ( -32.77174708219999388, -74.50000000000000000, -21.60034937629999874 ) ) ;
#19434 = AXIS2_PLACEMENT_3D ( 'NONE', #18099, #24811, #15607 ) ;
#19435 = EDGE_CURVE ( 'NONE', #20924, #3048, #24624, .T. ) ;
#19436 = CARTESIAN_POINT ( 'NONE',  ( -23.16987202530000189, -72.82938842069999907, 16.90923852390000093 ) ) ;
#19437 = B_SPLINE_SURFACE_WITH_KNOTS ( 'NONE', 5, 5, ( 
 ( #19166, #28053, #21494, #14647, #14774, #1685 ),
 ( #23543, #19030, #27916, #23675, #10524, #19439 ),
 ( #3719, #12579, #19863, #4433, #4576, #22358 ),
 ( #28744, #6625, #24396, #13304, #22209, #238 ),
 ( #7068, #15333, #17549, #11407, #10953, #6774 ),
 ( #15486, #15784, #19725, #1973, #8644, #27025 ) ),
 .UNSPECIFIED., .F., .F., .F.,
 ( 6, 6 ),
 ( 6, 6 ),
 ( 26.13957982610000030, 31.08299525409999831 ),
 ( 0.000000000000000000, 2.000000000000000000 ),
 .UNSPECIFIED. ) ;
#19438 = CARTESIAN_POINT ( 'NONE',  ( -14.64568814080000081, -101.2530993010000060, 4.044604232330000215 ) ) ;
#19439 = CARTESIAN_POINT ( 'NONE',  ( -12.98506133270000085, -65.72122283929999753, -21.88189319379999986 ) ) ;
#19440 = PLANE ( 'NONE',  #19268 ) ;
#19441 = ORIENTED_EDGE ( 'NONE', *, *, #2371, .F. ) ;
#19442 = EDGE_CURVE ( 'NONE', #11263, #24995, #1025, .T. ) ;
#19443 = CARTESIAN_POINT ( 'NONE',  ( 6.114061450890000415, -93.00000000000000000, -13.40104985119999981 ) ) ;
#19444 = AXIS2_PLACEMENT_3D ( 'NONE', #21692, #10581, #1740 ) ;
#19445 = ORIENTED_EDGE ( 'NONE', *, *, #8998, .T. ) ;
#19446 = CARTESIAN_POINT ( 'NONE',  ( 22.65555239909999941, -37.06806482060000008, -9.497542709419999341 ) ) ;
#19447 = ORIENTED_EDGE ( 'NONE', *, *, #25450, .F. ) ;
#19448 = CARTESIAN_POINT ( 'NONE',  ( -1.977440293640000402, -58.73757401350000151, -23.91133900879999885 ) ) ;
#19449 = CARTESIAN_POINT ( 'NONE',  ( -28.96583554960000129, -92.87863185420000889, 3.120909019039999954 ) ) ;
#19450 = CARTESIAN_POINT ( 'NONE',  ( -41.74999999998802025, -63.17171877515596634, -2.272201163158487969 ) ) ;
#19451 = CARTESIAN_POINT ( 'NONE',  ( -19.81272040990000249, -52.63293862049999916, 12.05498172269999912 ) ) ;
#19452 = EDGE_CURVE ( 'NONE', #7443, #24926, #286, .T. ) ;
#19453 = CARTESIAN_POINT ( 'NONE',  ( 15.53901966880000174, -100.4731125450000064, 4.587699026339999264 ) ) ;
#19454 = VERTEX_POINT ( 'NONE', #22544 ) ;
#19455 = CARTESIAN_POINT ( 'NONE',  ( 21.18066447389999851, -34.91901312109999367, -7.923301732400000574 ) ) ;
#19456 = CARTESIAN_POINT ( 'NONE',  ( 7.323177335909999641, -73.87252278319999732, -39.07223452299999167 ) ) ;
#19457 = ORIENTED_EDGE ( 'NONE', *, *, #17270, .F. ) ;
#19458 = CARTESIAN_POINT ( 'NONE',  ( 7.939780906490000234, -111.0000000000000000, 14.74863990870000130 ) ) ;
#19459 = CIRCLE ( 'NONE', #17134, 30.50000000000000000 ) ;
#19460 = EDGE_CURVE ( 'NONE', #21679, #12727, #26236, .T. ) ;
#19461 = CARTESIAN_POINT ( 'NONE',  ( 38.96762186381851478, -74.02518375729582090, 7.561767225083936061 ) ) ;
#19462 = CARTESIAN_POINT ( 'NONE',  ( 22.96746030019999907, -18.50000000000000000, 9.091461201590000485 ) ) ;
#19463 = CARTESIAN_POINT ( 'NONE',  ( -19.65424240789999999, -57.45864753259999702, 13.63538986699999889 ) ) ;
#19464 = ORIENTED_EDGE ( 'NONE', *, *, #24953, .T. ) ;
#19465 = DIRECTION ( 'NONE',  ( 0.4794255386042036715, 0.000000000000000000, 0.8775825618903724257 ) ) ;
#19466 = CARTESIAN_POINT ( 'NONE',  ( -12.41979737689999830, -101.2927714249999980, -10.17404332349999940 ) ) ;
#19467 =( NAMED_UNIT ( * ) PLANE_ANGLE_UNIT ( ) SI_UNIT ( $, .RADIAN. ) );
#19468 = PLANE ( 'NONE',  #19162 ) ;
#19469 = ORIENTED_EDGE ( 'NONE', *, *, #3466, .T. ) ;
#19470 = VECTOR ( 'NONE', #15752, 1000.000000000000000 ) ;
#19471 = CARTESIAN_POINT ( 'NONE',  ( -1.022274391844619545, -101.5620304352384977, -16.03241640329728668 ) ) ;
#19472 = CARTESIAN_POINT ( 'NONE',  ( -32.69122048629999711, -74.22019266179999875, -22.19435191799999885 ) ) ;
#19473 = VERTEX_POINT ( 'NONE', #28637 ) ;
#19474 = TOROIDAL_SURFACE ( 'NONE', #2767, 3.500000000000000000, 0.5000000000000000000 ) ;
#19475 = AXIS2_PLACEMENT_3D ( 'NONE', #23817, #1549, #27777 ) ;
#19476 = CIRCLE ( 'NONE', #1823, 39.25000000000000000 ) ;
#19477 = AXIS2_PLACEMENT_3D ( 'NONE', #9969, #14490, #23251 ) ;
#19478 = CARTESIAN_POINT ( 'NONE',  ( 11.44042105559999989, -101.2530993000000024, -9.998588429619998053 ) ) ;
#19479 = ORIENTED_EDGE ( 'NONE', *, *, #18924, .F. ) ;
#19480 = CARTESIAN_POINT ( 'NONE',  ( 5.798028723799999791E-12, -111.0000000000000000, -1.541933247750000003E-12 ) ) ;
#19481 = ORIENTED_EDGE ( 'NONE', *, *, #22890, .T. ) ;
#19482 = CARTESIAN_POINT ( 'NONE',  ( 21.05079011269999967, -56.25996389440000200, 10.47764512320000030 ) ) ;
#19483 = CARTESIAN_POINT ( 'NONE',  ( -38.25000000000000000, -63.07912966450000880, 2.684678751729999480 ) ) ;
#19484 = CARTESIAN_POINT ( 'NONE',  ( 2.842132195609999634, -93.86302664969998943, 24.60248089030000074 ) ) ;
#19485 = ORIENTED_EDGE ( 'NONE', *, *, #4825, .T. ) ;
#19486 = PRODUCT_RELATED_PRODUCT_CATEGORY ( 'part', '', ( #1309 ) ) ;
#19487 = CARTESIAN_POINT ( 'NONE',  ( 0.3872056760440000245, -99.92967571559999840, -17.35614698070000017 ) ) ;
#19488 = DIRECTION ( 'NONE',  ( 1.000000000000000000, 0.000000000000000000, 0.000000000000000000 ) ) ;
#19489 = ADVANCED_FACE ( 'NONE', ( #114 ), #23168, .T. ) ;
#19490 = VECTOR ( 'NONE', #2806, 1000.000000000000000 ) ;
#19491 = ORIENTED_EDGE ( 'NONE', *, *, #6512, .T. ) ;
#19492 = FACE_OUTER_BOUND ( 'NONE', #25176, .T. ) ;
#19493 = EDGE_CURVE ( 'NONE', #4465, #18453, #14147, .T. ) ;
#19494 = CARTESIAN_POINT ( 'NONE',  ( -20.44249130340000065, -92.65997669530000280, -20.57397485069999732 ) ) ;
#19495 = CARTESIAN_POINT ( 'NONE',  ( -1.282825862340494893, -79.73120692033671730, 47.21063963482292536 ) ) ;
#19496 = ORIENTED_EDGE ( 'NONE', *, *, #12077, .F. ) ;
#19497 = ADVANCED_FACE ( 'NONE', ( #9405 ), #12021, .F. ) ;
#19498 = AXIS2_PLACEMENT_3D ( 'NONE', #17996, #22525, #5178 ) ;
#19499 = AXIS2_PLACEMENT_3D ( 'NONE', #27128, #15593, #2070 ) ;
#19500 = CARTESIAN_POINT ( 'NONE',  ( -22.29269750809999806, -94.98812477769999418, -8.065862959109999508 ) ) ;
#19501 = CARTESIAN_POINT ( 'NONE',  ( 13.30722393669999981, -100.8088109309999965, -9.838500919220001251 ) ) ;
#19502 = CARTESIAN_POINT ( 'NONE',  ( -18.69985100839999959, -92.84292036730001030, 22.78328762010000119 ) ) ;
#19503 = ORIENTED_EDGE ( 'NONE', *, *, #10120, .F. ) ;
#19504 = CARTESIAN_POINT ( 'NONE',  ( 10.20338128179359316, -72.72363397105058880, -26.83891338716990660 ) ) ;
#19505 = CARTESIAN_POINT ( 'NONE',  ( -2.597184389209999722, -26.11257328410000156, -24.46312728259999858 ) ) ;
#19506 = VERTEX_POINT ( 'NONE', #20490 ) ;
#19507 = CARTESIAN_POINT ( 'NONE',  ( 8.271554556730841057, -65.04365450819993555, -23.74272564006271580 ) ) ;
#19508 = DIRECTION ( 'NONE',  ( 0.4280775881279951789, 0.000000000000000000, 0.9037419867099893978 ) ) ;
#19509 = DIRECTION ( 'NONE',  ( 1.000000000000000000, 0.000000000000000000, 0.000000000000000000 ) ) ;
#19510 = DIRECTION ( 'NONE',  ( 0.000000000000000000, -1.000000000000000000, 0.000000000000000000 ) ) ;
#19511 = CARTESIAN_POINT ( 'NONE',  ( 0.01062020221023751362, -92.80442066019506342, -30.50000543598749303 ) ) ;
#19512 =( NAMED_UNIT ( * ) PLANE_ANGLE_UNIT ( ) SI_UNIT ( $, .RADIAN. ) );
#19513 = CYLINDRICAL_SURFACE ( 'NONE', #9338, 8.099999999999997868 ) ;
#19514 = AXIS2_PLACEMENT_3D ( 'NONE', #22333, #26854, #9503 ) ;
#19515 = AXIS2_PLACEMENT_3D ( 'NONE', #581, #9426, #22854 ) ;
#19516 = VERTEX_POINT ( 'NONE', #12168 ) ;
#19517 = CARTESIAN_POINT ( 'NONE',  ( 19.52063838700000176, -35.55398684600000081, -8.985157197580001309 ) ) ;
#19518 = ORIENTED_EDGE ( 'NONE', *, *, #23738, .T. ) ;
#19519 = CARTESIAN_POINT ( 'NONE',  ( 20.45950369499999866, -35.93889390129999839, -8.926507745990001297 ) ) ;
#19520 = CARTESIAN_POINT ( 'NONE',  ( -43.16155280139999917, -65.17124718639999514, -0.1954025812290000053 ) ) ;
#19521 = ORIENTED_EDGE ( 'NONE', *, *, #22668, .T. ) ;
#19522 = CARTESIAN_POINT ( 'NONE',  ( 10.53835156000000062, -97.58469692710001198, 16.95036598099999736 ) ) ;
#19523 = EDGE_CURVE ( 'NONE', #2955, #11758, #25315, .T. ) ;
#19524 = DIRECTION ( 'NONE',  ( -0.8775825618903722036, 0.000000000000000000, 0.4794255386042041156 ) ) ;
#19525 = CARTESIAN_POINT ( 'NONE',  ( -27.68682485439999752, -24.80000000000000071, -50.68039294919999804 ) ) ;
#19526 = VERTEX_POINT ( 'NONE', #27647 ) ;
#19527 = CARTESIAN_POINT ( 'NONE',  ( 3.834560414579999854, -92.51556042380001088, 28.49273814280000039 ) ) ;
#19528 = CARTESIAN_POINT ( 'NONE',  ( 7.215414233289999757, -74.50000000000000000, -40.70731707320000226 ) ) ;
#19529 = CARTESIAN_POINT ( 'NONE',  ( 8.529247663789998768, -49.09615641429999755, -22.06548297080000154 ) ) ;
#19530 = CARTESIAN_POINT ( 'NONE',  ( -29.48581804101084458, -92.50630337894774868, 7.800858964961374653 ) ) ;
#19531 = ORIENTED_EDGE ( 'NONE', *, *, #18644, .F. ) ;
#19532 = ADVANCED_FACE ( 'NONE', ( #18459 ), #18751, .T. ) ;
#19533 = CARTESIAN_POINT ( 'NONE',  ( 13.38876965537391150, -100.8061861237962376, -9.910527470073281719 ) ) ;
#19534 = CARTESIAN_POINT ( 'NONE',  ( 24.42476859379999965, -57.44036992910000095, 1.191907835489999901 ) ) ;
#19535 = CARTESIAN_POINT ( 'NONE',  ( 22.86731741559999875, -66.04885972430001573, 11.50583643109999876 ) ) ;
#19536 = CARTESIAN_POINT ( 'NONE',  ( -16.03654356910000089, -101.2023582690000012, 3.165913905190000044 ) ) ;
#19537 = ORIENTED_EDGE ( 'NONE', *, *, #203, .T. ) ;
#19538 = CARTESIAN_POINT ( 'NONE',  ( -39.69269201139999836, -73.74944613229999391, 7.260205543919999727 ) ) ;
#19539 = CIRCLE ( 'NONE', #11636, 30.50381168839999901 ) ;
#19540 = CARTESIAN_POINT ( 'NONE',  ( -38.25000000000000000, -63.17361819573424953, -2.263739386401765863 ) ) ;
#19541 = CARTESIAN_POINT ( 'NONE',  ( 27.18988201479999844, -14.89844555430000028, 49.77074518290000071 ) ) ;
#19542 = CARTESIAN_POINT ( 'NONE',  ( 24.80237074776847805, -93.63284908648850546, -3.743708313212612104 ) ) ;
#19543 = EDGE_LOOP ( 'NONE', ( #19638, #25054, #15886, #4927 ) ) ;
#19544 = AXIS2_PLACEMENT_3D ( 'NONE', #9793, #12115, #18845 ) ;
#19545 = CARTESIAN_POINT ( 'NONE',  ( -0.04280064135489999866, -101.1848541609999899, -15.28253261989999956 ) ) ;
#19546 = CARTESIAN_POINT ( 'NONE',  ( 9.720213298399999147, -61.60483519569999800, -23.97432890940000405 ) ) ;
#19547 = CARTESIAN_POINT ( 'NONE',  ( -12.17277134789999948, -67.87585403689999453, -23.96831300490000061 ) ) ;
#19548 = DIRECTION ( 'NONE',  ( 0.000000000000000000, 1.000000000000000000, 0.000000000000000000 ) ) ;
#19549 = CARTESIAN_POINT ( 'NONE',  ( -11.19118494029999944, -42.26701801490000321, -20.14459658370000028 ) ) ;
#19550 = ORIENTED_EDGE ( 'NONE', *, *, #16424, .T. ) ;
#19551 = CARTESIAN_POINT ( 'NONE',  ( 6.997443162680000661, -100.0994409990000094, 15.73777937049999842 ) ) ;
#19552 = CARTESIAN_POINT ( 'NONE',  ( 14.90889165870000177, -101.1848541609999899, 3.358955891889999990 ) ) ;
#19553 = B_SPLINE_CURVE_WITH_KNOTS ( 'NONE', 3,
 ( #26339, #4038, #10712, #19076 ),
 .UNSPECIFIED., .F., .F.,
 ( 4, 4 ),
 ( -6.855861996759999855, 0.000000000000000000 ),
 .UNSPECIFIED. ) ;
#19554 = ORIENTED_EDGE ( 'NONE', *, *, #2629, .F. ) ;
#19555 = CARTESIAN_POINT ( 'NONE',  ( 8.749807307070001983, -35.48126036069999856, -20.57860491179999940 ) ) ;
#19556 = CARTESIAN_POINT ( 'NONE',  ( 23.70561558430525295, -62.31684853596433271, 10.61541341332936561 ) ) ;
#19557 = DIRECTION ( 'NONE',  ( 0.000000000000000000, 1.000000000000000000, 0.000000000000000000 ) ) ;
#19558 = ORIENTED_EDGE ( 'NONE', *, *, #22780, .F. ) ;
#19559 = AXIS2_PLACEMENT_3D ( 'NONE', #5412, #3101, #23191 ) ;
#19560 = CARTESIAN_POINT ( 'NONE',  ( 1.834176908449999921, -92.53610956480000027, -29.48862716980000087 ) ) ;
#19561 = AXIS2_PLACEMENT_3D ( 'NONE', #18666, #20993, #3357 ) ;
#19562 = EDGE_CURVE ( 'NONE', #28257, #16909, #20937, .T. ) ;
#19563 = CIRCLE ( 'NONE', #24700, 55.67692378859999991 ) ;
#19564 = CARTESIAN_POINT ( 'NONE',  ( -7.627568735119999666, -74.00000000000000000, -38.62788659690000515 ) ) ;
#19565 = CARTESIAN_POINT ( 'NONE',  ( -6.741828608569999659, -101.3256027139999986, 14.40730483740000167 ) ) ;
#19566 = EDGE_LOOP ( 'NONE', ( #6711, #11722, #17444, #14091 ) ) ;
#19567 = LINE ( 'NONE', #17390, #9161 ) ;
#19568 = CARTESIAN_POINT ( 'NONE',  ( -12.47973093158265634, -101.2145573445022251, -10.54238648815402257 ) ) ;
#19569 = ORIENTED_EDGE ( 'NONE', *, *, #5597, .F. ) ;
#19570 = CARTESIAN_POINT ( 'NONE',  ( 8.954566937750000122, -35.98146629219999681, -20.48934717840000275 ) ) ;
#19571 = ADVANCED_FACE ( 'NONE', ( #3166 ), #1585, .T. ) ;
#19572 = CARTESIAN_POINT ( 'NONE',  ( 24.59449300740000055, -93.85307999839999127, -3.931206936640000205 ) ) ;
#19573 = ADVANCED_FACE ( 'NONE', ( #16107 ), #15666, .T. ) ;
#19574 = CARTESIAN_POINT ( 'NONE',  ( -0.9146590393339999459, -101.2995922080000071, -15.89573683670000115 ) ) ;
#19575 = CARTESIAN_POINT ( 'NONE',  ( 22.28013210319999970, -18.61865660339999806, 1.245317927350000131 ) ) ;
#19576 = FACE_OUTER_BOUND ( 'NONE', #4337, .T. ) ;
#19577 = CARTESIAN_POINT ( 'NONE',  ( 24.33707037739999990, -62.95235822580000473, -9.864745197619999573 ) ) ;
#19578 = ORIENTED_EDGE ( 'NONE', *, *, #24680, .T. ) ;
#19579 = CARTESIAN_POINT ( 'NONE',  ( 19.57417645929999850, -18.50000000000000000, -7.622693574120000370 ) ) ;
#19580 = LINE ( 'NONE', #17547, #3452 ) ;
#19581 = CARTESIAN_POINT ( 'NONE',  ( -4.500000000000000000, -11.00000000000000000, -31.00000000000000000 ) ) ;
#19582 = CARTESIAN_POINT ( 'NONE',  ( -18.48910831820316858, -19.46665351423196455, 12.47298576395390057 ) ) ;
#19583 = CARTESIAN_POINT ( 'NONE',  ( 23.54313657600000198, -94.98812477599999227, -6.784142512209999865 ) ) ;
#19584 = DIRECTION ( 'NONE',  ( 0.000000000000000000, -1.000000000000000000, 0.000000000000000000 ) ) ;
#19585 = CONICAL_SURFACE ( 'NONE', #15357, 55.67692378859999280, 1.047197551199999799 ) ;
#19586 = ORIENTED_EDGE ( 'NONE', *, *, #13312, .T. ) ;
#19587 = CIRCLE ( 'NONE', #12585, 55.67692378859999991 ) ;
#19588 = CARTESIAN_POINT ( 'NONE',  ( 8.901252876769998323, -18.87168143470000103, -18.93437212940000336 ) ) ;
#19589 = VECTOR ( 'NONE', #6853, 1000.000000000000000 ) ;
#19590 = CARTESIAN_POINT ( 'NONE',  ( 22.83075791639999608, -36.54217832150000334, -9.915197167589999694 ) ) ;
#19591 = B_SPLINE_CURVE_WITH_KNOTS ( 'NONE', 3,
 ( #11234, #20141, #17961, #2095, #351, #22046, #19837, #18110, #28717, #18254 ),
 .UNSPECIFIED., .F., .F.,
 ( 4, 2, 2, 2, 4 ),
 ( 0.000000000000000000, 0.2500000000000006106, 0.5000000000000012212, 0.7500000000000017764, 1.000000000000000000 ),
 .UNSPECIFIED. ) ;
#19592 = CARTESIAN_POINT ( 'NONE',  ( -0.6973805902349998753, -64.04267428580000399, -24.66993619630000012 ) ) ;
#19593 = CARTESIAN_POINT ( 'NONE',  ( -23.55553543979999986, -94.54719310899999130, -3.773174522320000168 ) ) ;
#19594 = CARTESIAN_POINT ( 'NONE',  ( 50.00000000000000000, -11.00000000000000000, -4.500000000000000000 ) ) ;
#19595 = CARTESIAN_POINT ( 'NONE',  ( -38.55000000000000426, -65.14977478849999670, 2.857883832489999776 ) ) ;
#19596 = EDGE_CURVE ( 'NONE', #19426, #24400, #23901, .T. ) ;
#19597 = ADVANCED_FACE ( 'NONE', ( #15050 ), #19303, .F. ) ;
#19598 = CARTESIAN_POINT ( 'NONE',  ( 15.16019776770000149, -100.8023006570000035, 4.366346884840000442 ) ) ;
#19599 = ORIENTED_EDGE ( 'NONE', *, *, #7173, .F. ) ;
#19600 = CARTESIAN_POINT ( 'NONE',  ( 14.34373124439999891, -92.50000000000000000, 26.25602392650000283 ) ) ;
#19601 = FACE_OUTER_BOUND ( 'NONE', #15801, .T. ) ;
#19602 = ORIENTED_EDGE ( 'NONE', *, *, #13863, .T. ) ;
#19603 = AXIS2_PLACEMENT_3D ( 'NONE', #17949, #11514, #19972 ) ;
#19604 = DIRECTION ( 'NONE',  ( 0.000000000000000000, -1.000000000000000000, 0.000000000000000000 ) ) ;
#19605 = AXIS2_PLACEMENT_3D ( 'NONE', #15799, #15650, #15200 ) ;
#19606 = EDGE_CURVE ( 'NONE', #19954, #13987, #3892, .T. ) ;
#19607 = B_SPLINE_CURVE_WITH_KNOTS ( 'NONE', 5,
 ( #23968, #28194, #26885, #24403, #15937, #13762 ),
 .UNSPECIFIED., .F., .F.,
 ( 6, 6 ),
 ( 0.000000000000000000, 1.000000000000000000 ),
 .UNSPECIFIED. ) ;
#19608 = CARTESIAN_POINT ( 'NONE',  ( 19.90536779560000014, -32.73235193850000257, 10.48824559260000022 ) ) ;
#19609 = CARTESIAN_POINT ( 'NONE',  ( -22.13744763498781509, -74.09767108955308856, -32.45678264336510210 ) ) ;
#19610 = CARTESIAN_POINT ( 'NONE',  ( 22.25879350760000008, -18.50000000000000000, 8.634216631190000157 ) ) ;
#19611 = DIRECTION ( 'NONE',  ( 0.000000000000000000, -1.000000000000000000, 0.000000000000000000 ) ) ;
#19612 = DIRECTION ( 'NONE',  ( 0.000000000000000000, 1.000000000000000000, 0.000000000000000000 ) ) ;
#19613 = ORIENTED_EDGE ( 'NONE', *, *, #1371, .T. ) ;
#19614 = CARTESIAN_POINT ( 'NONE',  ( 40.65853658540000026, -84.50000000000000000, 6.717799458580000049 ) ) ;
#19615 = CARTESIAN_POINT ( 'NONE',  ( -12.31038953760000076, -100.5717442099999914, -10.73123778619999946 ) ) ;
#19616 = CARTESIAN_POINT ( 'NONE',  ( -7.155584660037434652, -73.50000006902133975, 38.82824093549695021 ) ) ;
#19617 = DIRECTION ( 'NONE',  ( 0.4794255386042041156, 0.000000000000000000, 0.8775825618903720926 ) ) ;
#19618 = VERTEX_POINT ( 'NONE', #16689 ) ;
#19619 = EDGE_CURVE ( 'NONE', #20652, #20846, #27913, .T. ) ;
#19620 = CARTESIAN_POINT ( 'NONE',  ( -1.120268941615737646, -101.5019029709670377, -16.07166635754587958 ) ) ;
#19621 = CARTESIAN_POINT ( 'NONE',  ( -32.35609092660000385, -74.05570514439999386, -22.11293405780000043 ) ) ;
#19622 = ORIENTED_EDGE ( 'NONE', *, *, #23587, .F. ) ;
#19623 = AXIS2_PLACEMENT_3D ( 'NONE', #18683, #23329, #2954 ) ;
#19624 = FACE_OUTER_BOUND ( 'NONE', #5397, .T. ) ;
#19625 = CARTESIAN_POINT ( 'NONE',  ( -5.145393133449999823, -99.91547912669999221, 17.23229113919999733 ) ) ;
#19626 = CARTESIAN_POINT ( 'NONE',  ( 12.02340861999999966, -92.49786325860000602, 27.16485054520000020 ) ) ;
#19627 = ORIENTED_EDGE ( 'NONE', *, *, #24623, .T. ) ;
#19628 = CARTESIAN_POINT ( 'NONE',  ( -16.59215593114620191, -93.55106866339940552, -21.49707546704379624 ) ) ;
#19629 = EDGE_LOOP ( 'NONE', ( #26047, #16879, #1705, #2297, #11350, #17858, #15422 ) ) ;
#19630 = CARTESIAN_POINT ( 'NONE',  ( 22.25602728220000159, -57.44036991819999827, 10.13208872880000122 ) ) ;
#19631 = CARTESIAN_POINT ( 'NONE',  ( 46.15163212009999683, -73.78135298099999773, -3.953675005160000477 ) ) ;
#19632 = ORIENTED_EDGE ( 'NONE', *, *, #9769, .T. ) ;
#19633 = CARTESIAN_POINT ( 'NONE',  ( -41.75000000000064659, -65.66839995185510759, 1.503614136383694122 ) ) ;
#19634 = CARTESIAN_POINT ( 'NONE',  ( 22.97877291129812605, -37.68584072819992770, -9.393614098449470262 ) ) ;
#19635 = CARTESIAN_POINT ( 'NONE',  ( 9.444779992160000859, -36.00000000019999646, -20.77909504619999836 ) ) ;
#19636 = CARTESIAN_POINT ( 'NONE',  ( -23.49132538869999820, -93.00000902169999506, -19.26888042029999681 ) ) ;
#19637 = CARTESIAN_POINT ( 'NONE',  ( -1.938080129439999855, -18.50000000000000000, -21.30966978559999703 ) ) ;
#19638 = ORIENTED_EDGE ( 'NONE', *, *, #11507, .F. ) ;
#19639 = CARTESIAN_POINT ( 'NONE',  ( -6.035167374697340215, -101.5620304352239600, 14.88825629219373603 ) ) ;
#19640 = CARTESIAN_POINT ( 'NONE',  ( 12.82869130110000100, -100.7833805400000102, -9.414914349620000067 ) ) ;
#19641 = CARTESIAN_POINT ( 'NONE',  ( -19.01557598040000130, -92.50000000000000000, 22.91712379000000155 ) ) ;
#19642 = CARTESIAN_POINT ( 'NONE',  ( -5.574503815731460143, -98.30555344503575554, -19.38668258828887048 ) ) ;
#19643 = CARTESIAN_POINT ( 'NONE',  ( 10.47579678358301436, -72.64479057567018572, -26.80810721546713893 ) ) ;
#19644 = CARTESIAN_POINT ( 'NONE',  ( 4.824585175810001050E-12, -111.0000000000000000, 3.574029960870000059E-12 ) ) ;
#19645 = VERTEX_POINT ( 'NONE', #12854 ) ;
#19646 = DIRECTION ( 'NONE',  ( -0.4822503909160886226, 0.000000000000000000, 0.8760334242831604445 ) ) ;
#19647 = ADVANCED_FACE ( 'NONE', ( #23401 ), #3016, .T. ) ;
#19648 = CARTESIAN_POINT ( 'NONE',  ( 9.464545271430450768, -57.41957453194978456, -23.23309258220142226 ) ) ;
#19649 = DIRECTION ( 'NONE',  ( -6.123031769110000420E-17, 0.000000000000000000, 1.000000000000000000 ) ) ;
#19650 = CARTESIAN_POINT ( 'NONE',  ( -38.25000000000000000, -65.31510159580000163, 2.337827133090000231 ) ) ;
#19651 = CARTESIAN_POINT ( 'NONE',  ( 0.07669151669536446170, -92.87422005960708304, -30.49990716389019241 ) ) ;
#19652 = EDGE_CURVE ( 'NONE', #20968, #21377, #23018, .T. ) ;
#19653 = TOROIDAL_SURFACE ( 'NONE', #19209, 29.91857981989999971, 10.00000000000000000 ) ;
#19654 = EDGE_CURVE ( 'NONE', #26053, #10170, #19272, .T. ) ;
#19655 = AXIS2_PLACEMENT_3D ( 'NONE', #11038, #326, #18076 ) ;
#19656 = LINE ( 'NONE', #2930, #10116 ) ;
#19657 = EDGE_CURVE ( 'NONE', #22334, #28503, #24855, .T. ) ;
#19658 = ORIENTED_EDGE ( 'NONE', *, *, #15779, .T. ) ;
#19659 = CARTESIAN_POINT ( 'NONE',  ( 19.45476613419999978, -98.30614355080000166, -0.3720397164350000563 ) ) ;
#19660 = ORIENTED_EDGE ( 'NONE', *, *, #7699, .T. ) ;
#19661 = CARTESIAN_POINT ( 'NONE',  ( 21.48608955399999942, -36.92296609210000469, -7.459959442930000684 ) ) ;
#19662 = CARTESIAN_POINT ( 'NONE',  ( 9.444187806723459033, -35.99901531098080909, -19.97576011151723563 ) ) ;
#19663 = EDGE_LOOP ( 'NONE', ( #16006, #15026 ) ) ;
#19664 = DIRECTION ( 'NONE',  ( 0.000000000000000000, 1.000000000000000000, 0.000000000000000000 ) ) ;
#19665 = DIRECTION ( 'NONE',  ( 0.4794255386042042266, 0.000000000000000000, 0.8775825618903720926 ) ) ;
#19666 = PRODUCT_DEFINITION_SHAPE ( 'NONE', 'NONE',  #10742 ) ;
#19667 = CARTESIAN_POINT ( 'NONE',  ( -13.09441259049999928, -92.84550468730000716, -23.96917219330000037 ) ) ;
#19668 = CARTESIAN_POINT ( 'NONE',  ( -8.799882794190001079, -96.11313168749998681, -20.83764462659999950 ) ) ;
#19669 = CIRCLE ( 'NONE', #4804, 55.50192378860000275 ) ;
#19670 = CARTESIAN_POINT ( 'NONE',  ( 7.653117467020000397, -101.1929016639999901, 13.21760603179999904 ) ) ;
#19671 = DIRECTION ( 'NONE',  ( 0.000000000000000000, 1.000000000000000000, 0.000000000000000000 ) ) ;
#19672 = CARTESIAN_POINT ( 'NONE',  ( 7.362282719720000479, -57.47832541620000057, -22.17287314020000011 ) ) ;
#19673 = CARTESIAN_POINT ( 'NONE',  ( -29.60150005379874827, -92.56772982772959324, 7.348804374798064920 ) ) ;
#19674 = CARTESIAN_POINT ( 'NONE',  ( -40.34155842951303583, -65.69467928435145154, 2.235060801196294467 ) ) ;
#19675 = ORIENTED_EDGE ( 'NONE', *, *, #9736, .T. ) ;
#19676 = FACE_OUTER_BOUND ( 'NONE', #25545, .T. ) ;
#19677 = CARTESIAN_POINT ( 'NONE',  ( 26.61465604159999998, -68.28989644159999273, 0.1578853838729999959 ) ) ;
#19678 = CARTESIAN_POINT ( 'NONE',  ( 25.93066785690000131, -70.16663891479998938, 10.87636646910000060 ) ) ;
#19679 = CARTESIAN_POINT ( 'NONE',  ( 38.71640881029999548, -73.50000064450000536, 7.135467304789999687 ) ) ;
#19680 = ORIENTED_EDGE ( 'NONE', *, *, #14950, .T. ) ;
#19681 = CIRCLE ( 'NONE', #7149, 0.3500000000000003664 ) ;
#19682 = CARTESIAN_POINT ( 'NONE',  ( 4.500000000000000000, -13.00000000000000000, -31.00000000000000000 ) ) ;
#19683 = CARTESIAN_POINT ( 'NONE',  ( -15.90615684040000133, -92.85195831059998284, 23.95936788750000090 ) ) ;
#19684 = CARTESIAN_POINT ( 'NONE',  ( 23.70295537799999863, -94.59276292389999696, -2.111841813949999924 ) ) ;
#19685 = ORIENTED_EDGE ( 'NONE', *, *, #10407, .T. ) ;
#19686 = CARTESIAN_POINT ( 'NONE',  ( 27.92725156619999893, -70.60688442979999024, 1.994915591920000342 ) ) ;
#19687 = CARTESIAN_POINT ( 'NONE',  ( 0.6048686566590000258, -100.8088109309999965, -16.53821160670000268 ) ) ;
#19688 = CARTESIAN_POINT ( 'NONE',  ( 8.600016245219999078, -57.45905972560000663, -22.33353789330000083 ) ) ;
#19689 = CARTESIAN_POINT ( 'NONE',  ( -12.22512305319999903, -68.97169036700000788, -24.44138895879999751 ) ) ;
#19690 = CARTESIAN_POINT ( 'NONE',  ( 22.25602933960000129, -57.44036955189999816, 10.13208958120000069 ) ) ;
#19691 = CARTESIAN_POINT ( 'NONE',  ( 22.85528114059999893, -62.13923587570000251, -7.268368518939999134 ) ) ;
#19692 = ORIENTED_EDGE ( 'NONE', *, *, #28767, .F. ) ;
#19693 = EDGE_CURVE ( 'NONE', #8389, #20314, #28551, .T. ) ;
#19694 = CARTESIAN_POINT ( 'NONE',  ( -36.50000000000000000, -69.00000000000000000, 0.000000000000000000 ) ) ;
#19695 = FACE_OUTER_BOUND ( 'NONE', #15775, .T. ) ;
#19696 = AXIS2_PLACEMENT_3D ( 'NONE', #6280, #15851, #24904 ) ;
#19697 = EDGE_CURVE ( 'NONE', #28649, #2030, #5769, .T. ) ;
#19698 = EDGE_CURVE ( 'NONE', #14463, #27919, #10402, .T. ) ;
#19699 = SHAPE_REPRESENTATION ( 'Mechanical Shaft Face Seal', ( #26433 ), #5053 ) ;
#19700 = ORIENTED_EDGE ( 'NONE', *, *, #8922, .F. ) ;
#19701 = LINE ( 'NONE', #4697, #18366 ) ;
#19702 = CARTESIAN_POINT ( 'NONE',  ( 23.48715812726448249, -61.18336516922612844, 10.53353075793953053 ) ) ;
#19703 = CARTESIAN_POINT ( 'NONE',  ( -5.679728865570000451, -96.65227117000000590, 20.49066625190000224 ) ) ;
#19704 = VERTEX_POINT ( 'NONE', #24249 ) ;
#19705 = CIRCLE ( 'NONE', #13170, 7.250000000000000000 ) ;
#19706 = CARTESIAN_POINT ( 'NONE',  ( 6.195449712719999447, -93.01125874769999768, -25.86806793289999717 ) ) ;
#19707 = CARTESIAN_POINT ( 'NONE',  ( 6.825713544544626643, -101.5409490182170487, 14.56261500540370868 ) ) ;
#19708 = FACE_OUTER_BOUND ( 'NONE', #9750, .T. ) ;
#19709 = ORIENTED_EDGE ( 'NONE', *, *, #11460, .F. ) ;
#19710 = CARTESIAN_POINT ( 'NONE',  ( -13.02449431219020681, -100.2392017796373977, -11.09622749139835918 ) ) ;
#19711 = EDGE_LOOP ( 'NONE', ( #5127, #15468, #1449, #3222 ) ) ;
#19712 = CARTESIAN_POINT ( 'NONE',  ( 8.927245643350000037, -35.93968828110000402, -20.45978054029999882 ) ) ;
#19713 = CARTESIAN_POINT ( 'NONE',  ( -40.00000000000000000, -77.00000000000000000, 0.000000000000000000 ) ) ;
#19714 = CARTESIAN_POINT ( 'NONE',  ( -1.449832362199999780, -100.8733988930000010, -15.65780151839999945 ) ) ;
#19715 = AXIS2_PLACEMENT_3D ( 'NONE', #7887, #10045, #18830 ) ;
#19716 = CARTESIAN_POINT ( 'NONE',  ( 21.27670944740000181, -18.50000000000000000, 0.7959958381299999663 ) ) ;
#19717 = CARTESIAN_POINT ( 'NONE',  ( -7.627567457969999687, -74.00000025069999765, 38.62788781560000473 ) ) ;
#19718 = CIRCLE ( 'NONE', #20686, 23.79684788999999867 ) ;
#19719 = CARTESIAN_POINT ( 'NONE',  ( -20.85581432803203938, -92.82529299097140552, -22.25499991766502106 ) ) ;
#19720 = ORIENTED_EDGE ( 'NONE', *, *, #10014, .F. ) ;
#19721 = CARTESIAN_POINT ( 'NONE',  ( -15.33274302080000062, -101.3256032150000010, 4.234343774090000068 ) ) ;
#19722 = DIRECTION ( 'NONE',  ( 0.000000000000000000, 1.000000000000000000, 0.000000000000000000 ) ) ;
#19723 = CARTESIAN_POINT ( 'NONE',  ( -36.72197963276312294, -65.10668761694336126, -0.09248738124049776799 ) ) ;
#19724 = CARTESIAN_POINT ( 'NONE',  ( 36.70830950850000107, -75.00000000000000000, -14.75000000000000000 ) ) ;
#19725 = CARTESIAN_POINT ( 'NONE',  ( -12.17278359089999995, -67.87586094739999965, -23.96830084060000132 ) ) ;
#19726 = AXIS2_PLACEMENT_3D ( 'NONE', #2595, #568, #22399 ) ;
#19727 = CARTESIAN_POINT ( 'NONE',  ( 24.59924222825820905, -93.48480241513080102, 11.95794408568441547 ) ) ;
#19728 = ORIENTED_EDGE ( 'NONE', *, *, #21481, .T. ) ;
#19729 = EDGE_CURVE ( 'NONE', #3141, #212, #14173, .T. ) ;
#19730 = CARTESIAN_POINT ( 'NONE',  ( 8.311993592450001245, -18.50000000000000000, -19.17432171929999996 ) ) ;
#19731 = EDGE_CURVE ( 'NONE', #25778, #24455, #19580, .T. ) ;
#19732 = ORIENTED_EDGE ( 'NONE', *, *, #10755, .F. ) ;
#19733 = CARTESIAN_POINT ( 'NONE',  ( -2.496526366579999934, -62.53529079479999808, -25.29179931070000009 ) ) ;
#19734 = VECTOR ( 'NONE', #6496, 1000.000000000000000 ) ;
#19735 = CARTESIAN_POINT ( 'NONE',  ( 20.33566493080000015, -36.00000000000000000, -9.885503730140001721 ) ) ;
#19736 = CARTESIAN_POINT ( 'NONE',  ( -20.48522561129999886, -53.77454410920000072, 14.80553289520000071 ) ) ;
#19737 = CARTESIAN_POINT ( 'NONE',  ( 0.000000000000000000, -33.79999999999999716, 0.000000000000000000 ) ) ;
#19738 = VERTEX_POINT ( 'NONE', #4286 ) ;
#19739 = CARTESIAN_POINT ( 'NONE',  ( -21.63521261336145685, -95.36087494562657696, -8.478298660255941144 ) ) ;
#19740 = CARTESIAN_POINT ( 'NONE',  ( 7.318371247189999984, -73.93831524339999817, -38.68350846249999364 ) ) ;
#19741 = ORIENTED_EDGE ( 'NONE', *, *, #5975, .F. ) ;
#19742 = CIRCLE ( 'NONE', #23490, 11.00000000000000000 ) ;
#19743 = CARTESIAN_POINT ( 'NONE',  ( 8.195672531370084002, -37.94341444778289940, -21.63145225707751251 ) ) ;
#19744 = CARTESIAN_POINT ( 'NONE',  ( -41.54999999999999716, -65.00000000000000000, -2.684678751729999480 ) ) ;
#19745 = CONICAL_SURFACE ( 'NONE', #27205, 57.74999999999999289, 1.152571997220000144 ) ;
#19746 = CARTESIAN_POINT ( 'NONE',  ( -9.864287931150000688, -18.50000000000000000, -19.01841465109999874 ) ) ;
#19747 = FACE_BOUND ( 'NONE', #12876, .T. ) ;
#19748 = CARTESIAN_POINT ( 'NONE',  ( -15.07824091630000041, -101.1292389600000092, 3.618410085480000316 ) ) ;
#19749 = CARTESIAN_POINT ( 'NONE',  ( -41.70526651914970984, -65.09475709727961146, 2.825938370821126089 ) ) ;
#19750 = CARTESIAN_POINT ( 'NONE',  ( -17.60046531049869145, -95.43638356959962721, 14.34842257852166192 ) ) ;
#19751 = ORIENTED_EDGE ( 'NONE', *, *, #12896, .F. ) ;
#19752 = VECTOR ( 'NONE', #21420, 1000.000000000000114 ) ;
#19753 = LINE ( 'NONE', #28499, #25087 ) ;
#19754 = CARTESIAN_POINT ( 'NONE',  ( -12.21977202059999890, -101.0678230150000019, -10.05267167180000065 ) ) ;
#19755 = CARTESIAN_POINT ( 'NONE',  ( 6.888451955769999913, -99.53431386179998697, 15.99365555089999802 ) ) ;
#19756 = CARTESIAN_POINT ( 'NONE',  ( 23.70177636041242764, -64.50388029674192580, -7.622970390447100009 ) ) ;
#19757 = VERTEX_POINT ( 'NONE', #26875 ) ;
#19758 = ADVANCED_FACE ( 'NONE', ( #11097 ), #21919, .T. ) ;
#19759 = FACE_OUTER_BOUND ( 'NONE', #931, .T. ) ;
#19760 = CARTESIAN_POINT ( 'NONE',  ( -32.17865685019999233, -74.02983596709999858, -21.95421844790000065 ) ) ;
#19761 = CARTESIAN_POINT ( 'NONE',  ( 0.000000000000000000, -56.78056608349999834, 0.000000000000000000 ) ) ;
#19762 = ORIENTED_EDGE ( 'NONE', *, *, #7877, .T. ) ;
#19763 = EDGE_CURVE ( 'NONE', #19516, #5855, #19718, .T. ) ;
#19764 = VECTOR ( 'NONE', #25498, 1000.000000000000000 ) ;
#19765 = B_SPLINE_CURVE_WITH_KNOTS ( 'NONE', 5,
 ( #8149, #17760, #11010, #24456, #8565, #15397, #13366, #26500, #22269 ),
 .UNSPECIFIED., .F., .F.,
 ( 6, 3, 6 ),
 ( 0.000000000000000000, 0.5000000000000000000, 1.000000000000000000 ),
 .UNSPECIFIED. ) ;
#19766 = SPHERICAL_SURFACE ( 'NONE', #11096, 2.000000000000000000 ) ;
#19767 = CARTESIAN_POINT ( 'NONE',  ( -0.8216735279219999910, -65.07443093669999712, -25.13632616349999793 ) ) ;
#19768 = VERTEX_POINT ( 'NONE', #6915 ) ;
#19769 = DIRECTION ( 'NONE',  ( 0.000000000000000000, 1.000000000000000000, 0.000000000000000000 ) ) ;
#19770 = ORIENTED_EDGE ( 'NONE', *, *, #9274, .F. ) ;
#19771 = CARTESIAN_POINT ( 'NONE',  ( 23.99168239580000161, -92.99570708089999016, 12.03585351179999918 ) ) ;
#19772 = CARTESIAN_POINT ( 'NONE',  ( 36.25000000000000000, -79.00000000000000000, 2.314797894279999601E-15 ) ) ;
#19773 = VERTEX_POINT ( 'NONE', #24689 ) ;
#19774 = LINE ( 'NONE', #28523, #8490 ) ;
#19775 = FACE_OUTER_BOUND ( 'NONE', #175, .T. ) ;
#19776 = EDGE_CURVE ( 'NONE', #2148, #9200, #7242, .T. ) ;
#19777 = CARTESIAN_POINT ( 'NONE',  ( 8.913589957130000130, -36.23936169889999803, -21.16767038869999951 ) ) ;
#19778 = CARTESIAN_POINT ( 'NONE',  ( -18.94669760780000090, -93.16461275559998967, -21.17240009389999855 ) ) ;
#19779 = CARTESIAN_POINT ( 'NONE',  ( 26.65586303345174812, -70.93575951088651266, 10.69912789994289959 ) ) ;
#19780 = VERTEX_POINT ( 'NONE', #10667 ) ;
#19781 = CARTESIAN_POINT ( 'NONE',  ( 36.22844186549999534, -74.00000000000000000, -13.75000000000000000 ) ) ;
#19782 = CARTESIAN_POINT ( 'NONE',  ( 12.68262372769999935, -101.2927714249999980, -9.844469503889998307 ) ) ;
#19783 = FACE_OUTER_BOUND ( 'NONE', #4816, .T. ) ;
#19784 = CARTESIAN_POINT ( 'NONE',  ( -11.73664924843507507, -94.54719627006902272, -20.76900799921979512 ) ) ;
#19785 = CLOSED_SHELL ( 'NONE', ( #2277, #19378, #22113, #2091, #7294, #24582, #25580, #8158, #605, #12933, #4065, #10499, #5779, #9907, #20583, #24984, #8512, #20706 ) ) ;
#19786 = DIRECTION ( 'NONE',  ( 0.4794255386042036715, 0.000000000000000000, 0.8775825618903724257 ) ) ;
#19787 = CARTESIAN_POINT ( 'NONE',  ( 26.72663706610000034, -37.96100227850000408, 48.92278099219999632 ) ) ;
#19788 = PLANE ( 'NONE',  #28466 ) ;
#19789 = ORIENTED_EDGE ( 'NONE', *, *, #5008, .F. ) ;
#19790 = EDGE_CURVE ( 'NONE', #8453, #25599, #28741, .T. ) ;
#19792 = EDGE_CURVE ( 'NONE', #20678, #14123, #22518, .T. ) ;
#19791 = CARTESIAN_POINT ( 'NONE',  ( -38.25000000000000000, -63.07912966450000880, 2.684678751729999480 ) ) ;
#19793 = CARTESIAN_POINT ( 'NONE',  ( 7.362282589680580358, -57.47832521685436546, -22.17287418770180452 ) ) ;
#19794 = DIRECTION ( 'NONE',  ( 0.8775825618903722036, 0.000000000000000000, -0.4794255386042041156 ) ) ;
#19795 = CARTESIAN_POINT ( 'NONE',  ( -38.25000000000000000, -65.19264941160000149, 2.595760183519999931 ) ) ;
#19796 = CARTESIAN_POINT ( 'NONE',  ( -0.4792089288136882064, -92.59055325466957242, -30.49623656381675119 ) ) ;
#19797 = AXIS2_PLACEMENT_3D ( 'NONE', #28327, #17258, #6180 ) ;
#19798 = DIRECTION ( 'NONE',  ( 0.000000000000000000, 1.000000000000000000, 0.000000000000000000 ) ) ;
#19799 = VERTEX_POINT ( 'NONE', #4431 ) ;
#19800 = CARTESIAN_POINT ( 'NONE',  ( -11.32307664120000013, -92.50000000000000000, 9.421136869679999748 ) ) ;
#19801 = CARTESIAN_POINT ( 'NONE',  ( 25.81706525379999917, -37.08699221940000257, 47.25782095779999992 ) ) ;
#19802 = ORIENTED_EDGE ( 'NONE', *, *, #23998, .F. ) ;
#19803 = CARTESIAN_POINT ( 'NONE',  ( -11.95046964750000029, -49.86907377909999894, 20.00125202210000097 ) ) ;
#19804 = CARTESIAN_POINT ( 'NONE',  ( 9.227003638719999401, -35.93081093159999995, -19.61343128729999918 ) ) ;
#19805 = ORIENTED_EDGE ( 'NONE', *, *, #15749, .T. ) ;
#19806 = CARTESIAN_POINT ( 'NONE',  ( 15.04572477429999822, -95.61314413700000614, 17.10854321069999884 ) ) ;
#19807 = EDGE_CURVE ( 'NONE', #1569, #24813, #15044, .T. ) ;
#19808 = CARTESIAN_POINT ( 'NONE',  ( -3.331535842216653887, -67.92908815540094736, -27.51829522574995579 ) ) ;
#19809 = ORIENTED_EDGE ( 'NONE', *, *, #10146, .F. ) ;
#19810 = CARTESIAN_POINT ( 'NONE',  ( -8.929965488379998817, -95.98352844290000974, -20.19091974539999867 ) ) ;
#19811 = DIRECTION ( 'NONE',  ( 0.000000000000000000, 1.000000000000000000, 0.000000000000000000 ) ) ;
#19812 = CARTESIAN_POINT ( 'NONE',  ( 9.464546293550000655, -57.41957467990000197, -23.23309162749999857 ) ) ;
#19813 = CARTESIAN_POINT ( 'NONE',  ( -29.52744277902158032, -92.52249206703173456, 7.640708811399515632 ) ) ;
#19814 = CARTESIAN_POINT ( 'NONE',  ( 11.79516146510218455, -98.68740020586984940, -15.74753716043547591 ) ) ;
#19815 = VERTEX_POINT ( 'NONE', #22285 ) ;
#19816 = CARTESIAN_POINT ( 'NONE',  ( 7.292763125380000488, -92.50000467790000869, -29.01615471190000051 ) ) ;
#19817 = DIRECTION ( 'NONE',  ( 0.000000000000000000, 1.000000000000000000, 0.000000000000000000 ) ) ;
#19818 = CARTESIAN_POINT ( 'NONE',  ( -14.01337423630000067, -80.50000000000000000, 36.66316738249999929 ) ) ;
#19819 = CARTESIAN_POINT ( 'NONE',  ( 9.396869795909999823, -94.80026829410000744, -22.54657044670000232 ) ) ;
#19820 = ORIENTED_EDGE ( 'NONE', *, *, #1193, .T. ) ;
#19821 =( REPRESENTATION_RELATIONSHIP ('NONE','NONE', #26008, #24690 ) REPRESENTATION_RELATIONSHIP_WITH_TRANSFORMATION ( #18655 )SHAPE_REPRESENTATION_RELATIONSHIP( ) );
#19822 = EDGE_CURVE ( 'NONE', #16038, #16955, #10848, .T. ) ;
#19823 = CARTESIAN_POINT ( 'NONE',  ( -38.71641004229999794, -73.65707963269998970, 7.135467526410000261 ) ) ;
#19824 = CARTESIAN_POINT ( 'NONE',  ( -13.52403886319999948, -92.76842119879999871, 27.15914155860000179 ) ) ;
#19825 = DIRECTION ( 'NONE',  ( 0.000000000000000000, 1.000000000000000000, 0.000000000000000000 ) ) ;
#19826 = EDGE_LOOP ( 'NONE', ( #4960, #25518, #24553, #6960 ) ) ;
#19827 = CARTESIAN_POINT ( 'NONE',  ( 28.55874257110000158, -72.70510787919999984, 2.003337190579999927 ) ) ;
#19828 = CARTESIAN_POINT ( 'NONE',  ( 1.014918664000000081, -100.4731125450000064, -16.17028307509999863 ) ) ;
#19829 = CARTESIAN_POINT ( 'NONE',  ( 0.000000000000000000, -2.000000000000000000, 0.000000000000000000 ) ) ;
#19830 = CARTESIAN_POINT ( 'NONE',  ( -12.08584241179999985, -69.49854687080001270, -25.11440336740000134 ) ) ;
#19831 = CARTESIAN_POINT ( 'NONE',  ( -11.62511810790000055, -42.27294335669999725, -19.65139164230000191 ) ) ;
#19832 = ORIENTED_EDGE ( 'NONE', *, *, #6406, .F. ) ;
#19833 = CARTESIAN_POINT ( 'NONE',  ( 22.17287391930145546, -57.47832537024360988, -7.362282751270468495 ) ) ;
#19834 = DIRECTION ( 'NONE',  ( 0.4794255386042041156, 0.000000000000000000, 0.8775825618903722036 ) ) ;
#19835 = VERTEX_POINT ( 'NONE', #20539 ) ;
#19836 = CARTESIAN_POINT ( 'NONE',  ( 0.000000000000000000, -33.49689110869999809, 0.000000000000000000 ) ) ;
#19837 = CARTESIAN_POINT ( 'NONE',  ( 15.62053000518932855, -101.3051320416605563, 2.831994469588900110 ) ) ;
#19838 = DIRECTION ( 'NONE',  ( 0.000000000000000000, -1.000000000000000000, 0.000000000000000000 ) ) ;
#19839 = CARTESIAN_POINT ( 'NONE',  ( -18.00123211990801764, -98.93440139940453548, 5.015526314420251985 ) ) ;
#19840 = B_SPLINE_SURFACE_WITH_KNOTS ( 'NONE', 2, 5, ( 
 ( #21397, #23722, #27697, #21538, #27961, #7862 ),
 ( #28227, #1594, #9889, #28097, #8261, #3902 ),
 ( #23310, #3492, #16603, #3626, #1053, #21261 ) ),
 .UNSPECIFIED., .F., .F., .F.,
 ( 3, 3 ),
 ( 6, 6 ),
 ( 6.132304667409999688, 7.821587791749999852 ),
 ( 0.000000000000000000, 0.5000000000000000000 ),
 .UNSPECIFIED. ) ;
#19841 = CARTESIAN_POINT ( 'NONE',  ( -7.472970580910000216, -74.00000000000000000, -38.65569705749999940 ) ) ;
#19842 = CARTESIAN_POINT ( 'NONE',  ( -6.439729480049999566, -101.2530993010000060, 13.76171823350000167 ) ) ;
#19843 = ORIENTED_EDGE ( 'NONE', *, *, #28319, .T. ) ;
#19844 = CARTESIAN_POINT ( 'NONE',  ( 26.88798373661718344, -72.41637509537598305, -11.07835129732953483 ) ) ;
#19845 = CARTESIAN_POINT ( 'NONE',  ( -12.49917433268771738, -101.1451610290395848, -10.60336746766995475 ) ) ;
#19846 = VERTEX_POINT ( 'NONE', #5094 ) ;
#19847 = CARTESIAN_POINT ( 'NONE',  ( 12.39757656149999931, -111.0000000000000000, -10.11435096289999969 ) ) ;
#19848 = CARTESIAN_POINT ( 'NONE',  ( -41.75000000000000000, -65.49083508809999898, 1.947031612730000028 ) ) ;
#19849 = ADVANCED_FACE ( 'NONE', ( #16011 ), #18815, .T. ) ;
#19850 = CARTESIAN_POINT ( 'NONE',  ( -0.6982943267950000310, -101.1292389600000092, -15.49059797790000026 ) ) ;
#19851 = FACE_OUTER_BOUND ( 'NONE', #4197, .T. ) ;
#19852 = CARTESIAN_POINT ( 'NONE',  ( -43.28961566200059252, -63.05619511567425661, -0.07254510122828666807 ) ) ;
#19853 = B_SPLINE_CURVE_WITH_KNOTS ( 'NONE', 5,
 ( #27655, #25876, #14650, #1414, #9852, #18900 ),
 .UNSPECIFIED., .F., .F.,
 ( 6, 6 ),
 ( 0.9548616571615553550, 1.000000000000000000 ),
 .UNSPECIFIED. ) ;
#19854 = CARTESIAN_POINT ( 'NONE',  ( -20.47543134015453248, -92.69183043850887316, -22.60564142679350397 ) ) ;
#19855 = ORIENTED_EDGE ( 'NONE', *, *, #9637, .F. ) ;
#19856 = ADVANCED_FACE ( 'NONE', ( #9454 ), #13828, .T. ) ;
#19857 = DIRECTION ( 'NONE',  ( -0.5000000000001882938, 0.000000000000000000, 0.8660254037843299058 ) ) ;
#19858 = CARTESIAN_POINT ( 'NONE',  ( 28.33616551327313715, -70.11425052315884443, 2.503553257605046323 ) ) ;
#19859 = DIRECTION ( 'NONE',  ( 0.2414462220490755373, 0.000000000000000000, -0.9704142011833032377 ) ) ;
#19860 = ADVANCED_FACE ( 'NONE', ( #17921 ), #461, .T. ) ;
#19861 = CARTESIAN_POINT ( 'NONE',  ( 6.890073352990000011, -40.75155002679999683, -21.70991749099999879 ) ) ;
#19862 = CARTESIAN_POINT ( 'NONE',  ( -38.08875739639999836, -82.25000000000000000, 9.476764215410000247 ) ) ;
#19863 = CARTESIAN_POINT ( 'NONE',  ( -12.00432114859999899, -65.97406652869999277, -23.19064400290000094 ) ) ;
#19864 = CARTESIAN_POINT ( 'NONE',  ( -17.93028678539999987, -18.50000000000000000, 10.99759328500000066 ) ) ;
#19865 = CARTESIAN_POINT ( 'NONE',  ( 0.000000000000000000, -80.50000000000000000, 40.00000000000000000 ) ) ;
#19866 = CARTESIAN_POINT ( 'NONE',  ( 25.52931313223885823, -93.31462968146665560, 11.30597120268183531 ) ) ;
#19867 = ORIENTED_EDGE ( 'NONE', *, *, #24990, .F. ) ;
#19868 = CARTESIAN_POINT ( 'NONE',  ( 9.024081099289999131, -19.49999992740000110, -18.94592230980000380 ) ) ;
#19869 = CARTESIAN_POINT ( 'NONE',  ( 21.93565869129999868, -36.00000000000000000, -11.17657094590000000 ) ) ;
#19870 = AXIS2_PLACEMENT_3D ( 'NONE', #19879, #15504, #24413 ) ;
#19871 = ORIENTED_EDGE ( 'NONE', *, *, #6184, .T. ) ;
#19872 = CARTESIAN_POINT ( 'NONE',  ( -14.06310087329999803, -61.59908875819999707, 21.57936076700000072 ) ) ;
#19873 = CARTESIAN_POINT ( 'NONE',  ( -12.94585355959999973, -101.1889999979999999, -9.402386697720000797 ) ) ;
#19874 = CARTESIAN_POINT ( 'NONE',  ( -12.89904789370000060, -65.07443093669999712, -21.58991903219999742 ) ) ;
#19875 = DIRECTION ( 'NONE',  ( 0.4740167705367959727, 0.000000000000000000, 0.8805158154456209640 ) ) ;
#19876 = CARTESIAN_POINT ( 'NONE',  ( 19.97124347238408859, -19.47946848935876929, -8.623261867002929293 ) ) ;
#19877 = CARTESIAN_POINT ( 'NONE',  ( 16.07378973510000009, -100.2511768809999921, 4.474534493000001056 ) ) ;
#19878 = ORIENTED_EDGE ( 'NONE', *, *, #24232, .F. ) ;
#19879 = CARTESIAN_POINT ( 'NONE',  ( -26.77683864449999973, -19.40000000000000213, -49.01467436490000296 ) ) ;
#19880 = AXIS2_PLACEMENT_3D ( 'NONE', #5996, #5727, #3551 ) ;
#19881 = CARTESIAN_POINT ( 'NONE',  ( 7.260629316970000247, -73.82505178009999725, -39.64169929279999849 ) ) ;
#19882 = EDGE_LOOP ( 'NONE', ( #3061, #6164, #20839, #1504 ) ) ;
#19883 = CARTESIAN_POINT ( 'NONE',  ( 7.409335217021491005, -92.49999999999998579, 29.58651093924895292 ) ) ;
#19884 = VERTEX_POINT ( 'NONE', #4947 ) ;
#19885 = ADVANCED_FACE ( 'NONE', ( #11023 ), #2774, .T. ) ;
#19886 = B_SPLINE_CURVE_WITH_KNOTS ( 'NONE', 5,
 ( #16476, #8146, #27572, #23465, #17032, #12495, #7612, #10307, #25379 ),
 .UNSPECIFIED., .F., .F.,
 ( 6, 3, 6 ),
 ( 0.000000000000000000, 0.5000000000000000000, 1.000000000000000000 ),
 .UNSPECIFIED. ) ;
#19887 = DIRECTION ( 'NONE',  ( 0.000000000000000000, 1.000000000000000000, 0.000000000000000000 ) ) ;
#19888 = CARTESIAN_POINT ( 'NONE',  ( 22.35211346940000254, -19.39383846089999963, 9.879721194109999161 ) ) ;
#19889 = DIRECTION ( 'NONE',  ( 0.000000000000000000, -1.000000000000000000, 0.000000000000000000 ) ) ;
#19890 = CARTESIAN_POINT ( 'NONE',  ( 24.83973459609999779, -92.98926436760000058, -13.74315515600000026 ) ) ;
#19891 = EDGE_CURVE ( 'NONE', #2012, #1944, #13201, .T. ) ;
#19892 = CIRCLE ( 'NONE', #23631, 1.000000000000000000 ) ;
#19893 = CARTESIAN_POINT ( 'NONE',  ( -13.82310862910000004, -74.00000000000000000, 36.20061004779999791 ) ) ;
#19894 = CARTESIAN_POINT ( 'NONE',  ( 8.034825427640001294, -66.63181251129999794, -24.57972215990000109 ) ) ;
#19895 = CARTESIAN_POINT ( 'NONE',  ( -16.82739518109305266, -98.07939314455124702, 9.438034146772373845 ) ) ;
#19896 = EDGE_LOOP ( 'NONE', ( #28353, #7914, #22823, #16395 ) ) ;
#19897 = CIRCLE ( 'NONE', #24108, 38.75000000000000000 ) ;
#19898 = DIRECTION ( 'NONE',  ( 0.9999792992113792911, 0.000000000000000000, 0.006434372441722923698 ) ) ;
#19899 = CARTESIAN_POINT ( 'NONE',  ( -12.54055638390000027, -100.2511768809999921, -11.00557226859999993 ) ) ;
#19900 = CARTESIAN_POINT ( 'NONE',  ( -7.225954378397760891, -73.65476501621135696, 39.40991843094596447 ) ) ;
#19901 = CARTESIAN_POINT ( 'NONE',  ( 22.65305255325292322, -60.89179363350914542, -7.201864690846052852 ) ) ;
#19902 = VERTEX_POINT ( 'NONE', #27248 ) ;
#19903 = CARTESIAN_POINT ( 'NONE',  ( -40.00000000000000000, -69.00000000000000000, 3.236300116779999679E-15 ) ) ;
#19904 = AXIS2_PLACEMENT_3D ( 'NONE', #26406, #6435, #24222 ) ;
#19905 = ORIENTED_EDGE ( 'NONE', *, *, #26126, .T. ) ;
#19906 = CARTESIAN_POINT ( 'NONE',  ( -5.298189715349999496, -100.9197081840000010, 14.69882786429999832 ) ) ;
#19907 = CARTESIAN_POINT ( 'NONE',  ( -22.71848792900000191, -80.00000000000000000, -32.61798286559999838 ) ) ;
#19908 = EDGE_LOOP ( 'NONE', ( #16414, #17850, #18005, #5653 ) ) ;
#19909 = AXIS2_PLACEMENT_3D ( 'NONE', #14263, #5234, #5082 ) ;
#19910 = CARTESIAN_POINT ( 'NONE',  ( -19.98504873792455072, -95.82120799309100789, 9.689515792764227697 ) ) ;
#19911 = ORIENTED_EDGE ( 'NONE', *, *, #18871, .T. ) ;
#19912 = CYLINDRICAL_SURFACE ( 'NONE', #3311, 53.34999999999998721 ) ;
#19913 = DIRECTION ( 'NONE',  ( -0.09756097560976716154, 0.000000000000000000, -0.9952295494196655712 ) ) ;
#19914 = ORIENTED_EDGE ( 'NONE', *, *, #21358, .T. ) ;
#19915 = CARTESIAN_POINT ( 'NONE',  ( 21.02965361369999897, -18.50000000000000000, -0.4426258060200000122 ) ) ;
#19916 = CARTESIAN_POINT ( 'NONE',  ( -21.93598400869999665, -79.95692792130000726, -32.60789339819999810 ) ) ;
#19917 = EDGE_CURVE ( 'NONE', #20323, #12729, #694, .T. ) ;
#19918 = ORIENTED_EDGE ( 'NONE', *, *, #16687, .T. ) ;
#19919 = PRODUCT_DEFINITION_FORMATION_WITH_SPECIFIED_SOURCE ( 'ANY', '', #14772, .NOT_KNOWN. ) ;
#19920 = CARTESIAN_POINT ( 'NONE',  ( -7.215414233289999757, -82.25000000000000000, 40.70731707320000226 ) ) ;
#19921 = DIRECTION ( 'NONE',  ( -0.6405991297529511908, 3.017111016349766299E-15, -0.7678754814159401976 ) ) ;
#19922 = CARTESIAN_POINT ( 'NONE',  ( -23.46882160569999698, -92.76843000840000286, -19.22844388999999765 ) ) ;
#19923 = CARTESIAN_POINT ( 'NONE',  ( 7.635702898730000854, -101.6454117330000031, 14.06304778130000166 ) ) ;
#19924 = EDGE_LOOP ( 'NONE', ( #27714, #20746, #22853, #9283 ) ) ;
#19925 = ADVANCED_FACE ( 'NONE', ( #13976 ), #5605, .T. ) ;
#19926 = DIRECTION ( 'NONE',  ( 0.000000000000000000, 1.000000000000000000, 0.000000000000000000 ) ) ;
#19927 = DIRECTION ( 'NONE',  ( 0.000000000000000000, -1.000000000000000000, 0.000000000000000000 ) ) ;
#19928 = CARTESIAN_POINT ( 'NONE',  ( 47.25000000000000000, -77.00000000000000000, -13.75000000000000000 ) ) ;
#19929 = CARTESIAN_POINT ( 'NONE',  ( -3.830277821634817226, -99.42096436988184394, -18.32509845586109876 ) ) ;
#19930 = CARTESIAN_POINT ( 'NONE',  ( 8.125631349740000786, -101.1889999979999999, 24.17072847820000092 ) ) ;
#19931 = CARTESIAN_POINT ( 'NONE',  ( 10.85455877420105431, -72.50961925363316141, -26.83546891656583711 ) ) ;
#19932 = CARTESIAN_POINT ( 'NONE',  ( -17.93694630730000128, -18.50000000000000000, 13.70495702920000092 ) ) ;
#19933 = EDGE_LOOP ( 'NONE', ( #4413, #2165, #12956, #23950 ) ) ;
#19934 = AXIS2_PLACEMENT_3D ( 'NONE', #13044, #26915, #17440 ) ;
#19935 = FACE_OUTER_BOUND ( 'NONE', #21480, .T. ) ;
#19936 = CARTESIAN_POINT ( 'NONE',  ( 20.30102379280298308, -72.26179938780217071, -30.97095677777052813 ) ) ;
#19937 = CARTESIAN_POINT ( 'NONE',  ( -23.91929231898793162, -92.72059904819356291, -18.92399198549271588 ) ) ;
#19938 = DIRECTION ( 'NONE',  ( 0.4794255386042032829, 0.000000000000000000, 0.8775825618903726477 ) ) ;
#19939 = CARTESIAN_POINT ( 'NONE',  ( -0.02603423451098885524, -92.77521214511344283, -30.50001158162930892 ) ) ;
#19940 = SHAPE_DEFINITION_REPRESENTATION ( #28051, #10734 ) ;
#19941 = CARTESIAN_POINT ( 'NONE',  ( 9.476764215410000247, -74.50000000000000000, 38.08875739639999836 ) ) ;
#19942 = ORIENTED_EDGE ( 'NONE', *, *, #9195, .F. ) ;
#19943 = DIRECTION ( 'NONE',  ( 0.4794255386042033384, 0.000000000000000000, 0.8775825618903726477 ) ) ;
#19945 = VERTEX_POINT ( 'NONE', #17775 ) ;
#19944 = CIRCLE ( 'NONE', #5081, 22.03370205219999889 ) ;
#19946 = FACE_OUTER_BOUND ( 'NONE', #28090, .T. ) ;
#19947 = FACE_OUTER_BOUND ( 'NONE', #22704, .T. ) ;
#19948 = EDGE_LOOP ( 'NONE', ( #6401, #24035, #3737, #9853 ) ) ;
#19949 = CARTESIAN_POINT ( 'NONE',  ( 15.09235194470000074, -95.70964358299998764, 17.10662658029999861 ) ) ;
#19950 = CIRCLE ( 'NONE', #9735, 25.11294200180000047 ) ;
#19951 = AXIS2_PLACEMENT_3D ( 'NONE', #21412, #1469, #26215 ) ;
#19952 = ADVANCED_FACE ( 'NONE', ( #26660 ), #6702, .T. ) ;
#19953 = CIRCLE ( 'NONE', #7437, 21.60095686220000033 ) ;
#19954 = VERTEX_POINT ( 'NONE', #15711 ) ;
#19955 = AXIS2_PLACEMENT_3D ( 'NONE', #1070, #8151, #7617 ) ;
#19956 = CARTESIAN_POINT ( 'NONE',  ( -4.610939809759999619, -98.36043306160000554, -18.57959422089999890 ) ) ;
#19957 = CARTESIAN_POINT ( 'NONE',  ( 5.787273401498926440, -93.40025063785100201, -27.00970585107326372 ) ) ;
#19958 = DIRECTION ( 'NONE',  ( 1.000000000000000000, 0.000000000000000000, 0.000000000000000000 ) ) ;
#19959 = CARTESIAN_POINT ( 'NONE',  ( -19.63026485099999618, -96.58392759020000540, 8.276969169350000044 ) ) ;
#19960 = CARTESIAN_POINT ( 'NONE',  ( -29.71162786834675629, -92.72722989462940291, 6.889795938524829744 ) ) ;
#19961 = CARTESIAN_POINT ( 'NONE',  ( 22.41768028079999908, -65.59529275500000267, 11.91456822289999984 ) ) ;
#19962 = EDGE_LOOP ( 'NONE', ( #8636, #12013, #4748, #17699 ) ) ;
#19963 = ADVANCED_FACE ( 'NONE', ( #2330 ), #17237, .F. ) ;
#19964 = DIRECTION ( 'NONE',  ( 0.4794255386042036715, 0.000000000000000000, 0.8775825618903724257 ) ) ;
#19965 = CARTESIAN_POINT ( 'NONE',  ( 23.16587695349999976, -49.87340317219999974, 0.05359468315350000150 ) ) ;
#19966 = CARTESIAN_POINT ( 'NONE',  ( 24.11425572830000164, -65.50583529140000394, 10.76556153070000121 ) ) ;
#19967 = CARTESIAN_POINT ( 'NONE',  ( 40.38463872053225856, -74.25043946767728187, 7.240437622435978327 ) ) ;
#19968 = ORIENTED_EDGE ( 'NONE', *, *, #12863, .F. ) ;
#19969 = B_SPLINE_CURVE_WITH_KNOTS ( 'NONE', 5,
 ( #28175, #22052, #21754, #15030, #2099, #28724 ),
 .UNSPECIFIED., .F., .F.,
 ( 6, 6 ),
 ( 0.000000000000000000, 1.000000000000000000 ),
 .UNSPECIFIED. ) ;
#19970 = CARTESIAN_POINT ( 'NONE',  ( -20.52703897250000153, -55.79355142130000900, 14.83226277630000034 ) ) ;
#19971 = CARTESIAN_POINT ( 'NONE',  ( -13.55845395200000070, -92.92146065570000246, 27.19007895920000095 ) ) ;
#19972 = DIRECTION ( 'NONE',  ( 1.000000000000000000, 0.000000000000000000, 0.000000000000000000 ) ) ;
#19973 = VERTEX_POINT ( 'NONE', #18208 ) ;
#19974 = CARTESIAN_POINT ( 'NONE',  ( 28.54888737639999974, -72.55114965769999458, 2.312894923860000063 ) ) ;
#19975 = CARTESIAN_POINT ( 'NONE',  ( 0.3686832740489999760, -101.0640712160000021, -16.09543371239999843 ) ) ;
#19976 = CARTESIAN_POINT ( 'NONE',  ( 25.79807934023626714, -74.30236118189925776, -29.52720746065469015 ) ) ;
#19977 = CARTESIAN_POINT ( 'NONE',  ( -12.76533745180000068, -68.20220936460000871, -23.31270229540000116 ) ) ;
#19978 = CARTESIAN_POINT ( 'NONE',  ( 23.78692593859999960, -64.96416322790000208, -8.575408708140001224 ) ) ;
#19979 = AXIS2_PLACEMENT_3D ( 'NONE', #15498, #2418, #24408 ) ;
#19980 = AXIS2_PLACEMENT_3D ( 'NONE', #17750, #4481, #2747 ) ;
#19981 = ADVANCED_FACE ( 'NONE', ( #20097 ), #6999, .T. ) ;
#19982 = CYLINDRICAL_SURFACE ( 'NONE', #11993, 0.9999999999999988898 ) ;
#19983 = CARTESIAN_POINT ( 'NONE',  ( -2.645751311070000167, -74.00000000000000000, 46.75000000000000000 ) ) ;
#19984 = EDGE_CURVE ( 'NONE', #4769, #8407, #2485, .T. ) ;
#19985 = VERTEX_POINT ( 'NONE', #9153 ) ;
#19986 = CARTESIAN_POINT ( 'NONE',  ( -39.57487616197608560, -65.66931566140442555, -2.266171304482763382 ) ) ;
#19987 = CARTESIAN_POINT ( 'NONE',  ( -34.89999999999999858, -82.50000000000000000, 0.000000000000000000 ) ) ;
#19988 = CARTESIAN_POINT ( 'NONE',  ( -4.317742246239999915, -95.94970068790001960, 22.11177757589999970 ) ) ;
#19989 = VERTEX_POINT ( 'NONE', #13685 ) ;
#19990 = CARTESIAN_POINT ( 'NONE',  ( 7.229383731089999543, -73.50070240710000746, 39.23650411529999360 ) ) ;
#19991 = CARTESIAN_POINT ( 'NONE',  ( 9.108757905360000962, -94.52419443349998573, -22.22442264740000084 ) ) ;
#19992 = CARTESIAN_POINT ( 'NONE',  ( 20.04401346829999753, -25.53205114500000050, -8.807493111859999502 ) ) ;
#19993 = CARTESIAN_POINT ( 'NONE',  ( 22.66861466926381397, -19.47159664147383751, 0.9610264626648014064 ) ) ;
#19994 = CARTESIAN_POINT ( 'NONE',  ( -7.243334595760000383, -101.4829589650000088, 14.41017875130000014 ) ) ;
#19995 = ORIENTED_EDGE ( 'NONE', *, *, #499, .F. ) ;
#19996 = CARTESIAN_POINT ( 'NONE',  ( 26.81105948361605229, -72.58019056410417136, -10.66796337414779217 ) ) ;
#19997 = CARTESIAN_POINT ( 'NONE',  ( -13.32816333360000094, -99.92967571559999840, -11.12411022969999941 ) ) ;
#19998 = CARTESIAN_POINT ( 'NONE',  ( 9.090175673379999211, -35.93817878899999840, -20.25147856850000139 ) ) ;
#19999 = CIRCLE ( 'NONE', #22411, 0.4999999999999983347 ) ;
#20000 = CARTESIAN_POINT ( 'NONE',  ( 21.51532853426891023, -35.83080157483318118, -6.934509737378918182 ) ) ;
#20001 = AXIS2_PLACEMENT_3D ( 'NONE', #24554, #5940, #259 ) ;
#20002 = MECHANICAL_DESIGN_GEOMETRIC_PRESENTATION_REPRESENTATION (  '', ( #1417 ), #25150 ) ;
#20003 = DIRECTION ( 'NONE',  ( -0.7071067811865474617, 0.000000000000000000, -0.7071067811865474617 ) ) ;
#20004 = CARTESIAN_POINT ( 'NONE',  ( 21.41854095929999602, -18.50000000000000000, 0.3037881489800000057 ) ) ;
#20005 = CARTESIAN_POINT ( 'NONE',  ( 27.68682485439999752, -28.10000000000000142, 50.68039294919999804 ) ) ;
#20006 = CARTESIAN_POINT ( 'NONE',  ( -20.84286287520331271, -92.82044061134170931, -22.26713171995569240 ) ) ;
#20007 = VERTEX_POINT ( 'NONE', #22591 ) ;
#20008 = CARTESIAN_POINT ( 'NONE',  ( -33.18922156509999866, -79.25000000000000000, -21.87551306609999813 ) ) ;
#20009 = CARTESIAN_POINT ( 'NONE',  ( 28.91458899939999938, -72.00000000000000000, 3.086557976320000396 ) ) ;
#20010 = DIRECTION ( 'NONE',  ( 0.9704142011833034598, 0.000000000000000000, 0.2414462220490750377 ) ) ;
#20011 = DIRECTION ( 'NONE',  ( -0.8940996652532122724, 0.000000000000000000, 0.4478680481951061165 ) ) ;
#20012 = DIRECTION ( 'NONE',  ( 0.000000000000000000, -1.000000000000000000, 0.000000000000000000 ) ) ;
#20013 = CARTESIAN_POINT ( 'NONE',  ( 25.46584391311435880, -59.75127557667808276, 1.379760577311673675 ) ) ;
#20014 = CARTESIAN_POINT ( 'NONE',  ( -38.44108623807613867, -65.10668761693770534, -2.885092602787210136 ) ) ;
#20015 = CARTESIAN_POINT ( 'NONE',  ( -40.70731707320000226, -77.00000000000000000, 7.215414233289999757 ) ) ;
#20016 = CARTESIAN_POINT ( 'NONE',  ( 25.12718488642092396, -93.38554229052554945, 11.59376715993274942 ) ) ;
#20017 = VERTEX_POINT ( 'NONE', #2634 ) ;
#20018 = CARTESIAN_POINT ( 'NONE',  ( 7.734359208889999948, -19.46510056589999849, -20.63161901249999985 ) ) ;
#20019 = EDGE_CURVE ( 'NONE', #10596, #18106, #4060, .T. ) ;
#20020 = AXIS2_PLACEMENT_3D ( 'NONE', #12850, #21765, #28183 ) ;
#20022 = ADVANCED_FACE ( 'NONE', ( #10019 ), #27935, .T. ) ;
#20021 = AXIS2_PLACEMENT_3D ( 'NONE', #26972, #22295, #15720 ) ;
#20023 = ORIENTED_EDGE ( 'NONE', *, *, #10927, .F. ) ;
#20024 = CIRCLE ( 'NONE', #24215, 59.04999999999999716 ) ;
#20025 = CARTESIAN_POINT ( 'NONE',  ( -13.87613801740000063, -58.81368956530000247, 21.27373992140000070 ) ) ;
#20026 = CARTESIAN_POINT ( 'NONE',  ( 7.224488193780730150, -74.42768721769506612, 40.61475266869189937 ) ) ;
#20027 = B_SPLINE_CURVE_WITH_KNOTS ( 'NONE', 5,
 ( #13566, #27283, #14012, #26992, #4978, #22621 ),
 .UNSPECIFIED., .F., .F.,
 ( 6, 6 ),
 ( 0.000000000000000000, 1.000000000000000000 ),
 .UNSPECIFIED. ) ;
#20028 = EDGE_CURVE ( 'NONE', #26317, #9320, #14891, .T. ) ;
#20029 = CARTESIAN_POINT ( 'NONE',  ( -27.11354574210000123, -93.21603264559999502, -0.5572048120379999858 ) ) ;
#20030 = CARTESIAN_POINT ( 'NONE',  ( -11.07305194678827043, -19.50000000000000000, -24.81486620154639411 ) ) ;
#20031 = EDGE_CURVE ( 'NONE', #26140, #7537, #16624, .T. ) ;
#20032 = CARTESIAN_POINT ( 'NONE',  ( -22.27191869549999836, -94.59276292389999696, -8.381623179300000004 ) ) ;
#20033 = CARTESIAN_POINT ( 'NONE',  ( 19.96747957240500071, -19.47954630362596973, -8.626122652564374604 ) ) ;
#20034 = CARTESIAN_POINT ( 'NONE',  ( 16.77193911569999685, -99.58396362730000817, 4.490484942109999267 ) ) ;
#20035 = ORIENTED_EDGE ( 'NONE', *, *, #19523, .F. ) ;
#20036 = CARTESIAN_POINT ( 'NONE',  ( 7.460698725479999927E-15, -73.50000000000000000, 40.00000000000000000 ) ) ;
#20037 = CARTESIAN_POINT ( 'NONE',  ( 29.06613905497733086, -74.35453649132965381, -26.34452374057316604 ) ) ;
#20038 = CARTESIAN_POINT ( 'NONE',  ( -13.21936810159999887, -100.9405345029999950, -8.915376394229999946 ) ) ;
#20039 = VERTEX_POINT ( 'NONE', #27813 ) ;
#20040 = DIRECTION ( 'NONE',  ( -0.8660254037838959196, 0.000000000000000000, 0.5000000000009399148 ) ) ;
#20041 = CARTESIAN_POINT ( 'NONE',  ( 22.14137210369998243, -52.59522851919948039, 10.05377507689999028 ) ) ;
#20042 = B_SPLINE_CURVE_WITH_KNOTS ( 'NONE', 3,
 ( #28645, #28504, #21529, #26189, #1586, #10425 ),
 .UNSPECIFIED., .F., .F.,
 ( 4, 2, 4 ),
 ( 0.000000000000000000, 0.5000000000000000000, 1.000000000000000000 ),
 .UNSPECIFIED. ) ;
#20043 = DIRECTION ( 'NONE',  ( 0.000000000000000000, 1.000000000000000000, 0.000000000000000000 ) ) ;
#20044 = DIRECTION ( 'NONE',  ( 0.8476796612309128731, -0.2588190451029734884, 0.4630895095199519806 ) ) ;
#20045 = CIRCLE ( 'NONE', #10256, 57.75000000000000000 ) ;
#20046 = DIRECTION ( 'NONE',  ( 1.000000000000000000, 0.000000000000000000, 0.000000000000000000 ) ) ;
#20047 = CARTESIAN_POINT ( 'NONE',  ( 24.12141425730000321, -92.50732182800000203, -16.93547630009999949 ) ) ;
#20048 = AXIS2_PLACEMENT_3D ( 'NONE', #5210, #27070, #27512 ) ;
#20049 = AXIS2_PLACEMENT_3D ( 'NONE', #11397, #16366, #2394 ) ;
#20050 = CARTESIAN_POINT ( 'NONE',  ( -13.92338919490000038, -74.00000000000000000, 36.27080632649999359 ) ) ;
#20051 = CARTESIAN_POINT ( 'NONE',  ( -32.76307242539326836, -79.87735098181109095, -22.39909635432421453 ) ) ;
#20052 = CARTESIAN_POINT ( 'NONE',  ( -16.09526080732491948, -99.28256948951555216, 7.457957185716643345 ) ) ;
#20053 = ORIENTED_EDGE ( 'NONE', *, *, #5478, .T. ) ;
#20054 = CARTESIAN_POINT ( 'NONE',  ( -12.00286543741112766, -72.31233190808829647, -26.16426295086472820 ) ) ;
#20055 = DIRECTION ( 'NONE',  ( 0.000000000000000000, 0.000000000000000000, 1.000000000000000000 ) ) ;
#20056 = CARTESIAN_POINT ( 'NONE',  ( -12.64324746780000019, -99.97545561319999763, -11.21434624260000135 ) ) ;
#20057 = CIRCLE ( 'NONE', #1028, 12.00000000000000000 ) ;
#20058 = DIRECTION ( 'NONE',  ( 0.000000000000000000, 1.000000000000000000, 0.000000000000000000 ) ) ;
#20059 = CARTESIAN_POINT ( 'NONE',  ( -40.30310653759999440, -74.34472676629999910, -7.255206491290000059 ) ) ;
#20060 = ORIENTED_EDGE ( 'NONE', *, *, #18637, .T. ) ;
#20061 = CARTESIAN_POINT ( 'NONE',  ( -31.99658184870000355, -79.50000000000000000, -31.99658184870000355 ) ) ;
#20062 = EDGE_LOOP ( 'NONE', ( #24901, #7453, #2746, #9149 ) ) ;
#20063 = EDGE_CURVE ( 'NONE', #24483, #3233, #5832, .T. ) ;
#20064 = FACE_OUTER_BOUND ( 'NONE', #2577, .T. ) ;
#20065 = DIRECTION ( 'NONE',  ( 0.8775825618903722036, 0.000000000000000000, -0.4794255386042041156 ) ) ;
#20066 = CIRCLE ( 'NONE', #4233, 19.50000000000000000 ) ;
#20067 = CARTESIAN_POINT ( 'NONE',  ( 12.04737265770000043, -101.6484611540000031, -10.52904611289999970 ) ) ;
#20068 = CIRCLE ( 'NONE', #8424, 0.5000000000000004441 ) ;
#20069 = EDGE_CURVE ( 'NONE', #10652, #20846, #9311, .T. ) ;
#20070 = ORIENTED_EDGE ( 'NONE', *, *, #14908, .F. ) ;
#20071 = AXIS2_PLACEMENT_3D ( 'NONE', #27554, #9462, #16461 ) ;
#20072 = VERTEX_POINT ( 'NONE', #20981 ) ;
#20073 = CARTESIAN_POINT ( 'NONE',  ( -26.60615435977595311, -93.74885976973425272, -1.266735793207066862 ) ) ;
#20074 = CARTESIAN_POINT ( 'NONE',  ( 21.43458377180000340, -94.34470043860000033, 13.67121948690000011 ) ) ;
#20075 = CARTESIAN_POINT ( 'NONE',  ( 46.59019410810000039, -73.90401672450001058, -3.140090762159999827 ) ) ;
#20076 = EDGE_LOOP ( 'NONE', ( #13565, #279, #26935, #26089 ) ) ;
#20077 = CARTESIAN_POINT ( 'NONE',  ( -39.50000000000000000, -63.30468293320000583, -2.309401076760000393 ) ) ;
#20078 = CARTESIAN_POINT ( 'NONE',  ( -22.22906625010000070, -79.49999999740001044, -32.83566834300000181 ) ) ;
#20079 = VERTEX_POINT ( 'NONE', #12212 ) ;
#20080 = CARTESIAN_POINT ( 'NONE',  ( 8.855030550580000437, -36.23917065910000446, -21.13310771060000093 ) ) ;
#20081 = CARTESIAN_POINT ( 'NONE',  ( -13.24613574540000016, -93.92589062410000622, -21.39339146240000034 ) ) ;
#20082 = CARTESIAN_POINT ( 'NONE',  ( 0.000000000000000000, -19.00000000000000000, 0.000000000000000000 ) ) ;
#20083 = ORIENTED_EDGE ( 'NONE', *, *, #15529, .F. ) ;
#20084 = CARTESIAN_POINT ( 'NONE',  ( -6.191817604487320104, -101.6407018583229416, 14.75961303763012644 ) ) ;
#20085 = CARTESIAN_POINT ( 'NONE',  ( 13.81100082510000071, -99.92967571559999840, -10.51865128849999920 ) ) ;
#20086 = CARTESIAN_POINT ( 'NONE',  ( -40.34085930499999506, -74.29298176469998793, 7.252015964940000003 ) ) ;
#20087 = CARTESIAN_POINT ( 'NONE',  ( -21.85457041760000152, -74.43208506860000284, -32.66023292170000758 ) ) ;
#20088 = CARTESIAN_POINT ( 'NONE',  ( -1.451488207819999987, -56.25996389440000200, -23.46934156900000090 ) ) ;
#20089 = CIRCLE ( 'NONE', #21938, 1.000000000000000888 ) ;
#20090 = CARTESIAN_POINT ( 'NONE',  ( 0.000000000000000000, -28.69999999999999929, 0.000000000000000000 ) ) ;
#20091 = PLANE ( 'NONE',  #23003 ) ;
#20092 = CARTESIAN_POINT ( 'NONE',  ( -17.39698466460000148, -18.50000000000000000, 12.78927784919999944 ) ) ;
#20093 = ORIENTED_EDGE ( 'NONE', *, *, #13481, .F. ) ;
#20094 = CARTESIAN_POINT ( 'NONE',  ( -8.508623865889999749, -94.26884736950000843, -22.81720901600000317 ) ) ;
#20095 = DIRECTION ( 'NONE',  ( 0.9037419867099890647, 0.000000000000000000, -0.4280775881279956785 ) ) ;
#20096 = CYLINDRICAL_SURFACE ( 'NONE', #10326, 18.64285714290000939 ) ;
#20097 = FACE_OUTER_BOUND ( 'NONE', #21208, .T. ) ;
#20098 = CARTESIAN_POINT ( 'NONE',  ( -10.20110288159999890, -80.50000000000000000, 41.00000000000000000 ) ) ;
#20099 = CARTESIAN_POINT ( 'NONE',  ( -14.65554054705737741, -101.0953223671037335, 4.722896106945597694 ) ) ;
#20100 = ADVANCED_FACE ( 'NONE', ( #18500 ), #5151, .T. ) ;
#20101 = B_SPLINE_SURFACE_WITH_KNOTS ( 'NONE', 5, 5, ( 
 ( #14822, #23726, #2424, #15653, #13471, #25914 ),
 ( #2271, #14959, #11279, #20185, #12489, #3906 ),
 ( #10301, #9099, #15802, #19212, #12772, #3769 ),
 ( #21682, #28101, #12630, #10439, #19357, #28230 ),
 ( #20324, #27043, #11423, #395, #4745, #7087 ),
 ( #13624, #15950, #9244, #18146, #22532, #2574 ) ),
 .UNSPECIFIED., .F., .F., .F.,
 ( 6, 6 ),
 ( 6, 6 ),
 ( 2.788355763089999773, 6.107000906329999701 ),
 ( 0.000000000000000000, 0.5000000000000000000 ),
 .UNSPECIFIED. ) ;
#20102 = DIRECTION ( 'NONE',  ( 1.000000000000000000, 0.000000000000000000, 0.000000000000000000 ) ) ;
#20103 = CARTESIAN_POINT ( 'NONE',  ( 5.753106463249999969, -2.000000000000000000, 10.53099074269999846 ) ) ;
#20104 = EDGE_CURVE ( 'NONE', #24926, #20274, #11388, .T. ) ;
#20105 = ORIENTED_EDGE ( 'NONE', *, *, #25738, .F. ) ;
#20106 = CARTESIAN_POINT ( 'NONE',  ( 21.34096039099999942, -97.41042626319999442, -2.228915448369999996 ) ) ;
#20107 = ORIENTED_EDGE ( 'NONE', *, *, #15749, .F. ) ;
#20108 = CARTESIAN_POINT ( 'NONE',  ( -11.45174557200000010, -57.47815920939999756, 20.36405547780000092 ) ) ;
#20109 = DIRECTION ( 'NONE',  ( 0.4794255386042037270, 0.000000000000000000, 0.8775825618903724257 ) ) ;
#20110 = EDGE_LOOP ( 'NONE', ( #28732, #28528 ) ) ;
#20111 = CARTESIAN_POINT ( 'NONE',  ( 15.00024946600000142, -95.51664469100001043, 17.13920226819999826 ) ) ;
#20112 = CARTESIAN_POINT ( 'NONE',  ( -3.380646432312965910, -68.17003325777139366, -27.59278602273885994 ) ) ;
#20113 = CARTESIAN_POINT ( 'NONE',  ( 7.773738738802946635, -93.98969193916553877, -24.92838943285665465 ) ) ;
#20114 = CARTESIAN_POINT ( 'NONE',  ( -40.00000000000000000, -69.00000000000000000, 0.000000000000000000 ) ) ;
#20115 = CARTESIAN_POINT ( 'NONE',  ( -35.88566914520000495, -74.50000000000000000, -26.69328098980000163 ) ) ;
#20116 = CARTESIAN_POINT ( 'NONE',  ( -29.64623384722952082, -92.61393927536423121, 7.166097978304951432 ) ) ;
#20117 = CARTESIAN_POINT ( 'NONE',  ( 21.57540932361363417, -37.72269071045047895, -7.960245178404622202 ) ) ;
#20118 = ORIENTED_EDGE ( 'NONE', *, *, #17856, .T. ) ;
#20119 = CARTESIAN_POINT ( 'NONE',  ( 26.69293917519999937, -34.10310889129999623, 48.86109741659999628 ) ) ;
#20120 = CARTESIAN_POINT ( 'NONE',  ( 40.00000000000000000, -69.00000000000000000, 4.790612351260000516E-15 ) ) ;
#20121 = CARTESIAN_POINT ( 'NONE',  ( -13.75178900340000077, -72.82938648530000592, -25.17248092229999656 ) ) ;
#20122 = VERTEX_POINT ( 'NONE', #5245 ) ;
#20123 = DIRECTION ( 'NONE',  ( 0.000000000000000000, -1.000000000000000000, 0.000000000000000000 ) ) ;
#20124 = CARTESIAN_POINT ( 'NONE',  ( -15.24159474039999829, -92.86430477140000050, 25.11115096520000378 ) ) ;
#20125 = CARTESIAN_POINT ( 'NONE',  ( 7.700566120479999555, -64.93340739229999770, -23.87431538810000120 ) ) ;
#20126 = ORIENTED_EDGE ( 'NONE', *, *, #7421, .T. ) ;
#20127 = CARTESIAN_POINT ( 'NONE',  ( 27.43242808539999800, -69.88456486680000523, 1.405611812030000074 ) ) ;
#20128 = VECTOR ( 'NONE', #15098, 1000.000000000000000 ) ;
#20129 = CARTESIAN_POINT ( 'NONE',  ( 0.2072563983730000281, -101.2063419769999939, -15.98545391140000049 ) ) ;
#20130 = CARTESIAN_POINT ( 'NONE',  ( 7.362282589679999489, -57.47832521680000184, -22.17287418769999974 ) ) ;
#20131 = CARTESIAN_POINT ( 'NONE',  ( 22.18552055780000032, -36.00000000000000000, -11.24205708569999906 ) ) ;
#20132 = CARTESIAN_POINT ( 'NONE',  ( -11.77274832230000001, -49.87554870529999818, -19.87235798440000423 ) ) ;
#20133 = AXIS2_PLACEMENT_3D ( 'NONE', #5401, #5535, #7868 ) ;
#20134 = EDGE_CURVE ( 'NONE', #22535, #19113, #10001, .T. ) ;
#20135 = DIRECTION ( 'NONE',  ( -0.9952295494196654602, 0.000000000000000000, 0.09756097560976760563 ) ) ;
#20136 = CARTESIAN_POINT ( 'NONE',  ( -34.11790219230000076, -74.50000000000000000, -24.21840725559999896 ) ) ;
#20137 = EDGE_CURVE ( 'NONE', #584, #12535, #18657, .T. ) ;
#20138 = ADVANCED_FACE ( 'NONE', ( #7591 ), #9555, .T. ) ;
#20139 = ORIENTED_EDGE ( 'NONE', *, *, #12139, .T. ) ;
#20140 = CARTESIAN_POINT ( 'NONE',  ( -14.34979093519999971, -92.51572464539999885, 25.42969430229999972 ) ) ;
#20141 = CARTESIAN_POINT ( 'NONE',  ( 15.02247708185264941, -101.1962283502375470, 2.723567765951154129 ) ) ;
#20142 = VECTOR ( 'NONE', #10496, 1000.000000000000000 ) ;
#20143 = CARTESIAN_POINT ( 'NONE',  ( 17.21337473110000005, -95.77248627129999647, 14.26927196279999954 ) ) ;
#20144 = EDGE_LOOP ( 'NONE', ( #25189, #21151, #15215, #16327 ) ) ;
#20145 = CARTESIAN_POINT ( 'NONE',  ( 36.29172732829999859, -79.00000000000000000, -14.94947765220000058 ) ) ;
#20146 = CARTESIAN_POINT ( 'NONE',  ( 22.66360973360000131, -92.65509162899999751, 15.93308052109999906 ) ) ;
#20147 = CARTESIAN_POINT ( 'NONE',  ( 23.74951379730920920, -19.48875272113166446, 1.479235313801489538 ) ) ;
#20148 = ORIENTED_EDGE ( 'NONE', *, *, #15189, .T. ) ;
#20149 = DIRECTION ( 'NONE',  ( 0.000000000000000000, 1.000000000000000000, 0.000000000000000000 ) ) ;
#20150 = CARTESIAN_POINT ( 'NONE',  ( -12.47284051790895809, -101.5526869446301106, -10.13888011385641441 ) ) ;
#20151 = CARTESIAN_POINT ( 'NONE',  ( 8.351979489730000594, -36.77152986899999831, -21.41523737049999809 ) ) ;
#20152 = CIRCLE ( 'NONE', #9461, 39.75000000000000000 ) ;
#20153 = CARTESIAN_POINT ( 'NONE',  ( 9.000933793642678538, -19.49520308528501999, -19.19207797698259910 ) ) ;
#20154 = CARTESIAN_POINT ( 'NONE',  ( -23.86485386499999706, -74.50000000000000000, -34.47145558279999733 ) ) ;
#20155 = EDGE_CURVE ( 'NONE', #1013, #27440, #15821, .T. ) ;
#20156 = CARTESIAN_POINT ( 'NONE',  ( 2.664535259099999805E-15, -18.50000000000000000, 7.105427357599999217E-15 ) ) ;
#20157 = CARTESIAN_POINT ( 'NONE',  ( 10.56351947379999956, -19.46510050329999686, 19.33639269489999890 ) ) ;
#20158 = DIRECTION ( 'NONE',  ( 0.000000000000000000, 0.000000000000000000, 1.000000000000000000 ) ) ;
#20159 = DIRECTION ( 'NONE',  ( 0.000000000000000000, -1.000000000000000000, 0.000000000000000000 ) ) ;
#20160 = CARTESIAN_POINT ( 'NONE',  ( -13.18577703620000108, -18.86473241050000027, 19.56302201480000136 ) ) ;
#20161 = CARTESIAN_POINT ( 'NONE',  ( -18.85761467144973835, -98.17436949385547962, -7.631504019717256782 ) ) ;
#20162 = DIRECTION ( 'NONE',  ( 6.123031769109993025E-17, 0.000000000000000000, -1.000000000000000000 ) ) ;
#20163 = B_SPLINE_SURFACE_WITH_KNOTS ( 'NONE', 5, 5, ( 
 ( #23789, #4104, #10224, #19690, #28436, #25844, #10495, #15016, #12549 ),
 ( #16953, #21463, #25975, #8323, #26116, #5866, #1517, #19276, #28162 ),
 ( #5999, #3968, #26267, #10778, #19136, #28025, #15155, #14746, #19410 ),
 ( #3827, #6289, #3554, #14616, #12690, #28581, #21603, #1659, #16809 ),
 ( #28291, #17226, #23930, #12829, #12975, #25704, #11782, #13125, #753 ),
 ( #311, #16008, #16299, #9598, #14126, #20834, #13973, #4253, #2631 ),
 ( #23024, #27245, #5091, #4805, #18497, #2771, #27391, #11626, #7282 ),
 ( #11478, #20384, #3075, #25209, #22588, #5242, #22037, #20693, #7439 ),
 ( #11928, #25057, #22878, #24219, #458, #24913, #8614, #11338, #9151 ) ),
 .UNSPECIFIED., .F., .F., .F.,
 ( 6, 3, 6 ),
 ( 6, 3, 6 ),
 ( 112.4516929440000013, 115.4092999559999981, 122.9563471670000041 ),
 ( 0.000000000000000000, 1.000000000000000000, 2.000000000000000000 ),
 .UNSPECIFIED. ) ;
#20164 = CIRCLE ( 'NONE', #19696, 24.50000000000000000 ) ;
#20165 = FACE_OUTER_BOUND ( 'NONE', #27522, .T. ) ;
#20166 = CARTESIAN_POINT ( 'NONE',  ( 25.35615114710841311, -58.58931700480601990, 1.380148426380368720 ) ) ;
#20167 = DIRECTION ( 'NONE',  ( 0.000000000000000000, 0.000000000000000000, 1.000000000000000000 ) ) ;
#20168 = LINE ( 'NONE', #241, #20682 ) ;
#20169 = EDGE_LOOP ( 'NONE', ( #18252, #27752, #23449, #20638 ) ) ;
#20170 = CARTESIAN_POINT ( 'NONE',  ( 29.70835240799999966, -93.00000000000000000, 6.903897247299999762 ) ) ;
#20171 = ADVANCED_FACE ( 'NONE', ( #22977 ), #15839, .T. ) ;
#20172 = CARTESIAN_POINT ( 'NONE',  ( 7.933291312079999713, -100.9679265919999978, 13.53917068360000009 ) ) ;
#20173 = AXIS2_PLACEMENT_3D ( 'NONE', #3913, #21686, #5817 ) ;
#20174 = ADVANCED_FACE ( 'NONE', ( #6797 ), #27012, .T. ) ;
#20175 = ORIENTED_EDGE ( 'NONE', *, *, #19178, .F. ) ;
#20176 = CARTESIAN_POINT ( 'NONE',  ( -14.22204520130000027, -64.47177057220000052, 21.80995652580000410 ) ) ;
#20177 = CARTESIAN_POINT ( 'NONE',  ( -13.32832959340000123, -60.38621941009999716, 20.74301091450000101 ) ) ;
#20178 = CYLINDRICAL_SURFACE ( 'NONE', #10308, 57.74999999999999289 ) ;
#20179 = CARTESIAN_POINT ( 'NONE',  ( 25.07905384420000061, -92.81180274260000829, 10.93373002890000123 ) ) ;
#20180 = FACE_OUTER_BOUND ( 'NONE', #16714, .T. ) ;
#20181 = VECTOR ( 'NONE', #14713, 1000.000000000000000 ) ;
#20182 = CARTESIAN_POINT ( 'NONE',  ( -11.22677516657805441, -38.85105898695408655, -22.23717618143276198 ) ) ;
#20183 = EDGE_LOOP ( 'NONE', ( #6131, #27193, #17892, #26387 ) ) ;
#20184 = AXIS2_PLACEMENT_3D ( 'NONE', #1437, #5917, #12748 ) ;
#20185 = CARTESIAN_POINT ( 'NONE',  ( -7.323170304809999642, -73.87254094300001839, -39.07240670449999698 ) ) ;
#20186 = CARTESIAN_POINT ( 'NONE',  ( -15.70426946210000096, -100.0012764439999984, -8.839107909470000024 ) ) ;
#20187 = ORIENTED_EDGE ( 'NONE', *, *, #13616, .F. ) ;
#20188 = B_SPLINE_CURVE_WITH_KNOTS ( 'NONE', 5,
 ( #6270, #15135, #21341, #14492, #1263, #26246 ),
 .UNSPECIFIED., .F., .F.,
 ( 6, 6 ),
 ( 0.000000000000000000, 1.000000000000000000 ),
 .UNSPECIFIED. ) ;
#20189 = ORIENTED_EDGE ( 'NONE', *, *, #24723, .T. ) ;
#20190 = DIRECTION ( 'NONE',  ( 0.6710133869769326909, 0.000000000000000000, 0.7414452336469262717 ) ) ;
#20191 = ADVANCED_FACE ( 'NONE', ( #9254 ), #3291, .F. ) ;
#20192 = FACE_OUTER_BOUND ( 'NONE', #10020, .T. ) ;
#20193 = CARTESIAN_POINT ( 'NONE',  ( 20.57577040579999661, -39.36011816900000326, 10.15925981210000018 ) ) ;
#20194 = AXIS2_PLACEMENT_3D ( 'NONE', #13716, #7474, #4681 ) ;
#20195 = LINE ( 'NONE', #26768, #2389 ) ;
#20196 = CARTESIAN_POINT ( 'NONE',  ( 23.42162764450000267, -94.71481161159999829, -6.692249091959999063 ) ) ;
#20197 = CARTESIAN_POINT ( 'NONE',  ( -14.07499735140000041, -74.00781516410000904, 36.22406682180000104 ) ) ;
#20198 = CARTESIAN_POINT ( 'NONE',  ( -32.67688019444538838, -79.98725929158342751, -22.59384834802810360 ) ) ;
#20199 = CARTESIAN_POINT ( 'NONE',  ( -17.54841868506949965, -95.98267023370895856, 13.27123176511321567 ) ) ;
#20200 = ORIENTED_EDGE ( 'NONE', *, *, #12161, .T. ) ;
#20201 = FACE_OUTER_BOUND ( 'NONE', #21761, .T. ) ;
#20202 = DIRECTION ( 'NONE',  ( 0.8775825618903722036, 0.000000000000000000, 0.4794255386042040601 ) ) ;
#20203 = EDGE_CURVE ( 'NONE', #20359, #16528, #15659, .T. ) ;
#20204 = CYLINDRICAL_SURFACE ( 'NONE', #1590, 7.250000000000004441 ) ;
#20205 = CARTESIAN_POINT ( 'NONE',  ( -37.16454418379386482, -63.17361819572786885, 0.3836747633999084695 ) ) ;
#20206 = VERTEX_POINT ( 'NONE', #11285 ) ;
#20207 = AXIS2_PLACEMENT_3D ( 'NONE', #28412, #26093, #1640 ) ;
#20208 = CARTESIAN_POINT ( 'NONE',  ( 26.16626699304385895, -92.92035259805699354, -15.67330046223513307 ) ) ;
#20209 = ORIENTED_EDGE ( 'NONE', *, *, #12776, .F. ) ;
#20210 = DIRECTION ( 'NONE',  ( 1.000000000000000000, 0.000000000000000000, 0.000000000000000000 ) ) ;
#20211 = CARTESIAN_POINT ( 'NONE',  ( 24.39713799250000292, -19.50000027030000282, 1.459766484860000046 ) ) ;
#20212 = CIRCLE ( 'NONE', #7687, 7.250000000000000000 ) ;
#20213 = CARTESIAN_POINT ( 'NONE',  ( 12.03366421969999855, -92.76454730689999906, 27.55075615510000020 ) ) ;
#20214 = ORIENTED_EDGE ( 'NONE', *, *, #24925, .T. ) ;
#20215 = DIRECTION ( 'NONE',  ( 0.000000000000000000, 1.000000000000000000, 0.000000000000000000 ) ) ;
#20216 = VECTOR ( 'NONE', #7961, 1000.000000000000000 ) ;
#20217 = ORIENTED_EDGE ( 'NONE', *, *, #20031, .F. ) ;
#20218 = CARTESIAN_POINT ( 'NONE',  ( -27.15213039292447306, -93.55106866394891085, -0.4309374578557728097 ) ) ;
#20219 = CARTESIAN_POINT ( 'NONE',  ( 20.57006820339999820, -94.36515600330000098, 13.91199895070000103 ) ) ;
#20220 = CARTESIAN_POINT ( 'NONE',  ( 45.84677419350000349, -73.50000000000000000, -4.286925650119999709 ) ) ;
#20221 = EDGE_LOOP ( 'NONE', ( #17989, #17551, #25185, #14708 ) ) ;
#20222 = DIRECTION ( 'NONE',  ( 1.000000000000000000, 0.000000000000000000, 0.000000000000000000 ) ) ;
#20223 = CARTESIAN_POINT ( 'NONE',  ( -22.43272078519999724, -80.50000000000000000, -32.20769377289999369 ) ) ;
#20224 = CIRCLE ( 'NONE', #15080, 34.89999999999999858 ) ;
#20225 = CARTESIAN_POINT ( 'NONE',  ( 8.472394962660001028, -37.95144078849999403, -21.79230209929999873 ) ) ;
#20226 = EDGE_CURVE ( 'NONE', #25155, #19945, #12119, .T. ) ;
#20227 = CARTESIAN_POINT ( 'NONE',  ( -16.31262492385664231, -92.99999871998110734, -23.61087909523048012 ) ) ;
#20228 = DIRECTION ( 'NONE',  ( 0.000000000000000000, 1.000000000000000000, 0.000000000000000000 ) ) ;
#20229 = ORIENTED_EDGE ( 'NONE', *, *, #21146, .T. ) ;
#20230 = EDGE_CURVE ( 'NONE', #26111, #21683, #22887, .T. ) ;
#20231 = FACE_OUTER_BOUND ( 'NONE', #6047, .T. ) ;
#20232 = FACE_OUTER_BOUND ( 'NONE', #7317, .T. ) ;
#20233 = CARTESIAN_POINT ( 'NONE',  ( -40.70731707320000226, -74.50000000000000000, 7.215414233289999757 ) ) ;
#20234 = DIRECTION ( 'NONE',  ( 0.000000000000000000, -1.000000000000000000, 0.000000000000000000 ) ) ;
#20235 = CARTESIAN_POINT ( 'NONE',  ( -7.548138925033555324, -97.11304554415646351, -20.42630931065637867 ) ) ;
#20236 = B_SPLINE_CURVE_WITH_KNOTS ( 'NONE', 5,
 ( #28057, #23268, #21498, #23127, #10259, #3175, #7958, #16562, #25598 ),
 .UNSPECIFIED., .F., .F.,
 ( 6, 3, 6 ),
 ( 0.000000000000000000, 1.237573681330000008, 1.566718891470000097 ),
 .UNSPECIFIED. ) ;
#20237 = CARTESIAN_POINT ( 'NONE',  ( 0.000000000000000000, -102.5000000000000000, 0.000000000000000000 ) ) ;
#20238 = EDGE_CURVE ( 'NONE', #28438, #14549, #10996, .T. ) ;
#20239 = CARTESIAN_POINT ( 'NONE',  ( -46.75000000000000000, -69.00000000000000000, -8.848045483979999792E-16 ) ) ;
#20240 = CARTESIAN_POINT ( 'NONE',  ( -43.20000000000000284, -63.07912966450000880, 0.1732050807559999961 ) ) ;
#20241 = VERTEX_POINT ( 'NONE', #20332 ) ;
#20242 = EDGE_CURVE ( 'NONE', #5855, #19985, #4439, .T. ) ;
#20243 = CARTESIAN_POINT ( 'NONE',  ( -10.77550730630000153, -93.62972879769999679, -23.34803025570000301 ) ) ;
#20244 = VECTOR ( 'NONE', #4552, 1000.000000000000000 ) ;
#20245 = CARTESIAN_POINT ( 'NONE',  ( 7.521517671639999847, -35.00270081890000284, -21.29432416079999868 ) ) ;
#20246 = CARTESIAN_POINT ( 'NONE',  ( -24.25983842336477991, -92.54938211481912447, -18.48561634559768763 ) ) ;
#20247 = CARTESIAN_POINT ( 'NONE',  ( 0.000000000000000000, -29.89689110870000022, 0.000000000000000000 ) ) ;
#20248 = CARTESIAN_POINT ( 'NONE',  ( 46.97084204269999930, -79.78836619429999644, -2.796096378869999732 ) ) ;
#20249 = DIRECTION ( 'NONE',  ( 0.9820818503191364179, -6.938893903907228378E-18, -0.1884548733085491812 ) ) ;
#20250 = AXIS2_PLACEMENT_3D ( 'NONE', #21015, #23745, #10319 ) ;
#20251 = DIRECTION ( 'NONE',  ( 0.000000000000000000, 1.000000000000000000, 0.000000000000000000 ) ) ;
#20252 = ORIENTED_EDGE ( 'NONE', *, *, #364, .F. ) ;
#20253 = CARTESIAN_POINT ( 'NONE',  ( 17.40083768629999739, -99.57131247590000100, 0.8327783396669999894 ) ) ;
#20254 = ORIENTED_EDGE ( 'NONE', *, *, #6207, .F. ) ;
#20255 = CARTESIAN_POINT ( 'NONE',  ( -13.46646228700000059, -101.1889999979999999, -9.098096927170001180 ) ) ;
#20256 = CARTESIAN_POINT ( 'NONE',  ( -21.62384810780000066, -74.29049705580000307, -32.72083640759999668 ) ) ;
#20257 = ORIENTED_EDGE ( 'NONE', *, *, #18999, .F. ) ;
#20258 = LINE ( 'NONE', #24484, #15465 ) ;
#20259 = CARTESIAN_POINT ( 'NONE',  ( 3.798704319269398333, -93.12686943395723915, -28.56536997530774613 ) ) ;
#20260 = DIRECTION ( 'NONE',  ( 0.000000000000000000, 1.000000000000000000, 0.000000000000000000 ) ) ;
#20261 = CARTESIAN_POINT ( 'NONE',  ( 25.72873358008812872, -69.52303041555084917, -8.753713131236221301 ) ) ;
#20262 = CARTESIAN_POINT ( 'NONE',  ( -40.50000000000000000, -65.63577453799999262, -2.309401076760000393 ) ) ;
#20263 = CARTESIAN_POINT ( 'NONE',  ( 21.48482217526310478, -36.89204261257724227, -7.440941901731657815 ) ) ;
#20264 = ORIENTED_EDGE ( 'NONE', *, *, #5891, .F. ) ;
#20265 = EDGE_CURVE ( 'NONE', #27117, #5430, #19539, .T. ) ;
#20266 = CARTESIAN_POINT ( 'NONE',  ( 7.003396616829999921, -92.68584525839999344, -28.68693272650000026 ) ) ;
#20267 = DIRECTION ( 'NONE',  ( 0.000000000000000000, 1.000000000000000000, 0.000000000000000000 ) ) ;
#20268 = B_SPLINE_CURVE_WITH_KNOTS ( 'NONE', 5,
 ( #655, #7335, #16202, #16060, #11682, #3261, #9507, #18410, #27733 ),
 .UNSPECIFIED., .F., .F.,
 ( 6, 3, 6 ),
 ( 0.000000000000000000, 1.376935797170000031, 2.292504252660000130 ),
 .UNSPECIFIED. ) ;
#20269 = CARTESIAN_POINT ( 'NONE',  ( -13.28370414271439870, -92.84927079009484885, 27.45529598729390841 ) ) ;
#20270 = EDGE_LOOP ( 'NONE', ( #26710, #2288, #2931, #19054 ) ) ;
#20271 = CARTESIAN_POINT ( 'NONE',  ( -37.75000000000000000, -63.30468293320000583, -0.7216878364849999006 ) ) ;
#20272 = CARTESIAN_POINT ( 'NONE',  ( -17.14516425180000070, -93.38171818049998762, 19.21619453270000122 ) ) ;
#20273 = CARTESIAN_POINT ( 'NONE',  ( -14.65665268890000128, -79.65629807879999191, 36.94583904750000158 ) ) ;
#20274 = VERTEX_POINT ( 'NONE', #8957 ) ;
#20275 = EDGE_CURVE ( 'NONE', #21532, #13393, #3309, .T. ) ;
#20276 = CARTESIAN_POINT ( 'NONE',  ( -17.74113198119999879, -94.52293239269999958, 16.06143229570000130 ) ) ;
#20277 = CARTESIAN_POINT ( 'NONE',  ( 0.4170640806890000274, -101.3090757639999993, -16.25756418510000145 ) ) ;
#20278 = CARTESIAN_POINT ( 'NONE',  ( 24.24283979073125650, -74.17041889795191878, -30.71041006161582132 ) ) ;
#20279 = CARTESIAN_POINT ( 'NONE',  ( 32.97008108400000026, -74.00000037499999905, -20.36016513680000273 ) ) ;
#20280 = CARTESIAN_POINT ( 'NONE',  ( 22.93659714569999863, -60.39374587409999862, -9.160202142630000210 ) ) ;
#20281 = FACE_BOUND ( 'NONE', #14781, .T. ) ;
#20282 = CARTESIAN_POINT ( 'NONE',  ( -10.42741367090000004, -18.61794786490000320, 18.97192220850000055 ) ) ;
#20283 = VERTEX_POINT ( 'NONE', #27198 ) ;
#20284 = CARTESIAN_POINT ( 'NONE',  ( 27.70978180510000044, -92.50000000000000000, 12.74433177200000067 ) ) ;
#20285 = CARTESIAN_POINT ( 'NONE',  ( -42.40756524499999358, -65.56519245710001087, 0.6307174998540000521 ) ) ;
#20286 = CARTESIAN_POINT ( 'NONE',  ( 19.94074162929999972, -94.89420189139998740, 14.19047635519999950 ) ) ;
#20287 = AXIS2_PLACEMENT_3D ( 'NONE', #13418, #11061, #13123 ) ;
#20288 = CARTESIAN_POINT ( 'NONE',  ( 7.367397733560000717, -74.05254684259999465, 39.49475000900000765 ) ) ;
#20289 = CARTESIAN_POINT ( 'NONE',  ( -32.77174707999999725, -79.50000000000000000, -21.60034937969999902 ) ) ;
#20290 = CARTESIAN_POINT ( 'NONE',  ( -42.25000000000000000, -65.00000000000000000, -0.7216878364880000563 ) ) ;
#20291 = CARTESIAN_POINT ( 'NONE',  ( 20.14104788939999935, -35.73233869100000248, -9.018304108959998899 ) ) ;
#20292 = CARTESIAN_POINT ( 'NONE',  ( -7.122560077160000169, -101.2063419769999939, 14.31247113230000068 ) ) ;
#20293 = ORIENTED_EDGE ( 'NONE', *, *, #24623, .F. ) ;
#20294 = DIRECTION ( 'NONE',  ( 0.000000000000000000, -1.000000000000000000, 0.000000000000000000 ) ) ;
#20295 = CARTESIAN_POINT ( 'NONE',  ( 7.854008167109999938, -37.08875413240000540, -21.51812330200000289 ) ) ;
#20296 = CARTESIAN_POINT ( 'NONE',  ( 7.610177731959999470, -101.4231532209999926, 14.04048934709999941 ) ) ;
#20297 = EDGE_CURVE ( 'NONE', #3752, #20553, #7001, .T. ) ;
#20298 = CARTESIAN_POINT ( 'NONE',  ( -0.6881950023909999548, -101.1848541609999899, -15.26655981750000102 ) ) ;
#20299 = B_SPLINE_CURVE_WITH_KNOTS ( 'NONE', 5,
 ( #15562, #19793, #11180, #26362, #10590, #15411, #13378, #19648, #24467 ),
 .UNSPECIFIED., .F., .F.,
 ( 6, 3, 6 ),
 ( 0.000000000000000000, 0.5000000000000000000, 1.000000000000000000 ),
 .UNSPECIFIED. ) ;
#20300 = CARTESIAN_POINT ( 'NONE',  ( -36.79999999999999716, -63.07912966450000880, -0.1732050807570000017 ) ) ;
#20301 = CARTESIAN_POINT ( 'NONE',  ( -7.498698696109999062, -94.79581469870001342, -22.45487717610000189 ) ) ;
#20302 = CARTESIAN_POINT ( 'NONE',  ( -14.62247892739999955, -90.50000000000000000, -26.76626813769999913 ) ) ;
#20303 = DIRECTION ( 'NONE',  ( 0.7071067811865475727, 0.000000000000000000, -0.7071067811865475727 ) ) ;
#20304 = CARTESIAN_POINT ( 'NONE',  ( -7.120447010050000358, -101.1889999979999999, 15.21641332169999927 ) ) ;
#20305 = CARTESIAN_POINT ( 'NONE',  ( 13.00155415721168772, -96.26579376197079796, 17.29370665404819718 ) ) ;
#20306 = DIRECTION ( 'NONE',  ( 0.1708373792999889895, 0.000000000000000000, 0.9852992387259372764 ) ) ;
#20307 = FACE_OUTER_BOUND ( 'NONE', #21969, .T. ) ;
#20308 = CARTESIAN_POINT ( 'NONE',  ( 24.01307781190000057, -93.00000000000000000, -18.61462211579999959 ) ) ;
#20309 = CIRCLE ( 'NONE', #13795, 55.67692378859999991 ) ;
#20310 = CARTESIAN_POINT ( 'NONE',  ( 0.000000000000000000, -18.50000000000000000, 0.000000000000000000 ) ) ;
#20311 = ORIENTED_EDGE ( 'NONE', *, *, #25728, .F. ) ;
#20312 = CARTESIAN_POINT ( 'NONE',  ( 36.28164458730000064, -74.50000000000000000, -14.97346873770000109 ) ) ;
#20313 = CARTESIAN_POINT ( 'NONE',  ( 7.790027027709999885, -101.0397073060000110, 13.52566268780000058 ) ) ;
#20314 = VERTEX_POINT ( 'NONE', #2432 ) ;
#20315 = DIRECTION ( 'NONE',  ( 1.000000000000000000, 0.000000000000000000, 0.000000000000000000 ) ) ;
#20316 = ADVANCED_FACE ( 'NONE', ( #20192 ), #17703, .T. ) ;
#20317 = CARTESIAN_POINT ( 'NONE',  ( -13.49470405399999962, -57.43018220239999749, 20.74700755119999585 ) ) ;
#20318 = CARTESIAN_POINT ( 'NONE',  ( 19.97576656849999921, -74.00000000000000000, -19.97576656849999921 ) ) ;
#20319 = CARTESIAN_POINT ( 'NONE',  ( 28.54521250490000028, -92.50425970539998843, 7.633765891700000417 ) ) ;
#20320 = CARTESIAN_POINT ( 'NONE',  ( 21.64960747819999654, -36.72219091790000078, -8.748808738199999269 ) ) ;
#20321 = DIRECTION ( 'NONE',  ( -2.784231178940000568E-16, 0.000000000000000000, 1.000000000000000000 ) ) ;
#20322 = CARTESIAN_POINT ( 'NONE',  ( 16.25689483720000084, -99.97545561319999763, 4.618077352500000288 ) ) ;
#20323 = VERTEX_POINT ( 'NONE', #26906 ) ;
#20324 = CARTESIAN_POINT ( 'NONE',  ( -7.248115120159999591, -74.24284936579999794, -40.37845838710000379 ) ) ;
#20325 = CARTESIAN_POINT ( 'NONE',  ( 30.43430859973134162, -74.20053182656846502, -24.62761277945777749 ) ) ;
#20326 = CARTESIAN_POINT ( 'NONE',  ( -20.19463108470000279, -97.41042626780000546, -7.251312267670000367 ) ) ;
#20327 = EDGE_LOOP ( 'NONE', ( #6670, #12188, #15085, #13841 ) ) ;
#20328 = CARTESIAN_POINT ( 'NONE',  ( -30.48054257754459329, -92.53708507728566701, 1.089948664374644105 ) ) ;
#20329 = EDGE_LOOP ( 'NONE', ( #878, #3529, #23070, #7855 ) ) ;
#20330 = EDGE_CURVE ( 'NONE', #12823, #1234, #23286, .T. ) ;
#20331 = CARTESIAN_POINT ( 'NONE',  ( 0.000000000000000000, -90.50000000000000000, 0.000000000000000000 ) ) ;
#20332 = CARTESIAN_POINT ( 'NONE',  ( -3.355978770230000130, -90.50000000000000000, -6.143077933229999843 ) ) ;
#20333 = CARTESIAN_POINT ( 'NONE',  ( -7.333297298759998917, -94.59276292389999696, -22.63874378639999563 ) ) ;
#20334 = DIRECTION ( 'NONE',  ( -2.739037067331800130E-16, 0.000000000000000000, 1.000000000000000000 ) ) ;
#20335 = CARTESIAN_POINT ( 'NONE',  ( -7.224658177536289472, -73.64797963450716622, -39.39373284330162051 ) ) ;
#20336 = ADVANCED_FACE ( 'NONE', ( #16834 ), #3163, .T. ) ;
#20337 = CARTESIAN_POINT ( 'NONE',  ( 19.02471330030000018, -18.50000000000000000, 9.686045925820002012 ) ) ;
#20338 = CARTESIAN_POINT ( 'NONE',  ( -41.74999999999999289, -65.11310065233230659, 2.760503925682381343 ) ) ;
#20339 = FACE_OUTER_BOUND ( 'NONE', #2804, .T. ) ;
#20340 = B_SPLINE_SURFACE_WITH_KNOTS ( 'NONE', 5, 5, ( 
 ( #12861, #17118, #4438, #10528, #28474, #20018 ),
 ( #4143, #28331, #2259, #11105, #6185, #8788 ),
 ( #15057, #26007, #6031, #2124, #23822, #26307 ),
 ( #17416, #13016, #1977, #22076, #17700, #23967 ),
 ( #28618, #19730, #3864, #10959, #26588, #8650 ),
 ( #6630, #17552, #6477, #19588, #26444, #19868 ) ),
 .UNSPECIFIED., .F., .F., .F.,
 ( 6, 6 ),
 ( 6, 6 ),
 ( 0.000000000000000000, 2.292504252660000130 ),
 ( 0.000000000000000000, 1.000000000000000000 ),
 .UNSPECIFIED. ) ;
#20341 = ORIENTED_EDGE ( 'NONE', *, *, #6545, .F. ) ;
#20342 = ADVANCED_FACE ( 'NONE', ( #20934 ), #22365, .F. ) ;
#20343 = B_SPLINE_CURVE_WITH_KNOTS ( 'NONE', 5,
 ( #17311, #19484, #17026, #17860, #8406, #24007, #6937, #26757, #26204 ),
 .UNSPECIFIED., .F., .F.,
 ( 6, 3, 6 ),
 ( 0.000000000000000000, 0.6992167742671963060, 1.000000000000000000 ),
 .UNSPECIFIED. ) ;
#20344 = CARTESIAN_POINT ( 'NONE',  ( -12.95441099080000136, -72.29970937929999764, -25.32226104859999793 ) ) ;
#20345 = CARTESIAN_POINT ( 'NONE',  ( -3.183996595813977315, -98.12113812247983446, 20.16279650972818871 ) ) ;
#20346 = CARTESIAN_POINT ( 'NONE',  ( -13.30220213780000016, -99.88067631459999518, -11.12664376240000053 ) ) ;
#20347 = CARTESIAN_POINT ( 'NONE',  ( -12.41793182790000039, -101.2530993039999885, -8.757551688899999576 ) ) ;
#20348 = CARTESIAN_POINT ( 'NONE',  ( 22.75761901743981142, -61.36591909834531577, -7.240633913292683133 ) ) ;
#20349 = ORIENTED_EDGE ( 'NONE', *, *, #25228, .T. ) ;
#20350 = CIRCLE ( 'NONE', #11982, 7.000000000000000000 ) ;
#20351 = CARTESIAN_POINT ( 'NONE',  ( 26.59508290546112264, -92.69183043814645373, -14.93184108318626357 ) ) ;
#20352 = ORIENTED_EDGE ( 'NONE', *, *, #357, .F. ) ;
#20353 = ADVANCED_FACE ( 'NONE', ( #10103 ), #3437, .F. ) ;
#20354 = CARTESIAN_POINT ( 'NONE',  ( -4.500000000000000000, -15.00000000000000000, -40.50000000000000000 ) ) ;
#20355 = EDGE_CURVE ( 'NONE', #13019, #25027, #26537, .T. ) ;
#20356 = VECTOR ( 'NONE', #18130, 1000.000000000000000 ) ;
#20357 = CARTESIAN_POINT ( 'NONE',  ( 1.563021348000000144, -94.54719592040000009, 23.80457129850000086 ) ) ;
#20358 = CARTESIAN_POINT ( 'NONE',  ( 4.026022453159999515, -93.52727151969999397, 25.97757116140000022 ) ) ;
#20359 = VERTEX_POINT ( 'NONE', #8083 ) ;
#20360 = EDGE_LOOP ( 'NONE', ( #24491, #21962, #6821, #20418 ) ) ;
#20361 = DIRECTION ( 'NONE',  ( 0.000000000000000000, 1.000000000000000000, 0.000000000000000000 ) ) ;
#20362 = FACE_OUTER_BOUND ( 'NONE', #18487, .T. ) ;
#20363 = CARTESIAN_POINT ( 'NONE',  ( 19.97576656849999921, -36.00000000000000000, -19.97576656849999921 ) ) ;
#20364 = EDGE_CURVE ( 'NONE', #25380, #7420, #14843, .T. ) ;
#20365 = ORIENTED_EDGE ( 'NONE', *, *, #13809, .T. ) ;
#20366 = DIRECTION ( 'NONE',  ( -0.4151946956541399669, 0.5000000000001689759, -0.7600087925152558821 ) ) ;
#20367 = CARTESIAN_POINT ( 'NONE',  ( -22.41677045990000394, -79.93903203729999518, -32.75734019789999962 ) ) ;
#20368 = TOROIDAL_SURFACE ( 'NONE', #6395, 15.50000000000000000, 0.5000000000000000000 ) ;
#20369 = CARTESIAN_POINT ( 'NONE',  ( 9.476129726560001743, -36.00000000000000000, -20.06309461059999677 ) ) ;
#20370 = CARTESIAN_POINT ( 'NONE',  ( -11.85289062220000034, -94.98812477599999227, -21.44324726179999985 ) ) ;
#20371 = DIRECTION ( 'NONE',  ( 0.000000000000000000, 1.000000000000000000, 0.000000000000000000 ) ) ;
#20372 = EDGE_LOOP ( 'NONE', ( #9602, #7350, #13141, #18179 ) ) ;
#20373 = CARTESIAN_POINT ( 'NONE',  ( -22.27191869549999836, -94.59276292389999696, -8.381623179300000004 ) ) ;
#20374 = FACE_OUTER_BOUND ( 'NONE', #21718, .T. ) ;
#20375 = CARTESIAN_POINT ( 'NONE',  ( -40.70731707320000226, -74.50000000000000000, 7.215414233289999757 ) ) ;
#20376 = CARTESIAN_POINT ( 'NONE',  ( -22.21587842519999967, -74.29049705580000307, -32.78062842099999585 ) ) ;
#20377 = ORIENTED_EDGE ( 'NONE', *, *, #7560, .F. ) ;
#20378 = CIRCLE ( 'NONE', #14783, 38.75000000000000000 ) ;
#20379 = CARTESIAN_POINT ( 'NONE',  ( -19.20882542639999713, -32.73217875690000511, 11.71052916729999893 ) ) ;
#20380 = CARTESIAN_POINT ( 'NONE',  ( 1.131980963049999955, -100.1275643909999928, -16.60892386949999988 ) ) ;
#20381 = CARTESIAN_POINT ( 'NONE',  ( -19.01889177740000036, -19.17414499179999865, 13.97303501010000026 ) ) ;
#20382 = ORIENTED_EDGE ( 'NONE', *, *, #14568, .T. ) ;
#20383 = DIRECTION ( 'NONE',  ( 0.000000000000000000, 1.000000000000000000, 0.000000000000000000 ) ) ;
#20384 = CARTESIAN_POINT ( 'NONE',  ( 23.67625467909999770, -63.41849336990000552, 10.62412784700000046 ) ) ;
#20385 = CARTESIAN_POINT ( 'NONE',  ( 8.805019338579999300, -34.63244828799999908, -20.36793968349999773 ) ) ;
#20386 = CARTESIAN_POINT ( 'NONE',  ( 16.09612372445523931, -100.8061861225251477, 4.288648819865870543 ) ) ;
#20387 = DIRECTION ( 'NONE',  ( 1.000000000000000000, 0.000000000000000000, 0.000000000000000000 ) ) ;
#20388 = EDGE_LOOP ( 'NONE', ( #26420, #273, #11053, #19297 ) ) ;
#20389 = CARTESIAN_POINT ( 'NONE',  ( 46.88136687659999779, -79.93788011300000562, -2.717859463149999488 ) ) ;
#20390 = CARTESIAN_POINT ( 'NONE',  ( 10.50000000000000000, -19.00000000000000000, -5.828670879280000091E-16 ) ) ;
#20391 = CIRCLE ( 'NONE', #10587, 32.39999999999999858 ) ;
#20392 = CARTESIAN_POINT ( 'NONE',  ( -13.16836258200000209, -18.50000000000000000, 18.78571244450000322 ) ) ;
#20393 = CARTESIAN_POINT ( 'NONE',  ( -11.45927840279999899, -61.83365245859999959, -22.14359330659999969 ) ) ;
#20394 = ADVANCED_FACE ( 'NONE', ( #3300 ), #3394, .T. ) ;
#20395 = CARTESIAN_POINT ( 'NONE',  ( 26.52608433400000010, -70.67711320560000843, -11.10241135090000064 ) ) ;
#20396 = CARTESIAN_POINT ( 'NONE',  ( 4.243840698532188149, -93.86127438317009819, 26.03392588043698908 ) ) ;
#20397 = EDGE_CURVE ( 'NONE', #14954, #3210, #13017, .T. ) ;
#20398 = ORIENTED_EDGE ( 'NONE', *, *, #2892, .F. ) ;
#20399 = CARTESIAN_POINT ( 'NONE',  ( -35.88566914520000495, -74.50000000000000000, -26.69328098980000163 ) ) ;
#20400 = ORIENTED_EDGE ( 'NONE', *, *, #27187, .T. ) ;
#20401 = PRODUCT_DEFINITION_FORMATION_WITH_SPECIFIED_SOURCE ( 'ANY', '', #2252, .NOT_KNOWN. ) ;
#20402 = CARTESIAN_POINT ( 'NONE',  ( 23.03829042120000281, -52.56313962710000709, 10.32398954119999956 ) ) ;
#20403 = CARTESIAN_POINT ( 'NONE',  ( -21.60034937969999902, -74.50000000000000000, -32.77174707999999725 ) ) ;
#20404 = ADVANCED_FACE ( 'NONE', ( #2112 ), #10661, .T. ) ;
#20405 = ORIENTED_EDGE ( 'NONE', *, *, #13761, .F. ) ;
#20406 = CARTESIAN_POINT ( 'NONE',  ( 1.678657213230000024E-14, -74.00000000000000000, 7.838174553849999450E-15 ) ) ;
#20407 = EDGE_CURVE ( 'NONE', #4784, #12424, #7933, .T. ) ;
#20408 = CARTESIAN_POINT ( 'NONE',  ( 3.331242539846007933, -93.08996811584388809, -28.87175727731148811 ) ) ;
#20409 = CARTESIAN_POINT ( 'NONE',  ( -28.91420642530000151, -92.51331408429999215, 5.051166948289999681 ) ) ;
#20410 = CARTESIAN_POINT ( 'NONE',  ( -17.97710455780000061, -98.83662759129998676, 4.969895303470000414 ) ) ;
#20411 = CARTESIAN_POINT ( 'NONE',  ( 17.05053095294056575, -99.82487967928406647, 0.9399568373772333452 ) ) ;
#20412 = CARTESIAN_POINT ( 'NONE',  ( 21.59890840851629079, -37.78281444658050958, -8.035513333422169779 ) ) ;
#20413 = ORIENTED_EDGE ( 'NONE', *, *, #1987, .F. ) ;
#20414 = CIRCLE ( 'NONE', #3663, 20.64285714290000229 ) ;
#20415 = CARTESIAN_POINT ( 'NONE',  ( 11.30811551740000098, -93.49005502370000897, -23.61965843710000001 ) ) ;
#20416 = CARTESIAN_POINT ( 'NONE',  ( -38.06767232176576954, -65.74137084432105382, -1.010180990337120832 ) ) ;
#20417 = CARTESIAN_POINT ( 'NONE',  ( -31.99064106590000023, -74.00000000000000000, -21.95840602359999849 ) ) ;
#20418 = ORIENTED_EDGE ( 'NONE', *, *, #3689, .F. ) ;
#20419 = CARTESIAN_POINT ( 'NONE',  ( 3.835404308829999831, -1.000000000000000000, 7.020660495120000455 ) ) ;
#20420 = DIRECTION ( 'NONE',  ( 0.000000000000000000, 1.000000000000000000, 0.000000000000000000 ) ) ;
#20421 = CARTESIAN_POINT ( 'NONE',  ( 7.312846564840000063, -92.50000000000000000, 29.61034067890000188 ) ) ;
#20422 = VERTEX_POINT ( 'NONE', #12572 ) ;
#20423 = CARTESIAN_POINT ( 'NONE',  ( -18.27191206690000058, -94.89419905399999777, 16.28310417119999798 ) ) ;
#20424 = DIRECTION ( 'NONE',  ( 0.000000000000000000, 1.000000000000000000, 0.000000000000000000 ) ) ;
#20425 = CARTESIAN_POINT ( 'NONE',  ( 7.356933064080000584, -36.56811125840000187, -21.47791245320000186 ) ) ;
#20426 = DIRECTION ( 'NONE',  ( 1.000000000000000000, 0.000000000000000000, 0.000000000000000000 ) ) ;
#20427 = CARTESIAN_POINT ( 'NONE',  ( -14.76448906705501862, -74.23471952222740811, 36.28496449933966517 ) ) ;
#20428 = CARTESIAN_POINT ( 'NONE',  ( 26.28708038020000259, -67.57003242129999876, 0.4743469720099999787 ) ) ;
#20429 = CARTESIAN_POINT ( 'NONE',  ( 8.125631349740000786, -92.50000000000000000, 24.17072847820000092 ) ) ;
#20430 = TOROIDAL_SURFACE ( 'NONE', #26474, 6.750000000000000000, 0.5000000000000000000 ) ;
#20431 = CARTESIAN_POINT ( 'NONE',  ( -7.713029007999999465, -80.00000000000000000, 40.75609756099999714 ) ) ;
#20433 = EDGE_CURVE ( 'NONE', #10833, #16440, #13982, .T. ) ;
#20432 = AXIS2_PLACEMENT_3D ( 'NONE', #5756, #6024, #15046 ) ;
#20434 = CIRCLE ( 'NONE', #2744, 0.4999999999999985567 ) ;
#20435 = EDGE_LOOP ( 'NONE', ( #9928, #21875, #8197, #1632 ) ) ;
#20436 = CARTESIAN_POINT ( 'NONE',  ( 9.926410842420001046, -36.18196426709999969, -21.60058389869999829 ) ) ;
#20437 = DIRECTION ( 'NONE',  ( 0.000000000000000000, 1.000000000000000000, 0.000000000000000000 ) ) ;
#20438 = VECTOR ( 'NONE', #23875, 1000.000000000000000 ) ;
#20439 = CARTESIAN_POINT ( 'NONE',  ( 10.31391047600000022, -100.0012789650000116, 14.77758590519999871 ) ) ;
#20440 = VERTEX_POINT ( 'NONE', #24090 ) ;
#20441 = CARTESIAN_POINT ( 'NONE',  ( 36.47289904669996474, -79.00000000000000000, -14.78463635570000001 ) ) ;
#20442 = DIRECTION ( 'NONE',  ( 1.000000000000000000, 0.000000000000000000, 0.000000000000000000 ) ) ;
#20443 = ADVANCED_FACE ( 'NONE', ( #19576 ), #12559, .F. ) ;
#20444 = LINE ( 'NONE', #13880, #9314 ) ;
#20445 = CARTESIAN_POINT ( 'NONE',  ( 27.02159208476454566, -72.26331251235005482, -11.39394181573582188 ) ) ;
#20446 = CARTESIAN_POINT ( 'NONE',  ( -12.45041691581901411, -101.4241070620317657, -10.32313517531819791 ) ) ;
#20447 = CARTESIAN_POINT ( 'NONE',  ( 8.090026142010000143, -37.42980753870000399, -21.59874174039999772 ) ) ;
#20448 = FACE_OUTER_BOUND ( 'NONE', #26491, .T. ) ;
#20449 = ORIENTED_EDGE ( 'NONE', *, *, #27784, .T. ) ;
#20450 = CARTESIAN_POINT ( 'NONE',  ( -0.7085401579220000912, -101.1716782170000073, -15.71788616779999970 ) ) ;
#20451 = CARTESIAN_POINT ( 'NONE',  ( -40.50000000000000000, -15.00000000000000000, -4.500000000000000000 ) ) ;
#20452 = CARTESIAN_POINT ( 'NONE',  ( 21.51316594792547576, -36.56981903696397751, -7.049162187537676871 ) ) ;
#20453 = CIRCLE ( 'NONE', #6482, 10.50000000000000000 ) ;
#20454 = DIRECTION ( 'NONE',  ( 0.000000000000000000, -1.000000000000000000, 0.000000000000000000 ) ) ;
#20455 = CARTESIAN_POINT ( 'NONE',  ( -14.94260916130000005, -100.8733989949999881, 4.897671729189999823 ) ) ;
#20456 = FACE_OUTER_BOUND ( 'NONE', #24799, .T. ) ;
#20457 = CARTESIAN_POINT ( 'NONE',  ( 0.000000000000000000, -30.50310889129999836, 0.000000000000000000 ) ) ;
#20458 = AXIS2_PLACEMENT_3D ( 'NONE', #16089, #18442, #27328 ) ;
#20459 = CIRCLE ( 'NONE', #24165, 2.000000000000000888 ) ;
#20460 = DIRECTION ( 'NONE',  ( 0.000000000000000000, -1.000000000000000000, 0.000000000000000000 ) ) ;
#20461 = CARTESIAN_POINT ( 'NONE',  ( 0.000000000000000000, -39.50000000000000000, 0.000000000000000000 ) ) ;
#20462 = DIRECTION ( 'NONE',  ( 1.000000000000000000, 0.000000000000000000, 0.000000000000000000 ) ) ;
#20463 = DIRECTION ( 'NONE',  ( 1.000000000000000000, 0.000000000000000000, 0.000000000000000000 ) ) ;
#20464 = DIRECTION ( 'NONE',  ( -0.2414462220490755373, 0.000000000000000000, 0.9704142011833032377 ) ) ;
#20465 = ORIENTED_EDGE ( 'NONE', *, *, #25458, .F. ) ;
#20466 = CARTESIAN_POINT ( 'NONE',  ( -32.51056936577126066, -80.00000002169532820, -22.64367424041782684 ) ) ;
#20467 = CARTESIAN_POINT ( 'NONE',  ( -22.22906643738334154, -79.56075417968409624, -32.83566815571666098 ) ) ;
#20468 = EDGE_CURVE ( 'NONE', #1165, #19506, #3740, .T. ) ;
#20469 = CARTESIAN_POINT ( 'NONE',  ( -12.07107500047315263, -68.72948970806329783, -25.24773251016443965 ) ) ;
#20470 = CARTESIAN_POINT ( 'NONE',  ( -13.89821210610000080, -61.67838661550000268, 21.35051843089999934 ) ) ;
#20471 = CARTESIAN_POINT ( 'NONE',  ( 10.50000000000000000, -18.50000000000000000, 0.000000000000000000 ) ) ;
#20472 = CARTESIAN_POINT ( 'NONE',  ( 26.30230850345395766, -72.70510570382117521, 11.30503913471621935 ) ) ;
#20473 = CARTESIAN_POINT ( 'NONE',  ( 19.35995903480842983, -19.20927481205639964, 10.50154324412826412 ) ) ;
#20474 = CARTESIAN_POINT ( 'NONE',  ( -19.93842487378145378, -95.91648618845204055, 9.502657547810732908 ) ) ;
#20475 = AXIS2_PLACEMENT_3D ( 'NONE', #18375, #13992, #6859 ) ;
#20476 = EDGE_CURVE ( 'NONE', #14401, #20122, #7498, .T. ) ;
#20477 = AXIS2_PLACEMENT_3D ( 'NONE', #20901, #11851, #25129 ) ;
#20478 = CARTESIAN_POINT ( 'NONE',  ( -11.03619930328196297, -25.78856419394296040, -21.97741589576630616 ) ) ;
#20479 = EDGE_LOOP ( 'NONE', ( #12890, #7298, #22006, #9579 ) ) ;
#20480 = CARTESIAN_POINT ( 'NONE',  ( 29.13907669020199265, -74.34630382065689957, -26.26003855043551738 ) ) ;
#20481 = CARTESIAN_POINT ( 'NONE',  ( -21.69992076209999965, -95.77248565549999171, -5.387565530199999841 ) ) ;
#20482 = ORIENTED_EDGE ( 'NONE', *, *, #20397, .T. ) ;
#20483 = CARTESIAN_POINT ( 'NONE',  ( 8.732396249151028300, -92.71525149955749612, 29.22337735326396313 ) ) ;
#20484 = CARTESIAN_POINT ( 'NONE',  ( 26.89647983300000078, -10.52212389379999991, 49.23367609159999603 ) ) ;
#20485 = CARTESIAN_POINT ( 'NONE',  ( -5.873292863139999653, -11.55246854740000018, -10.75099047199999980 ) ) ;
#20486 = CARTESIAN_POINT ( 'NONE',  ( -40.76878914953984179, -63.24880261862722364, -2.464586564602152752 ) ) ;
#20487 = CARTESIAN_POINT ( 'NONE',  ( -11.90443957499999961, -64.24504445130001784, -23.68393584109999850 ) ) ;
#20488 = CARTESIAN_POINT ( 'NONE',  ( -7.198125313996778907, -73.54003775238706453, -39.10791602294204239 ) ) ;
#20489 = CARTESIAN_POINT ( 'NONE',  ( 20.22453322670000020, -19.46723765599999822, 9.600718987880000554 ) ) ;
#20490 = CARTESIAN_POINT ( 'NONE',  ( -24.63993737860000266, -74.00000000000000000, 17.98210258840000009 ) ) ;
#20491 = CARTESIAN_POINT ( 'NONE',  ( 14.12869155539999966, -98.65110728930000050, -12.17622016660000028 ) ) ;
#20492 = ORIENTED_EDGE ( 'NONE', *, *, #20842, .F. ) ;
#20493 = CARTESIAN_POINT ( 'NONE',  ( -13.13779125880000009, -70.67790319679998845, -24.39064998879999635 ) ) ;
#20494 = CARTESIAN_POINT ( 'NONE',  ( -4.178487457639150193, -99.07183862851897516, 18.71548091470333830 ) ) ;
#20495 = CARTESIAN_POINT ( 'NONE',  ( 7.867248475934297325, -101.5674482532140956, 14.00205404261702569 ) ) ;
#20496 = CARTESIAN_POINT ( 'NONE',  ( 0.000000000000000000, -101.1889999979999999, 0.000000000000000000 ) ) ;
#20497 = CARTESIAN_POINT ( 'NONE',  ( -39.04162410960000074, -73.95638562449998687, -7.432628554119999897 ) ) ;
#20498 = ORIENTED_EDGE ( 'NONE', *, *, #23244, .T. ) ;
#20499 = CIRCLE ( 'NONE', #13985, 4.999999999999997335 ) ;
#20500 = CIRCLE ( 'NONE', #11164, 7.000000000000000000 ) ;
#20501 = CARTESIAN_POINT ( 'NONE',  ( 26.54754530181849859, -92.71525149907830610, -15.01627006387875696 ) ) ;
#20502 = ORIENTED_EDGE ( 'NONE', *, *, #5663, .T. ) ;
#20503 = EDGE_CURVE ( 'NONE', #22004, #24058, #8548, .T. ) ;
#20504 = ADVANCED_FACE ( 'NONE', ( #15177 ), #5172, .F. ) ;
#20505 = DIRECTION ( 'NONE',  ( 0.4794255386042040601, 0.000000000000000000, 0.8775825618903720926 ) ) ;
#20506 = CARTESIAN_POINT ( 'NONE',  ( 1.631254085230000150, -94.59276583650000703, 23.74088304550000217 ) ) ;
#20507 = CARTESIAN_POINT ( 'NONE',  ( 10.51495134820000033, -92.53777738559999477, 27.19433521669999720 ) ) ;
#20508 = ORIENTED_EDGE ( 'NONE', *, *, #18023, .F. ) ;
#20509 = CARTESIAN_POINT ( 'NONE',  ( -5.298192075760000286, -100.9197081840000010, 14.69882727599999939 ) ) ;
#20510 = ORIENTED_EDGE ( 'NONE', *, *, #10054, .F. ) ;
#20511 = CARTESIAN_POINT ( 'NONE',  ( -24.15516222759999820, -94.98812477599999227, -4.102682929219999330 ) ) ;
#20512 = CARTESIAN_POINT ( 'NONE',  ( 3.787197165510000296, -111.0000000000000000, -30.26395773239999798 ) ) ;
#20513 = CARTESIAN_POINT ( 'NONE',  ( 47.15182475600000345, -74.55832059870000705, -1.380511777149999952 ) ) ;
#20514 = ORIENTED_EDGE ( 'NONE', *, *, #7665, .F. ) ;
#20515 = CIRCLE ( 'NONE', #18184, 7.750000000000000000 ) ;
#20516 = CARTESIAN_POINT ( 'NONE',  ( 7.188997797770536380, -73.53996501802382113, -39.06010443590120218 ) ) ;
#20517 = CARTESIAN_POINT ( 'NONE',  ( 23.14416696340000001, -57.40875702419999982, 10.37855830930000067 ) ) ;
#20518 = VECTOR ( 'NONE', #2189, 1000.000000000000000 ) ;
#20519 = ORIENTED_EDGE ( 'NONE', *, *, #20740, .F. ) ;
#20520 = VECTOR ( 'NONE', #22693, 1000.000000000000114 ) ;
#20521 = CARTESIAN_POINT ( 'NONE',  ( 34.89999999999999858, -82.50000000000000000, 4.273876174839999917E-15 ) ) ;
#20522 = DIRECTION ( 'NONE',  ( 1.000000000000000000, 0.000000000000000000, 0.000000000000000000 ) ) ;
#20523 = CARTESIAN_POINT ( 'NONE',  ( -2.994983700900000212, -67.58705842039999823, -26.99846661069999953 ) ) ;
#20524 = CARTESIAN_POINT ( 'NONE',  ( -16.85275212700000225, -72.18744872199999918, 23.44936106520000152 ) ) ;
#20525 = ORIENTED_EDGE ( 'NONE', *, *, #16181, .F. ) ;
#20526 = DIRECTION ( 'NONE',  ( 0.4794255386042036715, 0.000000000000000000, 0.8775825618903723147 ) ) ;
#20527 = CARTESIAN_POINT ( 'NONE',  ( -16.86580049039999807, -99.83341253780000102, 3.169051538790000233 ) ) ;
#20528 = CARTESIAN_POINT ( 'NONE',  ( 25.19716909789999804, -60.27227161350000273, 1.367805385619999869 ) ) ;
#20529 = CARTESIAN_POINT ( 'NONE',  ( -21.83908241200000333, -74.03505044649999434, -32.25228936610000119 ) ) ;
#20530 = ORIENTED_EDGE ( 'NONE', *, *, #3226, .T. ) ;
#20531 = CARTESIAN_POINT ( 'NONE',  ( -36.23922253580000330, -74.00000000000000000, -27.04683438039999999 ) ) ;
#20532 = CARTESIAN_POINT ( 'NONE',  ( 0.7792231278100000269, -100.9137139110000021, -15.61347424839999931 ) ) ;
#20533 = DIRECTION ( 'NONE',  ( 0.000000000000000000, -1.000000000000000000, 0.000000000000000000 ) ) ;
#20534 = EDGE_LOOP ( 'NONE', ( #18694, #15105, #3747, #25692 ) ) ;
#20535 = CARTESIAN_POINT ( 'NONE',  ( -10.63275893859999854, -93.28923078690000636, -23.66443698309999633 ) ) ;
#20536 = CARTESIAN_POINT ( 'NONE',  ( -27.18988201479999844, -27.50155444569999830, -49.77074518290000071 ) ) ;
#20537 = CARTESIAN_POINT ( 'NONE',  ( 7.573069789530000762, -34.86444500489999854, -21.26629628179999898 ) ) ;
#20538 = CARTESIAN_POINT ( 'NONE',  ( 16.54913656973435110, -100.2392017793862209, 4.346239228624037665 ) ) ;
#20539 = CARTESIAN_POINT ( 'NONE',  ( 2.876553231629999985, -108.5000000000000000, 5.265495371340000119 ) ) ;
#20540 = VERTEX_POINT ( 'NONE', #26574 ) ;
#20541 = CARTESIAN_POINT ( 'NONE',  ( 47.25000000000000000, -79.00000000000000000, -7.713829575100000215E-13 ) ) ;
#20542 = CIRCLE ( 'NONE', #3348, 7.750000000000000000 ) ;
#20543 = DIRECTION ( 'NONE',  ( 0.000000000000000000, -1.000000000000000000, 0.000000000000000000 ) ) ;
#20544 = VECTOR ( 'NONE', #7598, 1000.000000000000000 ) ;
#20545 = CIRCLE ( 'NONE', #9359, 57.75000000000000000 ) ;
#20546 = UNCERTAINTY_MEASURE_WITH_UNIT (LENGTH_MEASURE( 1.000000000000000082E-05 ), #25669, 'distance_accuracy_value', 'NONE');
#20547 = ITEM_DEFINED_TRANSFORMATION ( 'NONE', 'NONE', #25074,  #26433 ) ;
#20548 = CARTESIAN_POINT ( 'NONE',  ( -11.25020521769999959, -58.97460807019999862, -21.16435021079999856 ) ) ;
#20549 = CARTESIAN_POINT ( 'NONE',  ( 23.74273760109999998, -65.04364753569998925, -8.271557007380000215 ) ) ;
#20550 = CARTESIAN_POINT ( 'NONE',  ( 5.383412395290363861, -93.59823626961022569, 26.48305322804162643 ) ) ;
#20551 = ORIENTED_EDGE ( 'NONE', *, *, #16680, .T. ) ;
#20552 = CARTESIAN_POINT ( 'NONE',  ( 46.74583929422170314, -73.84834818087099961, -2.656434933962762202 ) ) ;
#20553 = VERTEX_POINT ( 'NONE', #21484 ) ;
#20554 = CARTESIAN_POINT ( 'NONE',  ( -18.80176912509999809, -92.50000000000000000, 23.77750384849999676 ) ) ;
#20555 = CARTESIAN_POINT ( 'NONE',  ( -5.679770007689999289, -80.00000000000000000, 46.75000000000000000 ) ) ;
#20556 = VERTEX_POINT ( 'NONE', #15043 ) ;
#20557 = DIRECTION ( 'NONE',  ( 0.4794255386042036715, 0.000000000000000000, 0.8775825618903724257 ) ) ;
#20558 = CARTESIAN_POINT ( 'NONE',  ( -23.97049805334309269, -93.63284908740131129, -7.388380719408825570 ) ) ;
#20559 = CARTESIAN_POINT ( 'NONE',  ( -10.97062381167865830, -19.46488312546199850, -19.21093139428075602 ) ) ;
#20560 = DIRECTION ( 'NONE',  ( -0.03516156865429562878, -0.000000000000000000, -0.9993816408608722224 ) ) ;
#20561 = CARTESIAN_POINT ( 'NONE',  ( -40.96188834619999852, -65.41419836839999391, -2.576072437790000169 ) ) ;
#20562 = CIRCLE ( 'NONE', #15904, 10.00000000000000000 ) ;
#20563 = CARTESIAN_POINT ( 'NONE',  ( 6.744238910220000882, -101.2530993010000060, 13.61507422070000040 ) ) ;
#20564 = B_SPLINE_CURVE_WITH_KNOTS ( 'NONE', 3,
 ( #18006, #4751, #18150, #24999 ),
 .UNSPECIFIED., .F., .F.,
 ( 4, 4 ),
 ( 0.000000000000000000, 1.000000000000000000 ),
 .UNSPECIFIED. ) ;
#20565 = ORIENTED_EDGE ( 'NONE', *, *, #26618, .F. ) ;
#20566 = CIRCLE ( 'NONE', #10293, 5.000000000000000888 ) ;
#20567 = CARTESIAN_POINT ( 'NONE',  ( 12.26087422500000024, -93.85307999859999484, -21.67981636209999863 ) ) ;
#20568 = CARTESIAN_POINT ( 'NONE',  ( 50.00000000000000000, -12.50000000000000000, -4.500000000000000000 ) ) ;
#20569 = EDGE_CURVE ( 'NONE', #2204, #11892, #4754, .T. ) ;
#20570 = CARTESIAN_POINT ( 'NONE',  ( 15.04861839279999991, -100.9137139110000021, 4.234011249179999936 ) ) ;
#20571 = ORIENTED_EDGE ( 'NONE', *, *, #3500, .F. ) ;
#20572 = CARTESIAN_POINT ( 'NONE',  ( -5.679770007689999289, -79.50000000000000000, 46.75000000000000000 ) ) ;
#20573 = CARTESIAN_POINT ( 'NONE',  ( 19.36781163719999910, -19.46510053389999939, 10.50580276810000058 ) ) ;
#20574 = CARTESIAN_POINT ( 'NONE',  ( 7.066909182079999852, -57.47855601759999900, -22.26662627820000040 ) ) ;
#20575 = ORIENTED_EDGE ( 'NONE', *, *, #11780, .T. ) ;
#20576 = EDGE_CURVE ( 'NONE', #24926, #22634, #1019, .T. ) ;
#20577 = CARTESIAN_POINT ( 'NONE',  ( -17.83242922020000165, -95.72983087210000974, 13.58044602250000032 ) ) ;
#20578 = CARTESIAN_POINT ( 'NONE',  ( -19.80233708279999760, -45.95149559400000072, 14.32903646219999949 ) ) ;
#20579 = CARTESIAN_POINT ( 'NONE',  ( -26.77683864449999973, -30.20000000000000284, -49.01467436490000296 ) ) ;
#20580 = CARTESIAN_POINT ( 'NONE',  ( 22.43277176080000146, -36.00000000000000000, -11.31764183710000005 ) ) ;
#20581 = EDGE_CURVE ( 'NONE', #14378, #25468, #24228, .T. ) ;
#20582 = CARTESIAN_POINT ( 'NONE',  ( -14.93121066290857080, -74.45417263471367164, 36.29905574722082662 ) ) ;
#20583 = ADVANCED_FACE ( 'NONE', ( #10517 ), #22794, .T. ) ;
#20584 = CARTESIAN_POINT ( 'NONE',  ( 26.45575263930000176, -65.75576304679998429, 1.499652290349999806 ) ) ;
#20585 = AXIS2_PLACEMENT_3D ( 'NONE', #6600, #15458, #24369 ) ;
#20586 = ORIENTED_EDGE ( 'NONE', *, *, #22000, .T. ) ;
#20587 = B_SPLINE_CURVE_WITH_KNOTS ( 'NONE', 3,
 ( #23175, #7154, #18219, #9162 ),
 .UNSPECIFIED., .F., .F.,
 ( 4, 4 ),
 ( 0.000000000000000000, 1.000000000000000000 ),
 .UNSPECIFIED. ) ;
#20588 = CARTESIAN_POINT ( 'NONE',  ( 6.296318341739999269, -102.8486084350000027, 11.52533341650000054 ) ) ;
#20589 = DIRECTION ( 'NONE',  ( 0.4794255386042040601, 0.000000000000000000, 0.8775825618903720926 ) ) ;
#20590 = CARTESIAN_POINT ( 'NONE',  ( 20.28517606429999987, -35.95611764439999547, -9.102375980000001476 ) ) ;
#20591 = CARTESIAN_POINT ( 'NONE',  ( 10.16789867219999977, -99.55619336450000390, 14.22101452250000087 ) ) ;
#20592 = ORIENTED_EDGE ( 'NONE', *, *, #14361, .T. ) ;
#20593 = CARTESIAN_POINT ( 'NONE',  ( 23.34442203075309763, -92.53260370675270963, -19.62880660521832255 ) ) ;
#20594 = CARTESIAN_POINT ( 'NONE',  ( 16.44117558850000194, -94.63960343439998724, 17.12038290500000315 ) ) ;
#20595 = B_SPLINE_SURFACE_WITH_KNOTS ( 'NONE', 5, 5, ( 
 ( #652, #15760, #25112, #18112, #9199, #2378, #18407, #11529, #7490 ),
 ( #20439, #27445, #18255, #11678, #508, #22781, #20591, #20745, #2673 ),
 ( #24666, #9353, #27005, #801, #27151, #7190, #13875, #2819, #4699 ),
 ( #27296, #2972, #11236, #211, #16199, #13580, #5142, #15910, #24816 ),
 ( #14023, #22933, #24514, #11829, #9642, #4549, #18549, #4854, #20143 ),
 ( #9058, #20286, #353, #5429, #5703, #7902, #8036, #16352, #19247 ) ),
 .UNSPECIFIED., .F., .F., .F.,
 ( 6, 6 ),
 ( 6, 3, 6 ),
 ( 2.189016167100000132, 20.89370282910000043 ),
 ( 0.000000000000000000, 0.2500000000000000000, 0.5000000000000000000 ),
 .UNSPECIFIED. ) ;
#20596 = CARTESIAN_POINT ( 'NONE',  ( 11.15108825559999950, -100.9197081840000010, -10.94438638200000113 ) ) ;
#20597 = CARTESIAN_POINT ( 'NONE',  ( -7.473273236689999877, -100.7833805400000102, 14.04870527269999947 ) ) ;
#20598 = CARTESIAN_POINT ( 'NONE',  ( 19.97576656849999921, -35.50000000000000000, -19.97576656849999921 ) ) ;
#20599 = CARTESIAN_POINT ( 'NONE',  ( -13.18688177930000016, -93.32822605769999313, -23.58441486170000090 ) ) ;
#20600 = CARTESIAN_POINT ( 'NONE',  ( 8.705919335430001738, -36.40841211670000632, -21.16839176649999743 ) ) ;
#20601 = CARTESIAN_POINT ( 'NONE',  ( 7.358959778060000012, -101.1389411659999951, 13.51882459459999986 ) ) ;
#20602 = ORIENTED_EDGE ( 'NONE', *, *, #12855, .F. ) ;
#20603 = CARTESIAN_POINT ( 'NONE',  ( -39.85457864242477655, -73.88534697531770234, 7.248542667680531792 ) ) ;
#20604 = AXIS2_PLACEMENT_3D ( 'NONE', #11120, #6199, #15066 ) ;
#20605 = CARTESIAN_POINT ( 'NONE',  ( 23.47728460589999955, -18.62107971969999909, 1.886514288650000148 ) ) ;
#20606 = CARTESIAN_POINT ( 'NONE',  ( -2.080064695970000432, -97.58045781630001159, -19.90313438229999932 ) ) ;
#20607 = ORIENTED_EDGE ( 'NONE', *, *, #13143, .T. ) ;
#20608 = DIRECTION ( 'NONE',  ( 1.000000000000000000, 0.000000000000000000, 0.000000000000000000 ) ) ;
#20609 = EDGE_CURVE ( 'NONE', #21973, #28309, #26559, .T. ) ;
#20610 = CARTESIAN_POINT ( 'NONE',  ( 14.84965784370000108, -101.2530993010000060, 3.216001622850000352 ) ) ;
#20611 = AXIS2_PLACEMENT_3D ( 'NONE', #6086, #14694, #14825 ) ;
#20612 = DIRECTION ( 'NONE',  ( 0.4794255386042036160, 0.000000000000000000, 0.8775825618903723147 ) ) ;
#20613 = CARTESIAN_POINT ( 'NONE',  ( -16.86287214755321884, -99.33527508455092914, -8.386193468194429457 ) ) ;
#20614 = ADVANCED_FACE ( 'NONE', ( #4715 ), #6767, .T. ) ;
#20615 = FACE_OUTER_BOUND ( 'NONE', #19065, .T. ) ;
#20616 = B_SPLINE_CURVE_WITH_KNOTS ( 'NONE', 5,
 ( #22852, #25184, #724, #5361, #12040, #25465, #18908, #22998, #27667 ),
 .UNSPECIFIED., .F., .F.,
 ( 6, 3, 6 ),
 ( 0.000000000000000000, 0.4999899763738472891, 1.000000000000000000 ),
 .UNSPECIFIED. ) ;
#20617 = CARTESIAN_POINT ( 'NONE',  ( 21.88571563610000226, -49.10861551290000193, -7.914382952229998658 ) ) ;
#20618 = ADVANCED_FACE ( 'NONE', ( #9213 ), #7025, .F. ) ;
#20619 = CARTESIAN_POINT ( 'NONE',  ( -40.00441865919010098, -74.28334043021989430, -7.315281843715277788 ) ) ;
#20620 = CARTESIAN_POINT ( 'NONE',  ( 0.000000000000000000, -101.1889999979999999, 0.000000000000000000 ) ) ;
#20621 = ORIENTED_EDGE ( 'NONE', *, *, #19024, .F. ) ;
#20622 = EDGE_CURVE ( 'NONE', #22934, #15684, #5124, .T. ) ;
#20623 = CARTESIAN_POINT ( 'NONE',  ( 36.24656953779999924, -74.89763148439999441, -15.05817772819999867 ) ) ;
#20624 = CARTESIAN_POINT ( 'NONE',  ( 6.997793179249999440, -101.3256027139999986, 14.28490435800000036 ) ) ;
#20625 = CARTESIAN_POINT ( 'NONE',  ( 7.734359568749999525, -19.46510050329999686, -20.63161913629999944 ) ) ;
#20626 = FACE_OUTER_BOUND ( 'NONE', #8685, .T. ) ;
#20627 = CARTESIAN_POINT ( 'NONE',  ( -14.69770337990000009, -66.39466164420001348, 22.32636990160000323 ) ) ;
#20628 = CARTESIAN_POINT ( 'NONE',  ( 8.993405562710000467, -35.68342189879999893, -20.12810762659999853 ) ) ;
#20629 = CARTESIAN_POINT ( 'NONE',  ( 0.000000000000000000, -2.000000000000000000, 0.000000000000000000 ) ) ;
#20630 = AXIS2_PLACEMENT_3D ( 'NONE', #12114, #16356, #23211 ) ;
#20631 = CARTESIAN_POINT ( 'NONE',  ( 29.41275679339999982, -11.79999999999999893, 53.83969017199999740 ) ) ;
#20632 = AXIS2_PLACEMENT_3D ( 'NONE', #11979, #22940, #16361 ) ;
#20633 = DIRECTION ( 'NONE',  ( 0.000000000000000000, 1.000000000000000000, 0.000000000000000000 ) ) ;
#20634 = CARTESIAN_POINT ( 'NONE',  ( -17.59047486835680019, -93.38817447856811782, -21.35100961780407403 ) ) ;
#20635 = CARTESIAN_POINT ( 'NONE',  ( -16.86249289530055151, -97.53591929645045866, -10.88383259781367940 ) ) ;
#20636 = CARTESIAN_POINT ( 'NONE',  ( 27.68682485439999752, -24.80000000000000071, 50.68039294919999804 ) ) ;
#20637 = CARTESIAN_POINT ( 'NONE',  ( -11.24329055421529766, -40.03422670525277738, -22.26111247093807322 ) ) ;
#20638 = ORIENTED_EDGE ( 'NONE', *, *, #7324, .F. ) ;
#20639 = CARTESIAN_POINT ( 'NONE',  ( 8.099920077730001111, -100.8733989549999990, 13.47813240850000049 ) ) ;
#20640 = CARTESIAN_POINT ( 'NONE',  ( -23.61875854070000003, -94.52293512109999085, -3.856443273130000016 ) ) ;
#20641 = ORIENTED_EDGE ( 'NONE', *, *, #10612, .T. ) ;
#20642 = CARTESIAN_POINT ( 'NONE',  ( 8.526512829119999691E-15, -89.50000000000000000, -5.107025913280000248E-16 ) ) ;
#20643 = DIRECTION ( 'NONE',  ( -0.7414452336469260496, 0.000000000000000000, 0.6710133869769331350 ) ) ;
#20644 = CARTESIAN_POINT ( 'NONE',  ( -38.25000000000000000, -63.30468293320000583, 1.587713240270000048 ) ) ;
#20645 = AXIS2_PLACEMENT_3D ( 'NONE', #9557, #5191, #11731 ) ;
#20646 = DIRECTION ( 'NONE',  ( 0.000000000000000000, 1.000000000000000000, 0.000000000000000000 ) ) ;
#20647 = CARTESIAN_POINT ( 'NONE',  ( 47.19280574540000117, -74.66665734379999719, -1.149945984370000174 ) ) ;
#20648 = ADVANCED_FACE ( 'NONE', ( #13748 ), #7593, .T. ) ;
#20649 = CARTESIAN_POINT ( 'NONE',  ( -14.63774944959999935, -74.36723410090000641, 36.92911291229999904 ) ) ;
#20650 = CARTESIAN_POINT ( 'NONE',  ( -21.10814673490000004, -64.47177029070000742, 15.24425172959999841 ) ) ;
#20651 = CARTESIAN_POINT ( 'NONE',  ( 23.91589042248623187, -92.93978723899958538, -18.92829633725156313 ) ) ;
#20652 = VERTEX_POINT ( 'NONE', #20005 ) ;
#20653 = CARTESIAN_POINT ( 'NONE',  ( -12.75356989989999867, -71.11103304360000266, -24.81876632530000037 ) ) ;
#20654 = FACE_OUTER_BOUND ( 'NONE', #28132, .T. ) ;
#20655 = DIRECTION ( 'NONE',  ( 0.000000000000000000, -1.000000000000000000, 0.000000000000000000 ) ) ;
#20656 = AXIS2_PLACEMENT_3D ( 'NONE', #19128, #28017, #8055 ) ;
#20657 = CARTESIAN_POINT ( 'NONE',  ( 7.347638122930000545E-15, -79.00000000000000000, -40.00000000000000000 ) ) ;
#20658 = CARTESIAN_POINT ( 'NONE',  ( 15.44884930899999986, -100.9728541479999961, 2.166274872270000262 ) ) ;
#20659 = VERTEX_POINT ( 'NONE', #20157 ) ;
#20660 = EDGE_CURVE ( 'NONE', #25644, #321, #28416, .T. ) ;
#20661 = VERTEX_POINT ( 'NONE', #12397 ) ;
#20662 = CARTESIAN_POINT ( 'NONE',  ( 7.215414233289999757, -82.25000000000000000, 40.70731707320000226 ) ) ;
#20663 = AXIS2_PLACEMENT_3D ( 'NONE', #21914, #1965, #20608 ) ;
#20664 = DIRECTION ( 'NONE',  ( 1.000000000000000000, 0.000000000000000000, 0.000000000000000000 ) ) ;
#20665 = CARTESIAN_POINT ( 'NONE',  ( 4.226834115039999951, -93.34497626389999425, 25.39917024580000060 ) ) ;
#20666 = ORIENTED_EDGE ( 'NONE', *, *, #6604, .T. ) ;
#20667 = ORIENTED_EDGE ( 'NONE', *, *, #28575, .F. ) ;
#20668 = CARTESIAN_POINT ( 'NONE',  ( -25.97364739661740174, -94.01603309698641908, -2.107898430554720370 ) ) ;
#20669 = CARTESIAN_POINT ( 'NONE',  ( 20.33566493280000032, -36.00000000000000000, -9.885503726129998725 ) ) ;
#20670 = CARTESIAN_POINT ( 'NONE',  ( 47.13476942299999450, -74.39425306939999416, -1.308869127139999922 ) ) ;
#20671 = ORIENTED_EDGE ( 'NONE', *, *, #23007, .T. ) ;
#20672 = CARTESIAN_POINT ( 'NONE',  ( 7.247217007263055955, -73.85166138358573562, -39.79858521572417374 ) ) ;
#20673 = DIRECTION ( 'NONE',  ( 0.000000000000000000, -1.000000000000000000, 0.000000000000000000 ) ) ;
#20674 = DIRECTION ( 'NONE',  ( 1.000000000000000000, 0.000000000000000000, 0.000000000000000000 ) ) ;
#20675 = EDGE_CURVE ( 'NONE', #8713, #12207, #3717, .T. ) ;
#20676 = CARTESIAN_POINT ( 'NONE',  ( -2.472996982579999781, -66.23852357979998828, -26.10313830509999988 ) ) ;
#20677 = FACE_OUTER_BOUND ( 'NONE', #20388, .T. ) ;
#20678 = VERTEX_POINT ( 'NONE', #2985 ) ;
#20679 = ADVANCED_FACE ( 'NONE', ( #18712 ), #27956, .T. ) ;
#20680 = CARTESIAN_POINT ( 'NONE',  ( 27.02683049547185234, -18.50000000000000000, 2.817888817433861881 ) ) ;
#20681 = EDGE_CURVE ( 'NONE', #10004, #23975, #21442, .T. ) ;
#20682 = VECTOR ( 'NONE', #15186, 1000.000000000000000 ) ;
#20683 = CARTESIAN_POINT ( 'NONE',  ( -15.21470405170000006, -101.0782545459999966, 3.282628937979999773 ) ) ;
#20684 = CARTESIAN_POINT ( 'NONE',  ( -22.00249031550000112, -74.43208506860000284, -32.67527180340000825 ) ) ;
#20685 = ORIENTED_EDGE ( 'NONE', *, *, #27219, .T. ) ;
#20686 = AXIS2_PLACEMENT_3D ( 'NONE', #1822, #17838, #15782 ) ;
#20687 = DIRECTION ( 'NONE',  ( -0.4151946956541399669, 0.5000000000001689759, -0.7600087925152558821 ) ) ;
#20688 = DIRECTION ( 'NONE',  ( 0.000000000000000000, 1.000000000000000000, 0.000000000000000000 ) ) ;
#20689 = DIRECTION ( 'NONE',  ( 0.000000000000000000, -1.000000000000000000, 0.000000000000000000 ) ) ;
#20690 = CARTESIAN_POINT ( 'NONE',  ( 23.55423057129999975, -93.65023913340000661, -9.043220619339999544 ) ) ;
#20691 = ORIENTED_EDGE ( 'NONE', *, *, #12897, .F. ) ;
#20692 = FACE_OUTER_BOUND ( 'NONE', #4941, .T. ) ;
#20693 = CARTESIAN_POINT ( 'NONE',  ( 21.83772201000000024, -64.02328494229999478, 11.48627575220000097 ) ) ;
#20694 = LINE ( 'NONE', #18058, #22247 ) ;
#20695 = CARTESIAN_POINT ( 'NONE',  ( 15.65734951540625630, -101.5026031440680470, 3.803058839663215451 ) ) ;
#20696 = DIRECTION ( 'NONE',  ( 0.000000000000000000, -1.000000000000000000, 0.000000000000000000 ) ) ;
#20697 = ORIENTED_EDGE ( 'NONE', *, *, #7974, .T. ) ;
#20698 = CARTESIAN_POINT ( 'NONE',  ( 22.89432163829999922, -45.92926717529999792, 10.24748840149999829 ) ) ;
#20699 = STYLED_ITEM ( 'NONE', ( #25456 ), #25670 ) ;
#20700 = ITEM_DEFINED_TRANSFORMATION ( 'NONE', 'NONE', #12467,  #26433 ) ;
#20701 = CARTESIAN_POINT ( 'NONE',  ( -11.70763318529999886, -59.02987586149999544, -20.35466320700000153 ) ) ;
#20702 = VECTOR ( 'NONE', #5208, 1000.000000000000000 ) ;
#20703 = DIRECTION ( 'NONE',  ( 0.000000000000000000, 1.000000000000000000, 0.000000000000000000 ) ) ;
#20704 = CARTESIAN_POINT ( 'NONE',  ( 2.725557285477327341, -94.35872894872866823, 25.28257344816310948 ) ) ;
#20705 = ORIENTED_EDGE ( 'NONE', *, *, #3911, .T. ) ;
#20706 = ADVANCED_FACE ( 'NONE', ( #28013 ), #536, .T. ) ;
#20707 = CARTESIAN_POINT ( 'NONE',  ( 46.73034331009336739, -73.83477249655828700, -2.695375482873064943 ) ) ;
#20708 = ORIENTED_EDGE ( 'NONE', *, *, #2251, .T. ) ;
#20709 = TOROIDAL_SURFACE ( 'NONE', #9520, 38.75000000000000000, 0.5000000000000000000 ) ;
#20710 = CARTESIAN_POINT ( 'NONE',  ( 23.06458040940000132, -53.77454410920000072, 10.33795933400000067 ) ) ;
#20711 = B_SPLINE_CURVE_WITH_KNOTS ( 'NONE', 5,
 ( #10989, #8546, #17449, #20773, #3285, #7521 ),
 .UNSPECIFIED., .F., .F.,
 ( 6, 6 ),
 ( 0.000000000000000000, 1.000000000000000000 ),
 .UNSPECIFIED. ) ;
#20712 = CARTESIAN_POINT ( 'NONE',  ( -6.085662280650000255, -101.5026188610000020, 14.82188091429999943 ) ) ;
#20713 = ORIENTED_EDGE ( 'NONE', *, *, #24180, .T. ) ;
#20714 = CARTESIAN_POINT ( 'NONE',  ( -2.583988331150000040, -57.40875702419999982, -25.23271569440000306 ) ) ;
#20715 = CARTESIAN_POINT ( 'NONE',  ( 21.21808891099999883, -34.59820414320000026, -7.670974023059999425 ) ) ;
#20716 = DIRECTION ( 'NONE',  ( 0.4794255386042041156, 0.000000000000000000, 0.8775825618903722036 ) ) ;
#20717 = DIRECTION ( 'NONE',  ( -0.3687499999999802047, 0.000000000000000000, 0.9295286103719532234 ) ) ;
#20718 = DIRECTION ( 'NONE',  ( 0.9828852004421827493, 0.06995790998171046160, -0.1704188181590321205 ) ) ;
#20719 = CARTESIAN_POINT ( 'NONE',  ( -41.41155280139999917, -65.17124718639999514, -2.835686332019999867 ) ) ;
#20720 = CARTESIAN_POINT ( 'NONE',  ( 46.70302539038219436, -79.89150110136301919, -3.470455026150449651 ) ) ;
#20721 = ORIENTED_EDGE ( 'NONE', *, *, #6399, .F. ) ;
#20722 = CARTESIAN_POINT ( 'NONE',  ( -32.36019060869999464, -80.06168530479999390, -22.53893507739999791 ) ) ;
#20723 = ADVANCED_FACE ( 'NONE', ( #27866 ), #358, .F. ) ;
#20724 = CARTESIAN_POINT ( 'NONE',  ( -20.20157662561761214, -60.34340089795642115, 12.31263473384953322 ) ) ;
#20725 = DIRECTION ( 'NONE',  ( 1.000000000000000000, 0.000000000000000000, 0.000000000000000000 ) ) ;
#20726 = ORIENTED_EDGE ( 'NONE', *, *, #17999, .T. ) ;
#20727 = CIRCLE ( 'NONE', #21195, 0.4999999999999981126 ) ;
#20728 = DIRECTION ( 'NONE',  ( 0.000000000000000000, -1.000000000000000000, 0.000000000000000000 ) ) ;
#20729 = CARTESIAN_POINT ( 'NONE',  ( -12.54588562670000051, -101.3256027139999986, -9.778723817850000444 ) ) ;
#20730 = CARTESIAN_POINT ( 'NONE',  ( 2.842170943039999687E-14, -72.00000000000000000, 1.776356839399999804E-15 ) ) ;
#20731 = EDGE_LOOP ( 'NONE', ( #23997, #26434, #24076, #23678, #6257 ) ) ;
#20732 = CARTESIAN_POINT ( 'NONE',  ( 37.05123091498987264, -80.05388659141317476, -13.65971926633490163 ) ) ;
#20733 = CIRCLE ( 'NONE', #16518, 5.499999999999998224 ) ;
#20734 = CARTESIAN_POINT ( 'NONE',  ( -19.06307702970000051, -26.06274386020000122, 13.87368263639999988 ) ) ;
#20735 = DIRECTION ( 'NONE',  ( 1.000000000000000000, 0.000000000000000000, 9.436895709309994757E-16 ) ) ;
#20736 = CARTESIAN_POINT ( 'NONE',  ( -8.256726973129998370, -80.00000000000000000, 39.42856679209999982 ) ) ;
#20737 = CARTESIAN_POINT ( 'NONE',  ( 23.23309277569999765, -57.41957472270000551, -9.464544134220000515 ) ) ;
#20738 = CARTESIAN_POINT ( 'NONE',  ( 26.84354920890000074, -67.87586094739999965, 1.442210595809999996 ) ) ;
#20739 = VERTEX_POINT ( 'NONE', #12534 ) ;
#20740 = EDGE_CURVE ( 'NONE', #1856, #15453, #1451, .T. ) ;
#20741 = CARTESIAN_POINT ( 'NONE',  ( 20.46633117200000029, -56.50943265579999775, 11.19343934389999973 ) ) ;
#20742 = CARTESIAN_POINT ( 'NONE',  ( -38.90877162625164232, -73.50999119021167871, -7.168130346706902856 ) ) ;
#20743 = CLOSED_SHELL ( 'NONE', ( #2199, #3654, #20404, #11265, #6507, #5368, #17376, #3652 ) ) ;
#20744 = EDGE_CURVE ( 'NONE', #6032, #26457, #11183, .T. ) ;
#20745 = CARTESIAN_POINT ( 'NONE',  ( 10.19815034219999994, -99.57131501109998339, 14.12374920210000084 ) ) ;
#20746 = ORIENTED_EDGE ( 'NONE', *, *, #8960, .T. ) ;
#20747 = CARTESIAN_POINT ( 'NONE',  ( -11.16118678780000018, -80.00000000000000000, 46.75000000000000000 ) ) ;
#20748 = CARTESIAN_POINT ( 'NONE',  ( -17.08206735869999804, -92.57197946150000689, -23.65181049579999950 ) ) ;
#20749 = CARTESIAN_POINT ( 'NONE',  ( -18.67939945255520229, -18.95847994161255912, 11.45706375696013524 ) ) ;
#20750 = DIRECTION ( 'NONE',  ( 0.000000000000000000, -1.000000000000000000, 0.000000000000000000 ) ) ;
#20751 = DIRECTION ( 'NONE',  ( 0.000000000000000000, 1.000000000000000000, 0.000000000000000000 ) ) ;
#20752 = EDGE_CURVE ( 'NONE', #25380, #9289, #6497, .T. ) ;
#20753 = DIRECTION ( 'NONE',  ( 0.000000000000000000, 1.000000000000000000, 0.000000000000000000 ) ) ;
#20754 = ORIENTED_EDGE ( 'NONE', *, *, #1923, .F. ) ;
#20755 = CARTESIAN_POINT ( 'NONE',  ( -43.27802036723892343, -65.10668761694192597, 0.09248738125474099958 ) ) ;
#20756 = DIRECTION ( 'NONE',  ( 1.000000000000000000, 0.000000000000000000, 0.000000000000000000 ) ) ;
#20757 = CARTESIAN_POINT ( 'NONE',  ( -12.53622301170538123, -19.47630496351773033, 19.30239230919325166 ) ) ;
#20758 = CARTESIAN_POINT ( 'NONE',  ( 11.83146454849999962, -101.1461869959999973, -11.00634589319999890 ) ) ;
#20759 = VERTEX_POINT ( 'NONE', #26104 ) ;
#20760 = CARTESIAN_POINT ( 'NONE',  ( -2.295868756434714442, -19.47636826821743483, -22.90451916462247439 ) ) ;
#20761 = CARTESIAN_POINT ( 'NONE',  ( 11.84697068120000019, -101.1716782170000073, -10.35390073449999981 ) ) ;
#20762 = CARTESIAN_POINT ( 'NONE',  ( -2.508141046650000039, -45.95149559400000072, -24.31384519909999753 ) ) ;
#20763 = CARTESIAN_POINT ( 'NONE',  ( -17.97738387593933140, -98.68740020288944947, -7.995275462725576432 ) ) ;
#20764 = DIRECTION ( 'NONE',  ( -0.4151946956541399669, 0.5000000000001689759, -0.7600087925152558821 ) ) ;
#20765 = AXIS2_PLACEMENT_3D ( 'NONE', #9619, #24935, #16474 ) ;
#20766 = DIRECTION ( 'NONE',  ( 0.3687499999999825917, 0.000000000000000000, -0.9295286103719523352 ) ) ;
#20767 = CARTESIAN_POINT ( 'NONE',  ( 22.46437391599999955, -49.07760086100000052, -9.030336851770002227 ) ) ;
#20768 = CARTESIAN_POINT ( 'NONE',  ( 13.47882164853999676, -98.28141959653622450, 15.05059098890579961 ) ) ;
#20769 = FACE_OUTER_BOUND ( 'NONE', #23301, .T. ) ;
#20770 = ORIENTED_EDGE ( 'NONE', *, *, #673, .F. ) ;
#20771 = B_SPLINE_CURVE_WITH_KNOTS ( 'NONE', 3,
 ( #3548, #5859, #5310, #25697, #14606, #14471, #821, #16804, #14740, #3411, #25837, #3136, #12132, #9663, #27462, #28019, #9946, #7511, #20903, #21048, #7919, #23367, #23511, #23227, #12403, #16372, #18571, #25284, #23639, #1108 ),
 .UNSPECIFIED., .F., .F.,
 ( 4, 1, 1, 1, 1, 2, 2, 1, 1, 1, 1, 2, 2, 2, 1, 1, 1, 1, 2, 2, 4 ),
 ( 0.000000000000000000, 0.1250000000000265898, 0.1875000000000392464, 0.2187500000000447142, 0.2343750000000459632, 0.2421875000000486833, 0.2500000000000514033, 0.3750000000001049161, 0.4375000000001317280, 0.4687500000001439959, 0.4843750000001532663, 0.4921875000001595390, 0.5000000000001657563, 0.6250000000001812994, 0.6875000000001900702, 0.7187500000001965095, 0.7343750000001981748, 0.7421875000001975087, 0.7460937500001967315, 0.7500000000001958433, 1.000000000000000000 ),
 .UNSPECIFIED. ) ;
#20772 = CARTESIAN_POINT ( 'NONE',  ( 6.830934818989999435, -101.1411470200000053, 13.79009341090000085 ) ) ;
#20773 = CARTESIAN_POINT ( 'NONE',  ( -9.465086699151784799, -93.62676972709405732, -23.38439031276536539 ) ) ;
#20774 = CARTESIAN_POINT ( 'NONE',  ( 7.661042932279999995, -101.3151549749999987, 13.94743070049999822 ) ) ;
#20775 = CARTESIAN_POINT ( 'NONE',  ( -14.52637129600000065, -65.75479088560000207, 22.16126353170000129 ) ) ;
#20776 = CARTESIAN_POINT ( 'NONE',  ( 8.363364595560000225, -35.90622649329999660, -21.15739189799999664 ) ) ;
#20777 = CARTESIAN_POINT ( 'NONE',  ( 7.248796347620719338, -73.89318255930692203, 39.86740956980206363 ) ) ;
#20778 = CARTESIAN_POINT ( 'NONE',  ( 2.042810365310000056E-12, -74.50000000000000000, -2.458477865729999957E-12 ) ) ;
#20779 = ADVANCED_FACE ( 'NONE', ( #4242 ), #6130, .T. ) ;
#20780 = FACE_OUTER_BOUND ( 'NONE', #12567, .T. ) ;
#20781 = CARTESIAN_POINT ( 'NONE',  ( 0.4184155325020000316, -93.00000902169999506, -30.38020818910000287 ) ) ;
#20782 = EDGE_CURVE ( 'NONE', #17731, #20553, #16334, .T. ) ;
#20783 = FACE_OUTER_BOUND ( 'NONE', #13561, .T. ) ;
#20784 = ORIENTED_EDGE ( 'NONE', *, *, #20978, .F. ) ;
#20785 = CARTESIAN_POINT ( 'NONE',  ( 8.042004129799998680, -100.9405349759999950, 13.76814388520000065 ) ) ;
#20786 = CARTESIAN_POINT ( 'NONE',  ( -20.41940881060000024, -94.07621218059999535, 14.28684394100000077 ) ) ;
#20787 = ORIENTED_EDGE ( 'NONE', *, *, #4571, .T. ) ;
#20788 = EDGE_CURVE ( 'NONE', #21750, #16528, #21772, .T. ) ;
#20789 = CARTESIAN_POINT ( 'NONE',  ( 9.047106472501580399, -92.80045754867209951, 29.12732774022750704 ) ) ;
#20790 = EDGE_CURVE ( 'NONE', #13129, #17905, #25607, .T. ) ;
#20791 = CARTESIAN_POINT ( 'NONE',  ( 0.4730157680896098227, -100.0559847773881330, -17.25169209895160805 ) ) ;
#20792 = DIRECTION ( 'NONE',  ( 0.000000000000000000, 1.000000000000000000, 0.000000000000000000 ) ) ;
#20793 = CARTESIAN_POINT ( 'NONE',  ( -7.400691967549999362, -74.17650256410000509, 39.62483793549999689 ) ) ;
#20794 = CARTESIAN_POINT ( 'NONE',  ( 4.500000000000000000, -13.00000000000000000, 31.00000000000000000 ) ) ;
#20795 = CARTESIAN_POINT ( 'NONE',  ( -7.219194746715977828, -73.62392792452344281, -39.33235237970639986 ) ) ;
#20796 = CARTESIAN_POINT ( 'NONE',  ( 1.065814103639999922E-14, -19.50000000000000000, 2.664535259099999805E-15 ) ) ;
#20797 = CARTESIAN_POINT ( 'NONE',  ( -16.70219504179999959, -100.0012196380000091, 6.767083061890000195 ) ) ;
#20798 = ORIENTED_EDGE ( 'NONE', *, *, #25700, .T. ) ;
#20799 = DIRECTION ( 'NONE',  ( 0.000000000000000000, 1.000000000000000000, 0.000000000000000000 ) ) ;
#20800 = CARTESIAN_POINT ( 'NONE',  ( 1.375225265779999928, -94.98812079580000045, 24.46248543800000164 ) ) ;
#20801 = CARTESIAN_POINT ( 'NONE',  ( -21.87551306609999813, -79.25000000000000000, -33.18922156509999866 ) ) ;
#20802 = DIRECTION ( 'NONE',  ( 0.1770468907230372535, 0.000000000000000000, 0.9842024174352067556 ) ) ;
#20803 = CARTESIAN_POINT ( 'NONE',  ( 15.94609587029999886, -101.3399913430000083, 2.448433415369999810 ) ) ;
#20804 = VERTEX_POINT ( 'NONE', #4392 ) ;
#20805 = ORIENTED_EDGE ( 'NONE', *, *, #7898, .T. ) ;
#20806 = CARTESIAN_POINT ( 'NONE',  ( -0.5413073883429999622, -57.47855574479999774, -23.35488927860000175 ) ) ;
#20807 = DIRECTION ( 'NONE',  ( -0.6685326369589543738, 0.000000000000000000, -0.7436828042389492799 ) ) ;
#20808 = CARTESIAN_POINT ( 'NONE',  ( 1.436120303979999902, -94.52419051769999214, 23.97566470769999825 ) ) ;
#20809 = VERTEX_POINT ( 'NONE', #20121 ) ;
#20810 = ADVANCED_FACE ( 'NONE', ( #8737 ), #19585, .T. ) ;
#20811 = CARTESIAN_POINT ( 'NONE',  ( 20.82958082409999889, -36.06003250059999488, -9.510880482430000171 ) ) ;
#20812 = ORIENTED_EDGE ( 'NONE', *, *, #26009, .T. ) ;
#20813 = CARTESIAN_POINT ( 'NONE',  ( 7.246819345882899555, -74.12723354427720324, -40.21639064511597184 ) ) ;
#20814 = CARTESIAN_POINT ( 'NONE',  ( -11.45050398651610735, -61.30079904130542445, 20.94026329283510535 ) ) ;
#20815 = EDGE_CURVE ( 'NONE', #18945, #16909, #9954, .T. ) ;
#20816 = ORIENTED_EDGE ( 'NONE', *, *, #397, .F. ) ;
#20817 = CARTESIAN_POINT ( 'NONE',  ( -18.69985100839999959, -93.00000000000000000, 22.78328762010000119 ) ) ;
#20818 = CARTESIAN_POINT ( 'NONE',  ( -3.203052480429999793, -67.37930764479999368, -27.34961382279999853 ) ) ;
#20819 = CARTESIAN_POINT ( 'NONE',  ( -15.22881500629999962, -71.94538141299999268, 23.83405028770000200 ) ) ;
#20820 = ORIENTED_EDGE ( 'NONE', *, *, #27855, .T. ) ;
#20821 = CARTESIAN_POINT ( 'NONE',  ( 0.2284267155709999997, -93.00000000000000000, -29.91770779450000362 ) ) ;
#20822 = CARTESIAN_POINT ( 'NONE',  ( -15.74135051609999714, -100.8503292370000111, 3.071429158959999572 ) ) ;
#20823 = CARTESIAN_POINT ( 'NONE',  ( 23.95396754599999767, -58.97460807019999862, 0.8392115891270000017 ) ) ;
#20824 = CARTESIAN_POINT ( 'NONE',  ( -21.35786030099999877, -65.07443093669999712, 13.27975315080000129 ) ) ;
#20825 = VERTEX_POINT ( 'NONE', #4528 ) ;
#20826 = CARTESIAN_POINT ( 'NONE',  ( -27.18988201479999844, -18.49844555430000170, -49.77074518290000071 ) ) ;
#20827 = DIRECTION ( 'NONE',  ( 0.000000000000000000, -1.000000000000000000, 0.000000000000000000 ) ) ;
#20828 = AXIS2_PLACEMENT_3D ( 'NONE', #12375, #28393, #25937 ) ;
#20829 = CARTESIAN_POINT ( 'NONE',  ( -2.619606448679999922, -19.18584080579999807, -24.29997799329999708 ) ) ;
#20830 = CARTESIAN_POINT ( 'NONE',  ( 36.43448083739620813, -74.04079074338399380, -14.03271623279055724 ) ) ;
#20831 = ORIENTED_EDGE ( 'NONE', *, *, #11670, .T. ) ;
#20832 = DIRECTION ( 'NONE',  ( 0.000000000000000000, 1.000000000000000000, 0.000000000000000000 ) ) ;
#20833 = B_SPLINE_CURVE_WITH_KNOTS ( 'NONE', 3,
 ( #20511, #24446, #27222, #15540, #18332, #7262, #16127, #11755, #20668, #2305, #11155, #17893, #727, #20073, #15685, #20218, #289, #18034, #26932, #20958, #3459, #27365, #9576, #25186, #23421, #3050, #7706, #14246, #16858, #14102, #16571, #1015, #14389, #7409, #5362, #3322, #16426 ),
 .UNSPECIFIED., .F., .F.,
 ( 4, 2, 2, 1, 1, 1, 2, 2, 2, 2, 1, 1, 1, 2, 2, 2, 2, 1, 1, 1, 2, 2, 4 ),
 ( 0.000000000000000000, 0.1249999999999996114, 0.1875000000000000278, 0.2187500000000002220, 0.2343750000000005551, 0.2421875000000005551, 0.2460937500000005274, 0.2500000000000005551, 0.3749999999999905076, 0.4374999999999858447, 0.4687499999999831801, 0.4843749999999818479, 0.4921874999999809597, 0.4960937499999809597, 0.4999999999999809597, 0.6249999999999820144, 0.6874999999999825695, 0.7187499999999829026, 0.7343749999999827915, 0.7421874999999827915, 0.7460937499999830136, 0.7499999999999832356, 1.000000000000000000 ),
 .UNSPECIFIED. ) ;
#20834 = CARTESIAN_POINT ( 'NONE',  ( 21.58303642010000090, -61.82150526550000080, 10.78270930949999951 ) ) ;
#20835 = AXIS2_PLACEMENT_3D ( 'NONE', #23229, #16078, #16374 ) ;
#20836 = CARTESIAN_POINT ( 'NONE',  ( 7.472179712070000868, -35.14393334239999689, -21.32187190240000163 ) ) ;
#20837 = CARTESIAN_POINT ( 'NONE',  ( 16.62650357984983174, -100.1517898586434114, 4.328685068564946725 ) ) ;
#20838 = DIRECTION ( 'NONE',  ( 1.000000000000000000, 0.000000000000000000, 0.000000000000000000 ) ) ;
#20839 = ORIENTED_EDGE ( 'NONE', *, *, #26923, .F. ) ;
#20840 = B_SPLINE_SURFACE_WITH_KNOTS ( 'NONE', 5, 5, ( 
 ( #16584, #7274, #5512, #2910, #597, #1035, #7424, #5231, #22721 ),
 ( #25202, #16141, #25045, #18921, #5078, #12056, #9873, #9590, #3334 ),
 ( #12198, #7579, #18787, #9441, #14116, #23015, #16725, #21113, #25621 ),
 ( #7717, #20528, #1168, #13965, #27381, #10007, #22869, #27801, #11772 ),
 ( #25478, #745, #18640, #5377, #20823, #3065, #11920, #885, #27536 ),
 ( #16443, #14260, #23153, #25758, #23435, #5786, #12463, #25891, #19334 ) ),
 .UNSPECIFIED., .F., .F., .F.,
 ( 6, 6 ),
 ( 6, 3, 6 ),
 ( 8.242378609670000245, 18.74558921149999691 ),
 ( 0.000000000000000000, 1.000000000000000000, 2.000000000000000000 ),
 .UNSPECIFIED. ) ;
#20841 = CARTESIAN_POINT ( 'NONE',  ( -10.97235754340000113, -18.50000000000000000, 18.39710783539999994 ) ) ;
#20842 = EDGE_CURVE ( 'NONE', #10004, #27670, #16197, .T. ) ;
#20843 = CARTESIAN_POINT ( 'NONE',  ( 24.98429922149999882, -68.01082593649999808, -9.444232459920000267 ) ) ;
#20844 = CARTESIAN_POINT ( 'NONE',  ( 3.262018583601672184, -94.16479847359984490, 25.56489855335652805 ) ) ;
#20845 = VECTOR ( 'NONE', #15846, 1000.000000000000000 ) ;
#20846 = VERTEX_POINT ( 'NONE', #14005 ) ;
#20847 = EDGE_CURVE ( 'NONE', #23425, #28710, #12143, .T. ) ;
#20848 = CIRCLE ( 'NONE', #1754, 0.8000000000000003775 ) ;
#20849 = CARTESIAN_POINT ( 'NONE',  ( -41.45000000000000284, -64.11445222650000630, 2.857883832489999776 ) ) ;
#20850 = CYLINDRICAL_SURFACE ( 'NONE', #11863, 7.249999999999999112 ) ;
#20851 = ORIENTED_EDGE ( 'NONE', *, *, #23539, .T. ) ;
#20852 = CARTESIAN_POINT ( 'NONE',  ( -13.52482488829999951, -26.99661847659999836, 20.57476094929999633 ) ) ;
#20853 = CARTESIAN_POINT ( 'NONE',  ( -5.676692421769999441, -101.1516803200000112, 14.23663479639999885 ) ) ;
#20854 = ORIENTED_EDGE ( 'NONE', *, *, #26485, .F. ) ;
#20855 = EDGE_CURVE ( 'NONE', #20206, #300, #15864, .T. ) ;
#20856 = CIRCLE ( 'NONE', #1323, 57.75000000000000000 ) ;
#20857 = CARTESIAN_POINT ( 'NONE',  ( 39.49501612680000306, -74.05258142290000478, 7.367357169019999930 ) ) ;
#20858 = CARTESIAN_POINT ( 'NONE',  ( -10.48421507011602927, -19.48210984065671880, -20.91038783075365970 ) ) ;
#20859 = DIRECTION ( 'NONE',  ( 0.000000000000000000, -1.000000000000000000, 0.000000000000000000 ) ) ;
#20860 = CARTESIAN_POINT ( 'NONE',  ( 0.3059185938709999553, -93.00000000000000000, 14.72672055670000013 ) ) ;
#20861 = CARTESIAN_POINT ( 'NONE',  ( 9.917934831007896079, -63.16257045312386964, -24.43292808095910118 ) ) ;
#20862 = VERTEX_POINT ( 'NONE', #23057 ) ;
#20863 = CARTESIAN_POINT ( 'NONE',  ( -32.69645379630000548, -79.50000000000000000, -21.71458329359999695 ) ) ;
#20864 = CARTESIAN_POINT ( 'NONE',  ( -36.23922253580000330, -79.50000000000000000, -26.33972759919999973 ) ) ;
#20865 = CARTESIAN_POINT ( 'NONE',  ( -20.61424083620000047, -93.67870248599999172, 14.15158961350000055 ) ) ;
#20866 = CARTESIAN_POINT ( 'NONE',  ( 26.69293917519999937, -33.49689110869999809, 48.86109741659999628 ) ) ;
#20867 = ORIENTED_EDGE ( 'NONE', *, *, #10927, .T. ) ;
#20868 = CARTESIAN_POINT ( 'NONE',  ( -3.807886452449999570, -79.99999996820000092, 46.75000006680000553 ) ) ;
#20869 = DIRECTION ( 'NONE',  ( 1.000000000000000000, 0.000000000000000000, 0.000000000000000000 ) ) ;
#20870 = DIRECTION ( 'NONE',  ( 0.000000000000000000, 0.000000000000000000, 1.000000000000000000 ) ) ;
#20871 = ORIENTED_EDGE ( 'NONE', *, *, #20407, .F. ) ;
#20872 = VECTOR ( 'NONE', #27957, 1000.000000000000114 ) ;
#20873 = CARTESIAN_POINT ( 'NONE',  ( -16.68089843889999813, -99.91542228490000355, 6.721411764870000027 ) ) ;
#20874 = AXIS2_PLACEMENT_3D ( 'NONE', #28665, #12642, #25928 ) ;
#20875 = CARTESIAN_POINT ( 'NONE',  ( -19.24564007919999753, -39.36582103120000653, 12.09558240470000179 ) ) ;
#20876 = DIRECTION ( 'NONE',  ( -0.8775825618903722036, 0.000000000000000000, 0.4794255386042041156 ) ) ;
#20877 = CARTESIAN_POINT ( 'NONE',  ( 28.91021413440000032, -73.86467020649999426, -26.59947370389999932 ) ) ;
#20878 = CARTESIAN_POINT ( 'NONE',  ( 22.33353861309999999, -57.45905989829999783, -8.600015579559999068 ) ) ;
#20879 = CARTESIAN_POINT ( 'NONE',  ( 25.73809814099999826, -66.36684605059998887, -0.2162503729670000041 ) ) ;
#20880 = CARTESIAN_POINT ( 'NONE',  ( -10.60992277839999964, -18.50000000000000000, 18.52090900019999964 ) ) ;
#20881 = ADVANCED_FACE ( 'NONE', ( #206 ), #28742, .T. ) ;
#20882 = CARTESIAN_POINT ( 'NONE',  ( 7.609796875110000691, -99.12021627820000447, 16.26535001459999918 ) ) ;
#20884 = ORIENTED_EDGE ( 'NONE', *, *, #7763, .T. ) ;
#20883 = EDGE_CURVE ( 'NONE', #1115, #18376, #8860, .T. ) ;
#20885 = ADVANCED_FACE ( 'NONE', ( #12236 ), #9625, .F. ) ;
#20886 = CARTESIAN_POINT ( 'NONE',  ( -39.68146194298503815, -73.78481856947901463, -7.243236069910341968 ) ) ;
#20887 = CARTESIAN_POINT ( 'NONE',  ( 21.69038160389999703, -37.92210000699999739, -8.278728714260001453 ) ) ;
#20888 = ORIENTED_EDGE ( 'NONE', *, *, #22890, .F. ) ;
#20889 = CARTESIAN_POINT ( 'NONE',  ( 40.70731707320000226, -80.50000000000000000, -7.215414233289999757 ) ) ;
#20890 = CARTESIAN_POINT ( 'NONE',  ( -11.31667057079999950, -95.23931402160000914, -21.36056405359999744 ) ) ;
#20891 = AXIS2_PLACEMENT_3D ( 'NONE', #6695, #17615, #15556 ) ;
#20892 = CARTESIAN_POINT ( 'NONE',  ( -17.13033212710000086, -72.00000000000000000, 23.49748962700000021 ) ) ;
#20893 = DIRECTION ( 'NONE',  ( 0.4794255386042033384, 0.000000000000000000, 0.8775825618903726477 ) ) ;
#20894 = CARTESIAN_POINT ( 'NONE',  ( 7.540036301439999811, -101.3256028509999993, 14.00608922950000057 ) ) ;
#20895 = VERTEX_POINT ( 'NONE', #20866 ) ;
#20896 = CARTESIAN_POINT ( 'NONE',  ( -43.28927230711818197, -65.10052340106298630, -0.07634552800406639583 ) ) ;
#20897 = CARTESIAN_POINT ( 'NONE',  ( -28.75283265410000055, -92.49999846069999876, -2.687056279340000131 ) ) ;
#20898 = CARTESIAN_POINT ( 'NONE',  ( 11.40265797640000045, -97.01677120260001175, -17.81044358870000011 ) ) ;
#20899 = ORIENTED_EDGE ( 'NONE', *, *, #1043, .F. ) ;
#20900 = CARTESIAN_POINT ( 'NONE',  ( -27.04683438039999999, -74.00000000000000000, -36.23922253580000330 ) ) ;
#20901 = CARTESIAN_POINT ( 'NONE',  ( 0.000000000000000000, -92.50000000000000000, 0.000000000000000000 ) ) ;
#20902 = CARTESIAN_POINT ( 'NONE',  ( -2.631833427070000120, -26.03958238299999906, -24.12317078430000095 ) ) ;
#20903 = CARTESIAN_POINT ( 'NONE',  ( -17.40319643073701883, -92.71525149976336877, 25.04774006126359964 ) ) ;
#20904 = B_SPLINE_CURVE_WITH_KNOTS ( 'NONE', 3,
 ( #82, #17694, #13009, #17256, #6471, #8932 ),
 .UNSPECIFIED., .F., .F.,
 ( 4, 2, 4 ),
 ( 0.000000000000000000, 0.5000000000000000000, 1.000000000000000000 ),
 .UNSPECIFIED. ) ;
#20905 = CARTESIAN_POINT ( 'NONE',  ( 11.31764174110000098, -36.00000000000000000, -22.43277175240000076 ) ) ;
#20906 = EDGE_CURVE ( 'NONE', #17644, #16909, #2380, .T. ) ;
#20907 = CARTESIAN_POINT ( 'NONE',  ( 11.98259099005113804, -101.6407018583229274, -10.61142287496397074 ) ) ;
#20908 = CARTESIAN_POINT ( 'NONE',  ( 21.99751943120000064, -53.29445792020000283, -7.633405283620000148 ) ) ;
#20909 = CARTESIAN_POINT ( 'NONE',  ( 11.55429050816779224, -99.33527484956252351, 14.87222534504054039 ) ) ;
#20910 = CARTESIAN_POINT ( 'NONE',  ( -13.66168260340000096, -72.00000000000000000, -27.27344781959999764 ) ) ;
#20911 = ORIENTED_EDGE ( 'NONE', *, *, #16811, .F. ) ;
#20912 = TOROIDAL_SURFACE ( 'NONE', #21813, 18.14285714289999873, 0.5000000000000000000 ) ;
#20913 = VECTOR ( 'NONE', #17355, 1000.000000000000000 ) ;
#20914 = LINE ( 'NONE', #18287, #5945 ) ;
#20915 = DIRECTION ( 'NONE',  ( 0.000000000000000000, -1.000000000000000000, 0.000000000000000000 ) ) ;
#20916 = AXIS2_PLACEMENT_3D ( 'NONE', #21906, #3985, #6450 ) ;
#20917 = CARTESIAN_POINT ( 'NONE',  ( -11.44999862350000086, -95.17624356449999823, -21.38312836629999936 ) ) ;
#20918 = CARTESIAN_POINT ( 'NONE',  ( 21.23424069599999697, -35.30313414209999934, -7.936589188299999265 ) ) ;
#20919 = CARTESIAN_POINT ( 'NONE',  ( 23.34294251050530988, -60.17793182509785055, 10.47223221149565653 ) ) ;
#20920 = CARTESIAN_POINT ( 'NONE',  ( -7.539005773070000416, -98.58303758080000989, 17.10172281030000008 ) ) ;
#20921 = CARTESIAN_POINT ( 'NONE',  ( 11.44042105559999989, -101.2530993000000024, -9.998588429619998053 ) ) ;
#20922 = CARTESIAN_POINT ( 'NONE',  ( -0.1779554536940000098, -101.1889999979999999, -15.99901033990000165 ) ) ;
#20923 = FILL_AREA_STYLE ('',( #14220 ) ) ;
#20924 = VERTEX_POINT ( 'NONE', #14296 ) ;
#20925 = AXIS2_PLACEMENT_3D ( 'NONE', #23138, #3184, #5220 ) ;
#20926 = CARTESIAN_POINT ( 'NONE',  ( 30.67749406165812687, -74.17397605894404933, -24.28944146970528450 ) ) ;
#20927 = DIRECTION ( 'NONE',  ( 0.7071067811865475727, 0.000000000000000000, -0.7071067811865475727 ) ) ;
#20928 = VERTEX_POINT ( 'NONE', #14435 ) ;
#20929 = DIRECTION ( 'NONE',  ( 0.000000000000000000, -1.000000000000000000, 0.000000000000000000 ) ) ;
#20930 = CIRCLE ( 'NONE', #8326, 55.67692378859999991 ) ;
#20931 = VECTOR ( 'NONE', #14432, 1000.000000000000000 ) ;
#20932 = AXIS2_PLACEMENT_3D ( 'NONE', #24126, #24563, #4604 ) ;
#20933 = CARTESIAN_POINT ( 'NONE',  ( -0.09292153041354569987, -101.6484611540000174, -15.99995616405717413 ) ) ;
#20934 = FACE_OUTER_BOUND ( 'NONE', #21166, .T. ) ;
#20935 = CARTESIAN_POINT ( 'NONE',  ( -10.17458377400000025, -18.50000000000000000, -22.50859265919999785 ) ) ;
#20936 = CARTESIAN_POINT ( 'NONE',  ( 21.93840406509999852, -73.88712764410000489, -31.96455063700000210 ) ) ;
#20937 = LINE ( 'NONE', #23121, #9005 ) ;
#20938 = CARTESIAN_POINT ( 'NONE',  ( 23.88061036455241748, -92.84927079009761997, -18.97278372083326659 ) ) ;
#20939 = EDGE_CURVE ( 'NONE', #8616, #15112, #24193, .T. ) ;
#20940 = CARTESIAN_POINT ( 'NONE',  ( -11.93607363350000128, -70.93453115479999838, -26.12370071229999979 ) ) ;
#20941 = CARTESIAN_POINT ( 'NONE',  ( 8.807493968779999349, -25.53205038710000352, -20.04401236839999711 ) ) ;
#20942 = CARTESIAN_POINT ( 'NONE',  ( -2.353367408830994378, -57.44036977208730121, -24.34032937392296603 ) ) ;
#20943 = CARTESIAN_POINT ( 'NONE',  ( 7.990241584909999695, -34.99644672609999674, -21.18700924519999873 ) ) ;
#20944 = EDGE_LOOP ( 'NONE', ( #12911, #19244, #11117, #1842 ) ) ;
#20945 = ADVANCED_FACE ( 'NONE', ( #16179 ), #9767, .F. ) ;
#20946 = CARTESIAN_POINT ( 'NONE',  ( -40.33874795569358440, -63.33820666351654438, -2.216302165567395122 ) ) ;
#20947 = ORIENTED_EDGE ( 'NONE', *, *, #27516, .F. ) ;
#20948 = EDGE_CURVE ( 'NONE', #19815, #21547, #22858, .T. ) ;
#20949 = ADVANCED_FACE ( 'NONE', ( #3238 ), #5126, .T. ) ;
#20950 = TOROIDAL_SURFACE ( 'NONE', #20458, 7.750000000000000000, 0.5000000000000000000 ) ;
#20951 = CARTESIAN_POINT ( 'NONE',  ( -2.565531208409999930, -57.41946943429999806, -24.92671054230000038 ) ) ;
#20952 = B_SPLINE_CURVE_WITH_KNOTS ( 'NONE', 5,
 ( #5846, #26247, #1641, #23909, #3947, #12810 ),
 .UNSPECIFIED., .F., .F.,
 ( 6, 6 ),
 ( 0.000000000000000000, 1.000000000000000000 ),
 .UNSPECIFIED. ) ;
#20953 = CARTESIAN_POINT ( 'NONE',  ( -42.25000000000000000, -65.00000000000000000, 0.7216878364880000563 ) ) ;
#20954 = CARTESIAN_POINT ( 'NONE',  ( 1.436102896439999999, -94.52419709919999491, 23.97566704719999819 ) ) ;
#20955 = DIRECTION ( 'NONE',  ( 0.9704142011833034598, 0.000000000000000000, 0.2414462220490750377 ) ) ;
#20956 = ORIENTED_EDGE ( 'NONE', *, *, #2050, .F. ) ;
#20957 = CARTESIAN_POINT ( 'NONE',  ( -20.18078161143439786, -39.33785704641559278, 14.62338064274810634 ) ) ;
#20958 = CARTESIAN_POINT ( 'NONE',  ( -27.62030561685637409, -93.40025063768234759, 0.3680505982496029005 ) ) ;
#20959 = CARTESIAN_POINT ( 'NONE',  ( 22.08525036290000187, -37.96517279220000063, -8.883154216930000402 ) ) ;
#20960 = CARTESIAN_POINT ( 'NONE',  ( 5.115190889397799978, -93.00000166546709579, 28.53538671473107513 ) ) ;
#20961 = VERTEX_POINT ( 'NONE', #23471 ) ;
#20962 = CARTESIAN_POINT ( 'NONE',  ( 7.198781031971043021, -73.55869875168694705, -39.13694367198868918 ) ) ;
#20963 = DIRECTION ( 'NONE',  ( -1.000000000000000000, 0.000000000000000000, 0.000000000000000000 ) ) ;
#20964 = ORIENTED_EDGE ( 'NONE', *, *, #18509, .F. ) ;
#20965 = CARTESIAN_POINT ( 'NONE',  ( -14.43245924010000003, -80.10005509740000207, 36.56795405499999418 ) ) ;
#20966 = CARTESIAN_POINT ( 'NONE',  ( -3.669439427430000400, -72.55114739969998539, -28.40640588289999968 ) ) ;
#20967 = CARTESIAN_POINT ( 'NONE',  ( -16.03641129780000085, -70.40840182630000754, 23.20817888690000075 ) ) ;
#20968 = VERTEX_POINT ( 'NONE', #9483 ) ;
#20969 = CIRCLE ( 'NONE', #24679, 6.750000000000000000 ) ;
#20970 = DIRECTION ( 'NONE',  ( 0.000000000000000000, 1.000000000000000000, 0.000000000000000000 ) ) ;
#20971 = CARTESIAN_POINT ( 'NONE',  ( -15.59466818890000006, -100.7754213330000113, 2.827888207719999603 ) ) ;
#20972 = CARTESIAN_POINT ( 'NONE',  ( -20.21023039549999822, -62.10525983699999841, 13.01158141169999993 ) ) ;
#20973 = ORIENTED_EDGE ( 'NONE', *, *, #10612, .F. ) ;
#20974 = CYLINDRICAL_SURFACE ( 'NONE', #13879, 3.749999999999996447 ) ;
#20975 = CARTESIAN_POINT ( 'NONE',  ( -7.292785445180875570, -73.99991600666669456, 39.60658383038346386 ) ) ;
#20976 = CARTESIAN_POINT ( 'NONE',  ( 36.44118056271604189, -74.04359402117586342, -14.04216929337327713 ) ) ;
#20977 = ORIENTED_EDGE ( 'NONE', *, *, #5630, .F. ) ;
#20978 = EDGE_CURVE ( 'NONE', #25480, #24664, #18681, .T. ) ;
#20979 = CARTESIAN_POINT ( 'NONE',  ( -41.70814779298223129, -65.10234783419473104, -2.808123652670708736 ) ) ;
#20980 = CARTESIAN_POINT ( 'NONE',  ( 15.70469996677716829, -101.4085864807012882, 3.915613578189586441 ) ) ;
#20981 = CARTESIAN_POINT ( 'NONE',  ( 6.308882621499999566, -111.0000000000000000, -29.19167084780000110 ) ) ;
#20982 = ORIENTED_EDGE ( 'NONE', *, *, #13232, .T. ) ;
#20983 = ADVANCED_FACE ( 'NONE', ( #7472 ), #25634, .F. ) ;
#20984 = CARTESIAN_POINT ( 'NONE',  ( 36.94915360298272589, -79.79696885169119014, -14.35475846226867702 ) ) ;
#20985 = AXIS2_PLACEMENT_3D ( 'NONE', #27106, #15564, #24772 ) ;
#20986 = CARTESIAN_POINT ( 'NONE',  ( 25.01891871080000129, -68.13686112700000308, -8.889018148439999933 ) ) ;
#20987 = CARTESIAN_POINT ( 'NONE',  ( 5.988381294080164174, -93.48478527242041025, 26.68815097859544849 ) ) ;
#20988 = TOROIDAL_SURFACE ( 'NONE', #15842, 55.85192378860000417, 0.3499999999999999778 ) ;
#20989 = VERTEX_POINT ( 'NONE', #16332 ) ;
#20990 = VECTOR ( 'NONE', #16594, 1000.000000000000000 ) ;
#20991 = CARTESIAN_POINT ( 'NONE',  ( -41.75000000000000000, -65.21397798589998729, -2.551096136600000008 ) ) ;
#20992 = ORIENTED_EDGE ( 'NONE', *, *, #10543, .F. ) ;
#20993 = DIRECTION ( 'NONE',  ( 0.000000000000000000, -1.000000000000000000, 0.000000000000000000 ) ) ;
#20994 = CARTESIAN_POINT ( 'NONE',  ( -5.459548099580000091, -101.1364147039999892, 14.34189828759999941 ) ) ;
#20995 = ORIENTED_EDGE ( 'NONE', *, *, #4825, .F. ) ;
#20996 = DIRECTION ( 'NONE',  ( 0.000000000000000000, 0.000000000000000000, -1.000000000000000000 ) ) ;
#20997 = CARTESIAN_POINT ( 'NONE',  ( 40.70731707320000226, -74.50000000000000000, 7.215414233289999757 ) ) ;
#20998 = CARTESIAN_POINT ( 'NONE',  ( -11.17610348543527010, -19.46454334095421146, -19.00959556865977262 ) ) ;
#20999 = DIRECTION ( 'NONE',  ( 0.06892947544783696590, -0.9975499440283633890, -0.01195142600257996686 ) ) ;
#21000 = DIRECTION ( 'NONE',  ( 0.4794255386042059475, 0.000000000000000000, 0.8775825618903710934 ) ) ;
#21001 = CARTESIAN_POINT ( 'NONE',  ( 9.564509902230000193, -57.40875702419999982, -23.52622212079999997 ) ) ;
#21002 = ORIENTED_EDGE ( 'NONE', *, *, #4915, .F. ) ;
#21003 = CARTESIAN_POINT ( 'NONE',  ( -2.664535259099999805E-15, -72.82938648530000592, -3.552713678799999608E-15 ) ) ;
#21004 = CARTESIAN_POINT ( 'NONE',  ( 7.670973119660000172, -34.59820496239999699, -21.21808926809999818 ) ) ;
#21005 = FACE_OUTER_BOUND ( 'NONE', #23021, .T. ) ;
#21006 = DIRECTION ( 'NONE',  ( 0.000000000000000000, -1.000000000000000000, 0.000000000000000000 ) ) ;
#21007 = EDGE_LOOP ( 'NONE', ( #24025, #26050, #21759, #3538 ) ) ;
#21008 = ADVANCED_FACE ( 'NONE', ( #7618 ), #27601, .T. ) ;
#21009 = AXIS2_PLACEMENT_3D ( 'NONE', #8603, #8311, #23773 ) ;
#21010 = CARTESIAN_POINT ( 'NONE',  ( -0.7196032852779999933, -79.77560502979999058, 47.25024237019999873 ) ) ;
#21011 = CARTESIAN_POINT ( 'NONE',  ( -15.42363691649999957, -67.46051717960000360, 22.84488648889999851 ) ) ;
#21012 = VERTEX_POINT ( 'NONE', #20647 ) ;
#21013 = AXIS2_PLACEMENT_3D ( 'NONE', #23136, #9281, #12044 ) ;
#21014 = EDGE_CURVE ( 'NONE', #17168, #28456, #20515, .T. ) ;
#21015 = CARTESIAN_POINT ( 'NONE',  ( -40.50000000000000000, -12.50000000000000000, -4.500000000000000000 ) ) ;
#21016 = CIRCLE ( 'NONE', #4239, 57.75000000000000000 ) ;
#21017 = CARTESIAN_POINT ( 'NONE',  ( -19.20879816019999708, -32.73130089779999707, 11.71051500439999948 ) ) ;
#21018 = CARTESIAN_POINT ( 'NONE',  ( -33.25000000000000000, -69.50000000000000000, 5.481726184089999968E-15 ) ) ;
#21019 = CARTESIAN_POINT ( 'NONE',  ( 29.02377468160000262, -74.30612813009999229, -26.48574803420000023 ) ) ;
#21020 = AXIS2_PLACEMENT_3D ( 'NONE', #11432, #26908, #4757 ) ;
#21021 = CARTESIAN_POINT ( 'NONE',  ( -13.44405788329999929, -68.28990366489999531, 22.97003105929999833 ) ) ;
#21022 = EDGE_CURVE ( 'NONE', #3611, #25958, #14155, .T. ) ;
#21023 = CARTESIAN_POINT ( 'NONE',  ( 26.87922219139999669, -65.53745956530001138, 1.653266478199999945 ) ) ;
#21024 = CARTESIAN_POINT ( 'NONE',  ( -10.80821428159999975, -18.85485912780000106, 19.04257197200000107 ) ) ;
#21025 = ORIENTED_EDGE ( 'NONE', *, *, #19731, .F. ) ;
#21026 = AXIS2_PLACEMENT_3D ( 'NONE', #25437, #16673, #9965 ) ;
#21027 = CARTESIAN_POINT ( 'NONE',  ( 8.721287999440001215, -37.33944922460000271, -21.87060590859999820 ) ) ;
#21028 = FACE_OUTER_BOUND ( 'NONE', #14976, .T. ) ;
#21029 = CARTESIAN_POINT ( 'NONE',  ( 19.96641028149999997, -35.92495628129999830, -9.198931196760000262 ) ) ;
#21030 = FACE_OUTER_BOUND ( 'NONE', #22131, .T. ) ;
#21031 = ORIENTED_EDGE ( 'NONE', *, *, #19239, .T. ) ;
#21032 = CARTESIAN_POINT ( 'NONE',  ( -11.05730518689999897, -18.50000000000000000, -18.25363368680000065 ) ) ;
#21033 = DIRECTION ( 'NONE',  ( 1.000000000000000000, 0.000000000000000000, 0.000000000000000000 ) ) ;
#21034 = AXIS2_PLACEMENT_3D ( 'NONE', #8103, #23418, #6043 ) ;
#21035 = CIRCLE ( 'NONE', #7548, 24.50000000000000000 ) ;
#21036 = CARTESIAN_POINT ( 'NONE',  ( -15.42363691649999957, -67.46051717960000360, 22.84488648889999851 ) ) ;
#21037 = DIRECTION ( 'NONE',  ( 1.000000000000000000, 0.000000000000000000, 0.000000000000000000 ) ) ;
#21038 = DIRECTION ( 'NONE',  ( 1.000000000000000000, 0.000000000000000000, 0.000000000000000000 ) ) ;
#21039 = DIRECTION ( 'NONE',  ( 0.000000000000000000, -1.000000000000000000, 0.000000000000000000 ) ) ;
#21040 = ORIENTED_EDGE ( 'NONE', *, *, #1489, .F. ) ;
#21041 = CARTESIAN_POINT ( 'NONE',  ( -39.89765284886984631, -73.91187068862662102, 7.249313954218240319 ) ) ;
#21042 = DIRECTION ( 'NONE',  ( 0.000000000000000000, 1.000000000000000000, 0.000000000000000000 ) ) ;
#21043 = CARTESIAN_POINT ( 'NONE',  ( 10.91527628520000093, -97.01506441390000646, -17.67900200189999893 ) ) ;
#21044 = ORIENTED_EDGE ( 'NONE', *, *, #14765, .F. ) ;
#21045 = CARTESIAN_POINT ( 'NONE',  ( 18.93437244589999935, -18.87168146930000034, -8.901252599150000222 ) ) ;
#21046 = CARTESIAN_POINT ( 'NONE',  ( 11.51147269610000023, -101.1045726949999874, -10.43176325379999980 ) ) ;
#21047 = CARTESIAN_POINT ( 'NONE',  ( 19.97576656849999921, -19.50000000000000000, -19.97576656849999921 ) ) ;
#21048 = CARTESIAN_POINT ( 'NONE',  ( -17.27650544376518482, -92.75430643285494625, 25.13513460670969124 ) ) ;
#21049 = EDGE_CURVE ( 'NONE', #23834, #12597, #7955, .T. ) ;
#21050 = CARTESIAN_POINT ( 'NONE',  ( -2.481178842626576841, -74.00000000000000000, 46.81450634432220426 ) ) ;
#21051 = VECTOR ( 'NONE', #24195, 1000.000000000000000 ) ;
#21052 = DIRECTION ( 'NONE',  ( 0.000000000000000000, -1.000000000000000000, 0.000000000000000000 ) ) ;
#21053 = EDGE_CURVE ( 'NONE', #9393, #26809, #12582, .T. ) ;
#21054 = CARTESIAN_POINT ( 'NONE',  ( 13.30637309069069119, -98.37418017201852649, 15.04202739120032639 ) ) ;
#21055 = CARTESIAN_POINT ( 'NONE',  ( -16.13266937400000245, -84.75000000000000000, -29.53065320760000034 ) ) ;
#21056 = VERTEX_POINT ( 'NONE', #13480 ) ;
#21057 = CARTESIAN_POINT ( 'NONE',  ( -32.81694319320000375, -74.37394555080000202, -22.22457704239999998 ) ) ;
#21058 = CARTESIAN_POINT ( 'NONE',  ( 13.74596177532710151, -96.89152198108462244, -16.22606708551202459 ) ) ;
#21059 = CARTESIAN_POINT ( 'NONE',  ( 7.405704750090000843, -101.1273033739999931, 13.62605079230000094 ) ) ;
#21060 = CARTESIAN_POINT ( 'NONE',  ( -11.33452548760000056, -94.90396370949999039, -21.28272403569999938 ) ) ;
#21061 = FACE_OUTER_BOUND ( 'NONE', #15067, .T. ) ;
#21062 = CARTESIAN_POINT ( 'NONE',  ( 7.248542667680995422, -73.88534697533242479, 39.85457864244732917 ) ) ;
#21063 = CARTESIAN_POINT ( 'NONE',  ( -29.41500720700000215, -92.50000000000000000, 8.062713625770001613 ) ) ;
#21064 = FACE_OUTER_BOUND ( 'NONE', #14691, .T. ) ;
#21065 = CARTESIAN_POINT ( 'NONE',  ( 29.41275679339999982, -25.00000000000000000, 53.83969017199999740 ) ) ;
#21066 = AXIS2_PLACEMENT_3D ( 'NONE', #20642, #25309, #6940 ) ;
#21067 = EDGE_CURVE ( 'NONE', #13365, #20661, #20045, .T. ) ;
#21068 = FACE_OUTER_BOUND ( 'NONE', #28028, .T. ) ;
#21069 = ORIENTED_EDGE ( 'NONE', *, *, #3181, .T. ) ;
#21070 = CARTESIAN_POINT ( 'NONE',  ( -5.753106463249999969, -2.000000000000000000, -10.53099074269999846 ) ) ;
#21071 = CARTESIAN_POINT ( 'NONE',  ( -32.25000000000000000, -73.50000000000000000, 2.464695114664749979E-15 ) ) ;
#21072 = ORIENTED_EDGE ( 'NONE', *, *, #25987, .F. ) ;
#21073 = CARTESIAN_POINT ( 'NONE',  ( 7.215414233289999757, -74.50000000000000000, -40.70731707320000226 ) ) ;
#21074 = CARTESIAN_POINT ( 'NONE',  ( 0.4632353614598325175, -101.2111896145273988, -16.33269620291778423 ) ) ;
#21075 = CARTESIAN_POINT ( 'NONE',  ( -11.72000839801819616, -19.46749782351740876, 19.06227229943159429 ) ) ;
#21076 = CARTESIAN_POINT ( 'NONE',  ( -7.280256974170000284, -74.15866376920000391, 39.93430878389999350 ) ) ;
#21077 = CARTESIAN_POINT ( 'NONE',  ( 13.20251034797960799, -92.82709422631791085, 27.49443084435448981 ) ) ;
#21078 = CARTESIAN_POINT ( 'NONE',  ( 3.768036230260000150E-15, -69.50000000000000000, 40.00000000000000000 ) ) ;
#21079 = DIRECTION ( 'NONE',  ( 0.000000000000000000, -1.000000000000000000, 0.000000000000000000 ) ) ;
#21080 = EDGE_CURVE ( 'NONE', #19454, #8492, #23767, .T. ) ;
#21081 = ADVANCED_FACE ( 'NONE', ( #10388 ), #14317, .T. ) ;
#21082 = CARTESIAN_POINT ( 'NONE',  ( 10.69287703170000015, -70.89709150720000252, -26.27243468539999682 ) ) ;
#21083 = CARTESIAN_POINT ( 'NONE',  ( 12.94735060620000056, -94.70873613630000420, -19.84317021230000222 ) ) ;
#21084 = B_SPLINE_SURFACE_WITH_KNOTS ( 'NONE', 5, 5, ( 
 ( #14469, #12536, #17071, #21045, #27868, #28015 ),
 ( #27611, #16652, #8185, #23775, #3817, #9804 ),
 ( #21453, #23363, #19125, #18714, #21311, #5584 ),
 ( #7651, #19263, #1102, #3405, #10350, #16519 ),
 ( #9943, #25693, #1509, #25414, #5718, #1364 ),
 ( #5446, #14330, #23224, #18858, #14737, #14602 ) ),
 .UNSPECIFIED., .F., .F., .F.,
 ( 6, 6 ),
 ( 6, 6 ),
 ( 0.000000000000000000, 2.292501860869999852 ),
 ( 0.000000000000000000, 1.000000000000000000 ),
 .UNSPECIFIED. ) ;
#21085 = CARTESIAN_POINT ( 'NONE',  ( -6.665307709260000379, -93.00000000000000000, -13.13558364449999871 ) ) ;
#21086 = LINE ( 'NONE', #16557, #6576 ) ;
#21087 = CARTESIAN_POINT ( 'NONE',  ( -42.25000000000000000, -63.30468293320000583, -0.7216878364880000563 ) ) ;
#21088 = CARTESIAN_POINT ( 'NONE',  ( -4.500000000000000000, -15.00000000000000000, 50.00000000000000000 ) ) ;
#21089 = ORIENTED_EDGE ( 'NONE', *, *, #1151, .F. ) ;
#21090 = CARTESIAN_POINT ( 'NONE',  ( 9.173959622430000849, -111.0000000000000000, -19.14607041020000011 ) ) ;
#21091 = AXIS2_PLACEMENT_3D ( 'NONE', #1587, #27952, #10426 ) ;
#21092 = AXIS2_PLACEMENT_3D ( 'NONE', #3498, #19216, #21266 ) ;
#21093 = EDGE_LOOP ( 'NONE', ( #27234, #6805, #3484, #2074 ) ) ;
#21094 = AXIS2_PLACEMENT_3D ( 'NONE', #27564, #16470, #14285 ) ;
#21095 = DIRECTION ( 'NONE',  ( 0.000000000000000000, 1.000000000000000000, 0.000000000000000000 ) ) ;
#21096 = DIRECTION ( 'NONE',  ( 1.110223024630000146E-15, 0.000000000000000000, -1.000000000000000000 ) ) ;
#21097 = CARTESIAN_POINT ( 'NONE',  ( 9.396870180011182683, -94.80026864434297806, -22.54656979151466345 ) ) ;
#21098 = ORIENTED_EDGE ( 'NONE', *, *, #23358, .T. ) ;
#21099 = ADVANCED_FACE ( 'NONE', ( #9841 ), #7072, .F. ) ;
#21100 = AXIS2_PLACEMENT_3D ( 'NONE', #12377, #12516, #1344 ) ;
#21101 = FACE_OUTER_BOUND ( 'NONE', #14780, .T. ) ;
#21102 = EDGE_CURVE ( 'NONE', #19985, #1588, #977, .T. ) ;
#21103 = FACE_OUTER_BOUND ( 'NONE', #28056, .T. ) ;
#21104 = ORIENTED_EDGE ( 'NONE', *, *, #14240, .T. ) ;
#21105 = LINE ( 'NONE', #12328, #7625 ) ;
#21106 = CARTESIAN_POINT ( 'NONE',  ( 8.189694586359999917, -36.39795110199999328, -21.29668027459999990 ) ) ;
#21107 = CARTESIAN_POINT ( 'NONE',  ( -14.59815773839999942, -79.49999996000001090, 36.63377407710000000 ) ) ;
#21108 = EDGE_CURVE ( 'NONE', #17563, #2951, #8420, .T. ) ;
#21109 = AXIS2_PLACEMENT_3D ( 'NONE', #5675, #28378, #6234 ) ;
#21110 = DIRECTION ( 'NONE',  ( -0.5423995371861327630, 0.000000000000000000, 0.8401206711302066088 ) ) ;
#21111 = ORIENTED_EDGE ( 'NONE', *, *, #13073, .F. ) ;
#21112 = CARTESIAN_POINT ( 'NONE',  ( -15.74743825989999912, -100.6638977829999959, 2.772596425819999766 ) ) ;
#21113 = CARTESIAN_POINT ( 'NONE',  ( 23.98000230750000128, -62.12717499380000419, -0.2704306557409999479 ) ) ;
#21114 = CARTESIAN_POINT ( 'NONE',  ( -20.17414664320000028, -60.59603168650000526, 12.28933892000000050 ) ) ;
#21115 = EDGE_LOOP ( 'NONE', ( #2446, #24120, #24298, #25875, #4802, #24476, #6964 ) ) ;
#21116 = CARTESIAN_POINT ( 'NONE',  ( 23.74273760109999998, -65.04364753569998925, -8.271557007380000215 ) ) ;
#21117 = CARTESIAN_POINT ( 'NONE',  ( -1.803985702539999902, -19.15979404320000157, -22.30692425470000373 ) ) ;
#21118 = CARTESIAN_POINT ( 'NONE',  ( 24.21290647080000369, -92.68283714880000446, -13.91082074250000034 ) ) ;
#21119 = EDGE_LOOP ( 'NONE', ( #8586, #25792, #19330, #22959 ) ) ;
#21120 = CIRCLE ( 'NONE', #23886, 0.8000000000000003775 ) ;
#21121 = CARTESIAN_POINT ( 'NONE',  ( -41.52394852252965762, -65.11704020645255753, -2.883441032528796022 ) ) ;
#21122 = CARTESIAN_POINT ( 'NONE',  ( 36.78261483260000375, -79.80697408650000568, -14.39505880960000006 ) ) ;
#21123 = CARTESIAN_POINT ( 'NONE',  ( 19.58569043503641893, -94.54719627015504102, 13.61988836429140903 ) ) ;
#21124 = ORIENTED_EDGE ( 'NONE', *, *, #8663, .F. ) ;
#21125 = UNCERTAINTY_MEASURE_WITH_UNIT (LENGTH_MEASURE( 1.000000000000000082E-05 ), #27847, 'distance_accuracy_value', 'NONE');
#21126 = FACE_OUTER_BOUND ( 'NONE', #14808, .T. ) ;
#21127 = LINE ( 'NONE', #14415, #1773 ) ;
#21128 = ORIENTED_EDGE ( 'NONE', *, *, #81, .F. ) ;
#21129 = DIRECTION ( 'NONE',  ( 0.000000000000000000, -1.000000000000000000, 0.000000000000000000 ) ) ;
#21130 = CARTESIAN_POINT ( 'NONE',  ( -17.81659886998984987, -98.83160744532767694, 4.274644831898003261 ) ) ;
#21131 = ORIENTED_EDGE ( 'NONE', *, *, #2045, .T. ) ;
#21132 = CARTESIAN_POINT ( 'NONE',  ( -12.50408296909999883, -42.25464550570000455, 19.83474686469999781 ) ) ;
#21133 = CARTESIAN_POINT ( 'NONE',  ( -5.832419616270000162, -101.1848541600000004, 14.12653895319999897 ) ) ;
#21134 = ORIENTED_EDGE ( 'NONE', *, *, #23513, .F. ) ;
#21135 = PRODUCT_RELATED_PRODUCT_CATEGORY ( 'part', '', ( #2252 ) ) ;
#21136 = CARTESIAN_POINT ( 'NONE',  ( 9.726843560609999884, -36.00000000000000000, -20.21912206349999863 ) ) ;
#21137 = ADVANCED_FACE ( 'NONE', ( #1970 ), #86, .T. ) ;
#21138 = AXIS2_PLACEMENT_3D ( 'NONE', #1552, #1688, #3999 ) ;
#21139 = CIRCLE ( 'NONE', #8100, 13.00000000000000178 ) ;
#21140 = CARTESIAN_POINT ( 'NONE',  ( 38.70548920639999579, -73.81415963839999961, 7.196176986149999344 ) ) ;
#21141 = CARTESIAN_POINT ( 'NONE',  ( 23.48647081097517741, -94.80026864429605382, -6.710787388611177740 ) ) ;
#21142 = ADVANCED_FACE ( 'NONE', ( #26151 ), #1048, .F. ) ;
#21143 = CARTESIAN_POINT ( 'NONE',  ( 19.94173275869999884, -39.36577621580000397, 10.90498865049999822 ) ) ;
#21144 = CARTESIAN_POINT ( 'NONE',  ( 47.07870869154496063, -79.56040629918834384, -1.981086625768881060 ) ) ;
#21145 = ORIENTED_EDGE ( 'NONE', *, *, #28485, .T. ) ;
#21146 = EDGE_CURVE ( 'NONE', #24982, #13659, #23327, .T. ) ;
#21147 = CARTESIAN_POINT ( 'NONE',  ( -32.45231784149999754, -80.07464407599999845, -22.38373082789999913 ) ) ;
#21148 = CARTESIAN_POINT ( 'NONE',  ( 7.292753731799999528, -92.50000000000000000, -29.01615345709999971 ) ) ;
#21149 = CARTESIAN_POINT ( 'NONE',  ( -20.22326673870000135, -94.79581125309999834, 12.30737463699999878 ) ) ;
#21150 = DIRECTION ( 'NONE',  ( 1.000000000000000000, 0.000000000000000000, 0.000000000000000000 ) ) ;
#21151 = ORIENTED_EDGE ( 'NONE', *, *, #27436, .T. ) ;
#21152 =( GEOMETRIC_REPRESENTATION_CONTEXT ( 3 ) GLOBAL_UNCERTAINTY_ASSIGNED_CONTEXT ( ( #11187 ) ) GLOBAL_UNIT_ASSIGNED_CONTEXT ( ( #6355, #19467, #8387 ) ) REPRESENTATION_CONTEXT ( 'NONE', 'WORKASPACE' ) );
#21153 = CARTESIAN_POINT ( 'NONE',  ( 14.31067154247732098, -98.53908159006914502, -12.11011490584104600 ) ) ;
#21154 = DIRECTION ( 'NONE',  ( 0.000000000000000000, -1.000000000000000000, 0.000000000000000000 ) ) ;
#21155 = ORIENTED_EDGE ( 'NONE', *, *, #12479, .T. ) ;
#21156 = DIRECTION ( 'NONE',  ( 1.000000000000000000, 0.000000000000000000, 0.000000000000000000 ) ) ;
#21157 = CARTESIAN_POINT ( 'NONE',  ( 0.000000000000000000, -19.09689110869999951, 0.000000000000000000 ) ) ;
#21158 = CARTESIAN_POINT ( 'NONE',  ( 19.51011835330500688, -98.16872834563331196, 2.367675478629094332 ) ) ;
#21159 = CARTESIAN_POINT ( 'NONE',  ( 30.95803130440000217, -72.48673634319999337, -21.93485012370000220 ) ) ;
#21160 = CARTESIAN_POINT ( 'NONE',  ( -13.82310862920000005, -74.00000000000000000, 36.20061004769999613 ) ) ;
#21161 = AXIS2_PLACEMENT_3D ( 'NONE', #22827, #3299, #10102 ) ;
#21162 = ORIENTED_EDGE ( 'NONE', *, *, #21508, .T. ) ;
#21163 = CARTESIAN_POINT ( 'NONE',  ( -39.90536558174056836, -73.91587151486801588, -7.249694362034283301 ) ) ;
#21164 = CARTESIAN_POINT ( 'NONE',  ( 21.70178022940000062, -37.60290983899999873, -8.323168728980000708 ) ) ;
#21165 = LINE ( 'NONE', #12944, #1416 ) ;
#21166 = EDGE_LOOP ( 'NONE', ( #7863, #13474, #8443, #4948 ) ) ;
#21167 = AXIS2_PLACEMENT_3D ( 'NONE', #22658, #11554, #20463 ) ;
#21168 = CARTESIAN_POINT ( 'NONE',  ( 46.96755458150000351, -74.27975760209999123, -2.596029696810000065 ) ) ;
#21169 = EDGE_CURVE ( 'NONE', #12297, #16695, #27003, .T. ) ;
#21170 = CARTESIAN_POINT ( 'NONE',  ( -16.35365950510000133, -70.21389208120000092, 23.31707131299999958 ) ) ;
#21171 = AXIS2_PLACEMENT_3D ( 'NONE', #9125, #18026, #9275 ) ;
#21172 = PRESENTATION_STYLE_ASSIGNMENT (( #27735 ) ) ;
#21173 = CARTESIAN_POINT ( 'NONE',  ( 9.205819528820001096, -44.88560226490000105, -22.58640054960000043 ) ) ;
#21174 = CARTESIAN_POINT ( 'NONE',  ( 7.466414723079999760, -101.1716783170000014, 13.84943005919999948 ) ) ;
#21175 = EDGE_LOOP ( 'NONE', ( #24626, #19578, #8926, #9484 ) ) ;
#21176 = ADVANCED_FACE ( 'NONE', ( #15480 ), #28320, .T. ) ;
#21177 = CARTESIAN_POINT ( 'NONE',  ( -43.27242786852578860, -65.10974319587900538, 0.1023444634918562884 ) ) ;
#21178 = PLANE ( 'NONE',  #3328 ) ;
#21179 = CARTESIAN_POINT ( 'NONE',  ( 26.85539570430000111, -72.18744871750000414, 10.61487170320000040 ) ) ;
#21180 = ORIENTED_EDGE ( 'NONE', *, *, #16278, .F. ) ;
#21181 = AXIS2_PLACEMENT_3D ( 'NONE', #11991, #27467, #7513 ) ;
#21182 = LINE ( 'NONE', #28151, #11309 ) ;
#21183 = CARTESIAN_POINT ( 'NONE',  ( 11.77685286379999852, -101.1716782080000030, -10.43412980439999949 ) ) ;
#21184 = CARTESIAN_POINT ( 'NONE',  ( -14.01103650240000142, -74.00781516410000904, 36.37014139069999885 ) ) ;
#21185 = CARTESIAN_POINT ( 'NONE',  ( -41.68172601867422600, -63.05366291735987971, -2.839252009386262543 ) ) ;
#21186 = B_SPLINE_CURVE_WITH_KNOTS ( 'NONE', 3,
 ( #19483, #6082, #12771, #3768, #1459, #8265, #21400, #10300, #7637, #19211 ),
 .UNSPECIFIED., .F., .F.,
 ( 4, 2, 2, 2, 4 ),
 ( 0.000000000000000000, 0.2500000000000000000, 0.5000000000000000000, 0.7500000000000000000, 1.000000000000000000 ),
 .UNSPECIFIED. ) ;
#21187 = CARTESIAN_POINT ( 'NONE',  ( -7.879410208250000380, -101.1889999979999999, 15.46934584979999983 ) ) ;
#21188 = LINE ( 'NONE', #12278, #1190 ) ;
#21189 = CARTESIAN_POINT ( 'NONE',  ( 7.460698725479999927E-15, -73.50000000000000000, 40.00000000000000000 ) ) ;
#21190 = CARTESIAN_POINT ( 'NONE',  ( 22.07739135919999640, -36.53304298639999814, -8.940781203140000244 ) ) ;
#21191 = CARTESIAN_POINT ( 'NONE',  ( 7.936589523444843586, -35.30313553310306673, -21.23424061165941623 ) ) ;
#21192 = EDGE_LOOP ( 'NONE', ( #23924, #7565, #24892, #3096, #24223, #1558 ) ) ;
#21193 = CYLINDRICAL_SURFACE ( 'NONE', #21768, 34.89999999999999858 ) ;
#21194 = CARTESIAN_POINT ( 'NONE',  ( 13.86691431120587126, -97.38870237776961858, -15.27021487312774717 ) ) ;
#21195 = AXIS2_PLACEMENT_3D ( 'NONE', #19801, #21854, #19943 ) ;
#21196 = LINE ( 'NONE', #10089, #26562 ) ;
#21197 = FACE_OUTER_BOUND ( 'NONE', #18022, .T. ) ;
#21198 = CARTESIAN_POINT ( 'NONE',  ( 7.224658177529891034, -73.64797963444465267, 39.39373284322624613 ) ) ;
#21199 = CARTESIAN_POINT ( 'NONE',  ( -12.24789267329999909, -65.07443093669999712, 21.96586363990000024 ) ) ;
#21200 = DIRECTION ( 'NONE',  ( 0.4794255386042000078, 0.000000000000000000, 0.8775825618903743131 ) ) ;
#21201 = DIRECTION ( 'NONE',  ( 0.000000000000000000, 1.000000000000000000, 0.000000000000000000 ) ) ;
#21202 = EDGE_CURVE ( 'NONE', #22268, #1488, #12598, .T. ) ;
#21203 = CARTESIAN_POINT ( 'NONE',  ( 19.70171045420000056, -28.58309623110000075, -8.968814305740000492 ) ) ;
#21204 = DIRECTION ( 'NONE',  ( 0.3889993898738998701, 0.000000000000000000, 0.9212380119587628702 ) ) ;
#21205 = ORIENTED_EDGE ( 'NONE', *, *, #15750, .F. ) ;
#21206 = CARTESIAN_POINT ( 'NONE',  ( -32.38674382290000153, -80.50000054920000991, -22.17565024390000161 ) ) ;
#21207 = CARTESIAN_POINT ( 'NONE',  ( -17.00715350810000004, -99.92967601899998442, 3.484608414699999823 ) ) ;
#21208 = EDGE_LOOP ( 'NONE', ( #23342, #4478, #24756, #3242, #16066, #4616, #13542, #13873, #5205 ) ) ;
#21209 = DIRECTION ( 'NONE',  ( 0.000000000000000000, -1.000000000000000000, 0.000000000000000000 ) ) ;
#21210 = VERTEX_POINT ( 'NONE', #17405 ) ;
#21211 = CARTESIAN_POINT ( 'NONE',  ( 0.2236201771617485901, -101.5026031439579839, -16.11104727832875483 ) ) ;
#21212 = CARTESIAN_POINT ( 'NONE',  ( 20.06309728629999967, -36.00000015629999695, -9.476130053229999461 ) ) ;
#21213 = CARTESIAN_POINT ( 'NONE',  ( -7.320980735620000068, -73.89975593090001382, 38.91827670650000215 ) ) ;
#21214 = CIRCLE ( 'NONE', #16077, 0.4999999999999982236 ) ;
#21215 = CARTESIAN_POINT ( 'NONE',  ( -13.16778131023122000, -93.19477818465753671, -23.58326779864327705 ) ) ;
#21216 = DIRECTION ( 'NONE',  ( 0.4794255386042041156, 0.000000000000000000, 0.8775825618903722036 ) ) ;
#21217 = DIRECTION ( 'NONE',  ( 0.000000000000000000, 1.000000000000000000, 0.000000000000000000 ) ) ;
#21218 = CARTESIAN_POINT ( 'NONE',  ( 11.15108825559999950, -100.9197081840000010, -10.94438638200000113 ) ) ;
#21219 = CARTESIAN_POINT ( 'NONE',  ( 13.01745538959999848, -101.1889999979999999, -10.62006851110000127 ) ) ;
#21220 = PLANE ( 'NONE',  #26336 ) ;
#21221 = CARTESIAN_POINT ( 'NONE',  ( -41.51159121739436131, -63.06523941402172539, 2.884620168996051337 ) ) ;
#21222 = ORIENTED_EDGE ( 'NONE', *, *, #201, .F. ) ;
#21223 = CARTESIAN_POINT ( 'NONE',  ( 0.000000000000000000, -17.50000000000000000, 0.000000000000000000 ) ) ;
#21224 = EDGE_CURVE ( 'NONE', #11679, #21931, #3024, .T. ) ;
#21225 = ORIENTED_EDGE ( 'NONE', *, *, #26512, .F. ) ;
#21226 = CARTESIAN_POINT ( 'NONE',  ( -7.713029007999999465, -80.50000000000000000, 40.75609756099999714 ) ) ;
#21227 = CARTESIAN_POINT ( 'NONE',  ( -28.30453570960000320, -92.90721294769998906, 1.613063908820000059 ) ) ;
#21228 = CARTESIAN_POINT ( 'NONE',  ( 8.831064126840001194, -94.59276292389999696, -22.09756266850000017 ) ) ;
#21229 = B_SPLINE_CURVE_WITH_KNOTS ( 'NONE', 3,
 ( #8842, #22828, #27338, #9689, #27492, #1542, #18887, #12431, #25995, #12162, #21075, #14494, #26430, #2111, #11086, #15627, #4563, #10808, #5002, #7348, #20757, #25276, #11545, #22503, #9369, #14191, #14327, #9940, #10347, #28012, #19260, #5442, #9801, #7648, #23360 ),
 .UNSPECIFIED., .F., .F.,
 ( 4, 2, 2, 2, 2, 2, 2, 1, 1, 2, 2, 2, 2, 1, 1, 1, 2, 2, 2, 4 ),
 ( 0.000000000000000000, 0.1249999999999843459, 0.1874999999999762412, 0.2187499999999721889, 0.2499999999999681366, 0.3749999999999550360, 0.4374999999999479305, 0.4687499999999432676, 0.4843749999999405476, 0.4921874999999385492, 0.4999999999999364952, 0.6249999999999171774, 0.6874999999999090727, 0.7187499999999044098, 0.7343749999999011902, 0.7421874999998999689, 0.7460937499999003020, 0.7499999999999007461, 0.8749999999999503730, 1.000000000000000000 ),
 .UNSPECIFIED. ) ;
#21230 = EDGE_CURVE ( 'NONE', #7597, #5628, #25952, .T. ) ;
#21231 = ADVANCED_FACE ( 'NONE', ( #15777 ), #22884, .T. ) ;
#21232 = EDGE_LOOP ( 'NONE', ( #10062, #774, #17277, #9622 ) ) ;
#21233 = CARTESIAN_POINT ( 'NONE',  ( -38.44999999999999574, -65.00000000000000000, 2.684678751729999480 ) ) ;
#21234 = EDGE_LOOP ( 'NONE', ( #4556, #1772, #12477, #11453 ) ) ;
#21235 = CIRCLE ( 'NONE', #16104, 0.5000000000000004441 ) ;
#21236 = CARTESIAN_POINT ( 'NONE',  ( -32.39999999999999858, -82.50000000000000000, 0.000000000000000000 ) ) ;
#21237 = CARTESIAN_POINT ( 'NONE',  ( 8.002629315070000970, -36.69307580889999798, -21.43727073079999812 ) ) ;
#21238 = CARTESIAN_POINT ( 'NONE',  ( -14.78710422270000002, -79.49999982570000157, 36.35833235879999847 ) ) ;
#21239 = CARTESIAN_POINT ( 'NONE',  ( 24.58039951800000011, -93.96464232159999597, -3.979621713999999866 ) ) ;
#21240 = CARTESIAN_POINT ( 'NONE',  ( -7.593125501599999438, -94.98812477769999418, -22.45811160230000070 ) ) ;
#21241 = ORIENTED_EDGE ( 'NONE', *, *, #17334, .F. ) ;
#21242 = CARTESIAN_POINT ( 'NONE',  ( -14.77962994559999999, -101.1130182370000057, 4.416924883319999218 ) ) ;
#21243 = CARTESIAN_POINT ( 'NONE',  ( -15.53707292570000043, -101.0215274990000012, 3.216537776050000019 ) ) ;
#21244 = CARTESIAN_POINT ( 'NONE',  ( -32.20753451023040270, -74.02757818730215433, -22.07633857551952161 ) ) ;
#21245 = CARTESIAN_POINT ( 'NONE',  ( 19.43643804750000115, -34.66800313659999944, -8.988996126470000902 ) ) ;
#21246 = B_SPLINE_SURFACE_WITH_KNOTS ( 'NONE', 5, 5, ( 
 ( #14008, #2953, #11816, #20729, #788, #5274, #14161, #8386, #28355 ),
 ( #3749, #14940, #17145, #22105, #12612, #26470, #17293, #10421, #21802 ),
 ( #23846, #28082, #15217, #14805, #24281, #24132, #4168, #13195, #23990 ),
 ( #19338, #1858, #6061, #23705, #13045, #10550, #21956, #2004, #8536 ),
 ( #26182, #10845, #19466, #28640, #19754, #6213, #12886, #17582, #1580 ),
 ( #8249, #8118, #21523, #6506, #28214, #26033, #15367, #17441, #4322 ),
 ( #19193, #17007, #3887, #10284, #6354, #25896, #15082, #5921, #28500 ),
 ( #1712, #12752, #21664, #4025, #19615, #26328, #15670, #13335, #24573 ),
 ( #6657, #276, #22397, #6957, #19899, #26777, #15520, #4613, #8817 ),
 ( #13488, #11297, #18019, #2443, #15819, #20056, #11137, #13937, #9118 ),
 ( #7247, #26917, #24731, #4766, #2593, #24430, #13641, #8971, #2145 ),
 ( #22549, #20346, #415, #9265, #4468, #7106, #22688, #15968, #18319 ) ),
 .UNSPECIFIED., .F., .F., .F.,
 ( 6, 3, 3, 6 ),
 ( 6, 3, 6 ),
 ( 3.852920539469999905, 4.834764074420000668, 6.134713715050000182, 8.383984506250000024 ),
 ( 0.000000000000000000, 0.2500000000000000000, 0.5000000000000000000 ),
 .UNSPECIFIED. ) ;
#21247 = VERTEX_POINT ( 'NONE', #24832 ) ;
#21248 = DIRECTION ( 'NONE',  ( 0.000000000000000000, 1.000000000000000000, 0.000000000000000000 ) ) ;
#21249 = CARTESIAN_POINT ( 'NONE',  ( -2.640725192390000142, -18.61940624680000056, -22.57500579379999905 ) ) ;
#21250 = CARTESIAN_POINT ( 'NONE',  ( 36.42998798566536323, -74.03894771716547041, -14.02638628026671164 ) ) ;
#21251 = EDGE_LOOP ( 'NONE', ( #10339, #7168, #10895, #12539 ) ) ;
#21252 = EDGE_CURVE ( 'NONE', #22701, #8141, #14480, .T. ) ;
#21253 = EDGE_CURVE ( 'NONE', #25637, #618, #9373, .T. ) ;
#21254 = CARTESIAN_POINT ( 'NONE',  ( 30.97576656850000276, -55.50000000000000000, -19.97576656849999921 ) ) ;
#21255 = CARTESIAN_POINT ( 'NONE',  ( 8.988513471540001021, -34.97532534249999259, -19.44627031849999810 ) ) ;
#21256 = CARTESIAN_POINT ( 'NONE',  ( 7.135467526410000261, -73.65707963269998970, 38.71641004229999794 ) ) ;
#21257 = EDGE_LOOP ( 'NONE', ( #25828, #1904, #24048, #23768 ) ) ;
#21258 = CARTESIAN_POINT ( 'NONE',  ( 6.729516044911419748, -100.6338045028395953, 15.38746398300566298 ) ) ;
#21259 = CARTESIAN_POINT ( 'NONE',  ( -0.6093759117718606788, -79.73250874465735194, 47.22473603108858953 ) ) ;
#21260 = ORIENTED_EDGE ( 'NONE', *, *, #21552, .T. ) ;
#21261 = CARTESIAN_POINT ( 'NONE',  ( 47.25000000000000000, -75.00000000000000000, -1.242228542250000064E-12 ) ) ;
#21262 = EDGE_LOOP ( 'NONE', ( #20691, #15418, #17361, #9923 ) ) ;
#21263 = CARTESIAN_POINT ( 'NONE',  ( 27.47009838660000014, -93.04780275979999260, 9.761662582170000491 ) ) ;
#21264 = CARTESIAN_POINT ( 'NONE',  ( -5.991572043530000613, -101.1499348409999897, 14.56695843900000042 ) ) ;
#21265 = ORIENTED_EDGE ( 'NONE', *, *, #25295, .F. ) ;
#21266 = DIRECTION ( 'NONE',  ( 0.4794255386042040601, 0.000000000000000000, 0.8775825618903719816 ) ) ;
#21267 = DIRECTION ( 'NONE',  ( 0.000000000000000000, 0.000000000000000000, -1.000000000000000000 ) ) ;
#21268 = B_SPLINE_CURVE_WITH_KNOTS ( 'NONE', 3,
 ( #24899, #20227, #4930, #24754 ),
 .UNSPECIFIED., .F., .F.,
 ( 4, 4 ),
 ( 0.000000000000000000, 1.000000000000000000 ),
 .UNSPECIFIED. ) ;
#21269 = CARTESIAN_POINT ( 'NONE',  ( 39.69297836850000039, -73.74954830100000436, 7.260231713059999592 ) ) ;
#21270 = DIRECTION ( 'NONE',  ( -0.4794255386042028944, 0.000000000000000000, 0.8775825618903727587 ) ) ;
#21271 = DIRECTION ( 'NONE',  ( 0.000000000000000000, -1.000000000000000000, 0.000000000000000000 ) ) ;
#21272 = ORIENTED_EDGE ( 'NONE', *, *, #22372, .T. ) ;
#21273 = CARTESIAN_POINT ( 'NONE',  ( 26.46310988749999993, -64.24504445130001784, 1.532420830840000026 ) ) ;
#21274 = DIRECTION ( 'NONE',  ( 0.000000000000000000, -1.000000000000000000, 0.000000000000000000 ) ) ;
#21275 = CARTESIAN_POINT ( 'NONE',  ( -20.31500103569999993, -92.75885976620000406, 18.51637639279999803 ) ) ;
#21276 = CARTESIAN_POINT ( 'NONE',  ( 24.26460669609999954, -92.67327634539999792, -13.69605124519999961 ) ) ;
#21277 = ORIENTED_EDGE ( 'NONE', *, *, #7324, .T. ) ;
#21278 = CARTESIAN_POINT ( 'NONE',  ( -2.677516332570000006E-13, -79.50000000000000000, 47.25000000000000000 ) ) ;
#21279 = CARTESIAN_POINT ( 'NONE',  ( -14.70960788549999876, -64.89138858019998679, 22.30467294780000032 ) ) ;
#21280 = ORIENTED_EDGE ( 'NONE', *, *, #23702, .F. ) ;
#21281 = LINE ( 'NONE', #19098, #18814 ) ;
#21282 = DIRECTION ( 'NONE',  ( 1.000000000000000000, 0.000000000000000000, 0.000000000000000000 ) ) ;
#21283 = CARTESIAN_POINT ( 'NONE',  ( -4.314829847440000421, -17.50000000000000000, -7.898243057010000179 ) ) ;
#21284 = FACE_OUTER_BOUND ( 'NONE', #4823, .T. ) ;
#21285 = CARTESIAN_POINT ( 'NONE',  ( -14.29601107782766611, -74.04677398807629629, 36.24402428269467435 ) ) ;
#21286 = EDGE_CURVE ( 'NONE', #28264, #3937, #20771, .T. ) ;
#21287 = COLOUR_RGB ( '', 0.72549020, 0.75294118, 0.79215686) ;
#21288 =( NAMED_UNIT ( * ) PLANE_ANGLE_UNIT ( ) SI_UNIT ( $, .RADIAN. ) );
#21289 = DIRECTION ( 'NONE',  ( 1.000000000000000000, 0.000000000000000000, 0.000000000000000000 ) ) ;
#21290 = ADVANCED_FACE ( 'NONE', ( #3678 ), #22406, .T. ) ;
#21291 = CIRCLE ( 'NONE', #3158, 0.3500000000000003664 ) ;
#21292 = ADVANCED_FACE ( 'NONE', ( #21315 ), #25550, .T. ) ;
#21293 = ORIENTED_EDGE ( 'NONE', *, *, #25177, .T. ) ;
#21294 = CARTESIAN_POINT ( 'NONE',  ( 20.52569424749999882, -35.38531401670000065, -8.770435444200000319 ) ) ;
#21295 = AXIS2_PLACEMENT_3D ( 'NONE', #18281, #25135, #20766 ) ;
#21296 = CARTESIAN_POINT ( 'NONE',  ( 19.84586683699999909, -35.72979163229999955, -9.028475981840001552 ) ) ;
#21297 = CARTESIAN_POINT ( 'NONE',  ( 0.000000000000000000, -15.80000000000000071, 0.000000000000000000 ) ) ;
#21298 = EDGE_LOOP ( 'NONE', ( #6232, #13243, #14396, #4087 ) ) ;
#21299 = CARTESIAN_POINT ( 'NONE',  ( -12.57997069900000042, -101.2141467319999890, -8.613800160570001196 ) ) ;
#21300 = PRODUCT_DEFINITION_SHAPE ( 'NONE', 'NONE',  #28810 ) ;
#21301 = CARTESIAN_POINT ( 'NONE',  ( -20.91226881666572623, -64.69849613357062879, 14.77252284388811709 ) ) ;
#21302 = CARTESIAN_POINT ( 'NONE',  ( -3.134349037060000231, -94.63960343439998724, 23.52861282910000185 ) ) ;
#21303 = CARTESIAN_POINT ( 'NONE',  ( 8.472395100179999972, -37.95144078439999902, -21.79230218340000036 ) ) ;
#21304 = DIRECTION ( 'NONE',  ( 1.000000000000000000, 0.000000000000000000, 0.000000000000000000 ) ) ;
#21305 = ORIENTED_EDGE ( 'NONE', *, *, #17702, .T. ) ;
#21306 = AXIS2_PLACEMENT_3D ( 'NONE', #17594, #26483, #15379 ) ;
#21307 = CARTESIAN_POINT ( 'NONE',  ( 13.27284362584146216, -100.9609609850291747, -9.861926373179022320 ) ) ;
#21308 = LINE ( 'NONE', #18984, #11186 ) ;
#21309 = CARTESIAN_POINT ( 'NONE',  ( 12.03933649750000079, -99.75094652210000845, -13.19595464940000085 ) ) ;
#21310 = ORIENTED_EDGE ( 'NONE', *, *, #21102, .F. ) ;
#21311 = CARTESIAN_POINT ( 'NONE',  ( 19.82299317300000041, -19.17198320609999840, -8.810535036470000136 ) ) ;
#21312 = PLANE ( 'NONE',  #12086 ) ;
#21313 = CARTESIAN_POINT ( 'NONE',  ( -14.78710411640000011, -74.45413981500000489, 36.35833236359999887 ) ) ;
#21314 = CARTESIAN_POINT ( 'NONE',  ( -1.610129840139999935, -19.46163090469999801, -22.22448219650000212 ) ) ;
#21315 = FACE_OUTER_BOUND ( 'NONE', #24202, .T. ) ;
#21316 = ORIENTED_EDGE ( 'NONE', *, *, #4317, .T. ) ;
#21317 = CARTESIAN_POINT ( 'NONE',  ( -1.136716282782229914, -74.21413368979379754, 47.16040998064198675 ) ) ;
#21318 = CARTESIAN_POINT ( 'NONE',  ( -0.1050716136000000023, -101.4254868729999970, -15.96877589609999681 ) ) ;
#21319 = CARTESIAN_POINT ( 'NONE',  ( 9.753828195949997948, -63.05466297450000468, -24.08172833849999961 ) ) ;
#21320 = CARTESIAN_POINT ( 'NONE',  ( 15.25351091960000005, -101.0848057460000007, 2.208595176079999778 ) ) ;
#21321 = CARTESIAN_POINT ( 'NONE',  ( -10.20110288159999890, -74.00000000000000000, 41.00000000000000000 ) ) ;
#21322 = CYLINDRICAL_SURFACE ( 'NONE', #15484, 1.000000000000000888 ) ;
#21323 = ORIENTED_EDGE ( 'NONE', *, *, #17105, .T. ) ;
#21324 = ADVANCED_FACE ( 'NONE', ( #27746 ), #23093, .T. ) ;
#21325 = CARTESIAN_POINT ( 'NONE',  ( 6.723571926760000039, -99.77922884479998800, 15.77121833869999890 ) ) ;
#21326 = CARTESIAN_POINT ( 'NONE',  ( 15.37735894870000131, -101.1716782170000073, 3.330286249999999892 ) ) ;
#21327 = EDGE_CURVE ( 'NONE', #5681, #16038, #13553, .T. ) ;
#21328 = CIRCLE ( 'NONE', #25064, 57.75000000000000000 ) ;
#21329 = CARTESIAN_POINT ( 'NONE',  ( -11.53977386519999904, -95.01967132979999064, -21.39764275870000176 ) ) ;
#21330 = CARTESIAN_POINT ( 'NONE',  ( 20.82960294989999994, -24.50935766780000336, -7.708047809820000040 ) ) ;
#21331 = CARTESIAN_POINT ( 'NONE',  ( 5.625522035772098306, -92.55017404143156057, -29.97671659717093817 ) ) ;
#21332 = AXIS2_PLACEMENT_3D ( 'NONE', #14958, #18551, #2974 ) ;
#21333 =( REPRESENTATION_RELATIONSHIP ('NONE','NONE', #26008, #5912 ) REPRESENTATION_RELATIONSHIP_WITH_TRANSFORMATION ( #11632 )SHAPE_REPRESENTATION_RELATIONSHIP( ) );
#21334 = CARTESIAN_POINT ( 'NONE',  ( -8.107793959220000346, -99.57787118740000665, 15.34802496579999875 ) ) ;
#21335 = DIRECTION ( 'NONE',  ( 0.6033158263509921237, 0.000000000000000000, -0.7975023596669915671 ) ) ;
#21336 = CARTESIAN_POINT ( 'NONE',  ( 0.2284307630869999717, -92.50000942380000879, -29.91770856260000144 ) ) ;
#21337 = DIRECTION ( 'NONE',  ( 1.000000000000000000, 0.000000000000000000, 0.000000000000000000 ) ) ;
#21338 = ORIENTED_EDGE ( 'NONE', *, *, #6311, .T. ) ;
#21339 = CARTESIAN_POINT ( 'NONE',  ( -5.750261582500000301, -100.9405348700000076, 14.87178911969999895 ) ) ;
#21340 = ORIENTED_EDGE ( 'NONE', *, *, #297, .T. ) ;
#21341 = CARTESIAN_POINT ( 'NONE',  ( -13.18623751009999978, -69.39685719070000403, -23.69831535020000146 ) ) ;
#21342 = ORIENTED_EDGE ( 'NONE', *, *, #5181, .T. ) ;
#21343 = CARTESIAN_POINT ( 'NONE',  ( 0.5497266010686944204, -101.0147714271427617, -16.48405362120961470 ) ) ;
#21344 = DIRECTION ( 'NONE',  ( -0.000000000000000000, 1.000000000000000000, 0.000000000000000000 ) ) ;
#21345 = DIRECTION ( 'NONE',  ( 0.4151946956541399669, 0.5000000000001689759, 0.7600087925152558821 ) ) ;
#21346 = CARTESIAN_POINT ( 'NONE',  ( 26.47162268830000187, -74.36200393670000608, -29.03680661989999834 ) ) ;
#21347 = TOROIDAL_SURFACE ( 'NONE', #12478, 19.50000000000000000, 7.000000000000000000 ) ;
#21348 = CARTESIAN_POINT ( 'NONE',  ( -22.44117711659999870, -70.82666672430001142, 16.89270182850000168 ) ) ;
#21349 = VECTOR ( 'NONE', #15316, 1000.000000000000000 ) ;
#21350 = DIRECTION ( 'NONE',  ( -0.9704142011833033488, 0.000000000000000000, 0.2414462220490755373 ) ) ;
#21351 = CARTESIAN_POINT ( 'NONE',  ( -18.59271594794251570, -19.47322495657686403, 13.20546376242789499 ) ) ;
#21352 = DIRECTION ( 'NONE',  ( 0.000000000000000000, -1.000000000000000000, 0.000000000000000000 ) ) ;
#21353 = CARTESIAN_POINT ( 'NONE',  ( 24.31603054292643051, -94.01603309709156520, -9.370392387943658363 ) ) ;
#21354 = CARTESIAN_POINT ( 'NONE',  ( -13.15041533549999997, -18.50000000000000000, 18.48778311079999881 ) ) ;
#21355 = ORIENTED_EDGE ( 'NONE', *, *, #7780, .F. ) ;
#21356 = ADVANCED_FACE ( 'NONE', ( #18717 ), #3785, .F. ) ;
#21357 = EDGE_LOOP ( 'NONE', ( #8872, #8983, #19878, #18030 ) ) ;
#21358 = EDGE_CURVE ( 'NONE', #9863, #4043, #20066, .T. ) ;
#21359 = EDGE_CURVE ( 'NONE', #9504, #11556, #12275, .T. ) ;
#21360 = CARTESIAN_POINT ( 'NONE',  ( -2.483024534920000193, -60.10032509980000270, -24.81723791200000306 ) ) ;
#21361 = AXIS2_PLACEMENT_3D ( 'NONE', #22326, #2373, #11228 ) ;
#21362 = CARTESIAN_POINT ( 'NONE',  ( 4.794255386040000566, -90.50000000000000000, 8.775825618900000791 ) ) ;
#21363 = CARTESIAN_POINT ( 'NONE',  ( 0.000000000000000000, 0.000000000000000000, 0.000000000000000000 ) ) ;
#21364 = CONICAL_SURFACE ( 'NONE', #9250, 8.099999999999997868, 0.7853981633970000820 ) ;
#21365 = VECTOR ( 'NONE', #3707, 1000.000000000000114 ) ;
#21366 = VERTEX_POINT ( 'NONE', #10077 ) ;
#21367 = CYLINDRICAL_SURFACE ( 'NONE', #6513, 0.5000000000000012212 ) ;
#21368 = ORIENTED_EDGE ( 'NONE', *, *, #18003, .F. ) ;
#21369 = CARTESIAN_POINT ( 'NONE',  ( 7.563321429468666146, -37.15172930439049281, -21.49750332032474986 ) ) ;
#21370 = CARTESIAN_POINT ( 'NONE',  ( 9.127337073059999639, -35.86526714520000070, -19.87708224909999899 ) ) ;
#21371 = ORIENTED_EDGE ( 'NONE', *, *, #13509, .T. ) ;
#21372 = CARTESIAN_POINT ( 'NONE',  ( -14.78710393409999924, -79.76388319610001076, 36.35833235529999996 ) ) ;
#21373 = CARTESIAN_POINT ( 'NONE',  ( -6.285925807789999986, -111.0000000000000000, 14.71350185169999847 ) ) ;
#21374 = CARTESIAN_POINT ( 'NONE',  ( -22.22671645450000000, -94.70873790529999781, -8.207211804499998209 ) ) ;
#21375 = CARTESIAN_POINT ( 'NONE',  ( -15.58411797090000128, -101.6484611620000038, 3.625951500279999795 ) ) ;
#21376 = DIRECTION ( 'NONE',  ( 0.7071067811865475727, 0.000000000000000000, 0.7071067811865475727 ) ) ;
#21377 = VERTEX_POINT ( 'NONE', #27872 ) ;
#21378 = TOROIDAL_SURFACE ( 'NONE', #15773, 33.64999999999999858, 1.250000000000000000 ) ;
#21379 = CARTESIAN_POINT ( 'NONE',  ( 20.30130924245990087, -98.17436949284241621, -1.306264829020119755 ) ) ;
#21380 = CARTESIAN_POINT ( 'NONE',  ( 7.670973119660000172, -34.59820496239999699, -21.21808926809999818 ) ) ;
#21381 = CARTESIAN_POINT ( 'NONE',  ( -1.470084592559999903, -18.85499412049999890, -21.97723017330000417 ) ) ;
#21382 = CARTESIAN_POINT ( 'NONE',  ( -7.894758065967145022, -100.4211561361303922, 15.01530531104792310 ) ) ;
#21383 = ORIENTED_EDGE ( 'NONE', *, *, #16847, .F. ) ;
#21384 = CIRCLE ( 'NONE', #2316, 29.91857981989999971 ) ;
#21385 = CIRCLE ( 'NONE', #7921, 4.999999999999997335 ) ;
#21386 = EDGE_CURVE ( 'NONE', #25224, #21714, #28442, .T. ) ;
#21387 = EDGE_CURVE ( 'NONE', #1710, #22634, #7850, .T. ) ;
#21388 = DIRECTION ( 'NONE',  ( 0.07620182022913774000, 0.000000000000000000, 0.9970924142694930215 ) ) ;
#21389 = CARTESIAN_POINT ( 'NONE',  ( -41.85974496015488455, -65.74398723832253211, -1.129426529332626883 ) ) ;
#21390 = CARTESIAN_POINT ( 'NONE',  ( 36.47289904670000027, -79.20535029740000255, -14.78463635570000001 ) ) ;
#21391 = ORIENTED_EDGE ( 'NONE', *, *, #23341, .F. ) ;
#21392 = EDGE_CURVE ( 'NONE', #22268, #21973, #5640, .T. ) ;
#21393 = PRODUCT_DEFINITION_CONTEXT ( 'detailed design', #14444, 'design' ) ;
#21394 = CARTESIAN_POINT ( 'NONE',  ( 6.693983694146544039, -100.7538407678108854, 15.29886744127561471 ) ) ;
#21395 = CARTESIAN_POINT ( 'NONE',  ( -2.629725044940439016, -80.38171235789693014, 46.75630123315725939 ) ) ;
#21396 = ORIENTED_EDGE ( 'NONE', *, *, #14417, .T. ) ;
#21397 = CARTESIAN_POINT ( 'NONE',  ( 47.16974817210000026, -74.50000513039999817, -1.075739376850000095 ) ) ;
#21398 = VERTEX_POINT ( 'NONE', #12965 ) ;
#21399 = CARTESIAN_POINT ( 'NONE',  ( 29.51280632209999766, -92.84292833370000153, 7.159272379339999937 ) ) ;
#21400 = CARTESIAN_POINT ( 'NONE',  ( -38.41801806958173415, -63.05619511567419977, 2.885163282592999145 ) ) ;
#21401 = DIRECTION ( 'NONE',  ( 0.000000000000000000, -1.000000000000000000, 0.000000000000000000 ) ) ;
#21402 = ORIENTED_EDGE ( 'NONE', *, *, #12576, .F. ) ;
#21403 = CARTESIAN_POINT ( 'NONE',  ( 11.77298154309999845, -101.2530993010000060, -9.604785791470000333 ) ) ;
#21404 = CARTESIAN_POINT ( 'NONE',  ( 2.486899575159999765E-14, -80.00000000000000000, 7.105427357599999217E-15 ) ) ;
#21405 = VECTOR ( 'NONE', #21857, 1000.000000000000000 ) ;
#21406 = AXIS2_PLACEMENT_3D ( 'NONE', #1843, #8105, #8524 ) ;
#21407 = ORIENTED_EDGE ( 'NONE', *, *, #17193, .F. ) ;
#21408 = DIRECTION ( 'NONE',  ( 0.6710140631236515274, 0.000000000000000000, -0.7414446217286144725 ) ) ;
#21409 = DIRECTION ( 'NONE',  ( 0.000000000000000000, -1.000000000000000000, 0.000000000000000000 ) ) ;
#21410 = CARTESIAN_POINT ( 'NONE',  ( -2.239413966154953695, -79.87344868178468005, 47.08826786916112184 ) ) ;
#21411 = EDGE_LOOP ( 'NONE', ( #23173, #23694, #22195, #25207 ) ) ;
#21412 = CARTESIAN_POINT ( 'NONE',  ( 0.000000000000000000, -82.25000000000000000, -40.00000000000000000 ) ) ;
#21413 = CARTESIAN_POINT ( 'NONE',  ( 18.35308676840000075, -98.83667233820000320, 3.322316128729999818 ) ) ;
#21414 = CARTESIAN_POINT ( 'NONE',  ( -20.34964369559999753, -94.63959812639998859, 12.21932103440000006 ) ) ;
#21415 = CARTESIAN_POINT ( 'NONE',  ( 23.64032483880000157, -93.61368346399999041, -9.011411803559999711 ) ) ;
#21416 = CARTESIAN_POINT ( 'NONE',  ( -1.156463699030000125, -55.05312981980000586, -23.31578321539999976 ) ) ;
#21417 = DIRECTION ( 'NONE',  ( 1.000000000000000000, 0.000000000000000000, 0.000000000000000000 ) ) ;
#21418 = CARTESIAN_POINT ( 'NONE',  ( -2.573828320119999624, -39.33785708389999769, -24.78875986600000303 ) ) ;
#21419 = EDGE_LOOP ( 'NONE', ( #16429, #16573, #5670, #28685 ) ) ;
#21421 = EDGE_CURVE ( 'NONE', #9768, #26053, #26943, .T. ) ;
#21420 = DIRECTION ( 'NONE',  ( 0.3390050494208429743, -0.7071067811866730279, 0.6205445805637129775 ) ) ;
#21422 = DIRECTION ( 'NONE',  ( 0.000000000000000000, 1.000000000000000000, 0.000000000000000000 ) ) ;
#21423 = CARTESIAN_POINT ( 'NONE',  ( 20.52188441893875392, -97.43430234772971232, 1.382123642611622572 ) ) ;
#21424 = CARTESIAN_POINT ( 'NONE',  ( 28.99618183149999950, -74.19519567169999164, -26.51509840489999803 ) ) ;
#21425 = CARTESIAN_POINT ( 'NONE',  ( 8.472395020760000506, -37.95144078679999922, -21.79230213740000011 ) ) ;
#21426 = VECTOR ( 'NONE', #24561, 1000.000000000000000 ) ;
#21427 = AXIS2_PLACEMENT_3D ( 'NONE', #14458, #23352, #28004 ) ;
#21428 = AXIS2_PLACEMENT_3D ( 'NONE', #17686, #8633, #17831 ) ;
#21429 =( NAMED_UNIT ( * ) SI_UNIT ( $, .STERADIAN. ) SOLID_ANGLE_UNIT ( ) );
#21430 = ORIENTED_EDGE ( 'NONE', *, *, #28731, .T. ) ;
#21431 = DIRECTION ( 'NONE',  ( 0.4794255386042040046, 0.000000000000000000, 0.8775825618903722036 ) ) ;
#21432 = CARTESIAN_POINT ( 'NONE',  ( 20.14104788939999935, -35.73233869100000248, -9.018304108959998899 ) ) ;
#21433 = ORIENTED_EDGE ( 'NONE', *, *, #16252, .F. ) ;
#21434 = CARTESIAN_POINT ( 'NONE',  ( 19.54973049059999823, -35.76277645470000266, -9.056828148970000214 ) ) ;
#21435 = CARTESIAN_POINT ( 'NONE',  ( -22.14844716308801864, -79.50000004209999815, -32.75504888958925420 ) ) ;
#21436 = VERTEX_POINT ( 'NONE', #28155 ) ;
#21437 = CARTESIAN_POINT ( 'NONE',  ( -12.79312068399999980, -101.1716782080000030, -9.159770265490001506 ) ) ;
#21438 = EDGE_CURVE ( 'NONE', #18300, #12333, #17744, .T. ) ;
#21439 = ORIENTED_EDGE ( 'NONE', *, *, #13655, .F. ) ;
#21440 = DIRECTION ( 'NONE',  ( -0.8775825618903722036, 0.000000000000000000, 0.4794255386042041156 ) ) ;
#21441 = CARTESIAN_POINT ( 'NONE',  ( 8.998660423299998712, -44.89607406070000195, -22.33592606139999859 ) ) ;
#21442 = CIRCLE ( 'NONE', #9333, 18.64285714289999873 ) ;
#21443 = CARTESIAN_POINT ( 'NONE',  ( -39.83915519491969803, -65.73344136608082522, 2.187954346637793979 ) ) ;
#21444 = ORIENTED_EDGE ( 'NONE', *, *, #419, .F. ) ;
#21446 = EDGE_CURVE ( 'NONE', #18925, #13695, #26124, .T. ) ;
#21445 = AXIS2_PLACEMENT_3D ( 'NONE', #5219, #16273, #4923 ) ;
#21447 = CARTESIAN_POINT ( 'NONE',  ( 25.77179612209999959, -37.57799544290000426, 47.17495636800000369 ) ) ;
#21448 = VECTOR ( 'NONE', #22613, 1000.000000000000000 ) ;
#21449 = CARTESIAN_POINT ( 'NONE',  ( -22.22671645450000000, -94.70873790529999781, -8.207211804499998209 ) ) ;
#21450 = CARTESIAN_POINT ( 'NONE',  ( 26.43538883849999976, -72.55114739969998539, 11.02537517960000102 ) ) ;
#21451 = DIRECTION ( 'NONE',  ( 0.000000000000000000, 1.000000000000000000, 0.000000000000000000 ) ) ;
#21452 = ORIENTED_EDGE ( 'NONE', *, *, #5324, .T. ) ;
#21453 = CARTESIAN_POINT ( 'NONE',  ( 19.29218169219999979, -18.50000000000000000, -7.924293390789999947 ) ) ;
#21454 = ADVANCED_FACE ( 'NONE', ( #4246 ), #7970, .F. ) ;
#21455 = CARTESIAN_POINT ( 'NONE',  ( -14.77250568370000039, -74.40829841730000282, 36.35986053050000066 ) ) ;
#21456 = CARTESIAN_POINT ( 'NONE',  ( -2.535581654609999624, -19.42987840509999842, -23.25781427689999958 ) ) ;
#21457 = CARTESIAN_POINT ( 'NONE',  ( -27.68682485439999752, -13.40000000000000036, -50.68039294919999804 ) ) ;
#21458 = VERTEX_POINT ( 'NONE', #6583 ) ;
#21459 = DIRECTION ( 'NONE',  ( 0.4794255386042041156, 0.000000000000000000, 0.8775825618903722036 ) ) ;
#21460 = CARTESIAN_POINT ( 'NONE',  ( 0.08412725538310000806, -101.1700440390000040, -15.30178034989999958 ) ) ;
#21461 = CARTESIAN_POINT ( 'NONE',  ( 7.442798598269999566, -60.60073824219999494, -22.42221163419999996 ) ) ;
#21462 = CARTESIAN_POINT ( 'NONE',  ( 15.50925565250000027, -100.9197086960000007, 1.894555174519999996 ) ) ;
#21463 = CARTESIAN_POINT ( 'NONE',  ( 22.87891866909999905, -57.82174915179999886, 10.24673290389999991 ) ) ;
#21464 = CARTESIAN_POINT ( 'NONE',  ( -36.79999999999999716, -65.14977478849999670, 0.1732050807570000017 ) ) ;
#21465 = VERTEX_POINT ( 'NONE', #6425 ) ;
#21466 = CARTESIAN_POINT ( 'NONE',  ( 6.252384452659999425, -100.1340845430000002, 15.41982103239999979 ) ) ;
#21467 = CARTESIAN_POINT ( 'NONE',  ( 15.58391247289999981, -101.4121386959999995, 3.523358517780000199 ) ) ;
#21468 = CIRCLE ( 'NONE', #556, 7.750000000000000000 ) ;
#21469 = AXIS2_PLACEMENT_3D ( 'NONE', #13334, #4905, #2290 ) ;
#21470 = CARTESIAN_POINT ( 'NONE',  ( 23.00372540730000281, -92.50000000000000000, -20.02694728079999820 ) ) ;
#21471 = CARTESIAN_POINT ( 'NONE',  ( 5.046652419183167204, -92.65976904077027143, -30.07958860648908583 ) ) ;
#21472 = DIRECTION ( 'NONE',  ( 1.000000000000000000, 0.000000000000000000, 0.000000000000000000 ) ) ;
#21473 = CARTESIAN_POINT ( 'NONE',  ( 1.955333439440000154, -92.99999932709999939, -29.74887251719999881 ) ) ;
#21474 = B_SPLINE_SURFACE_WITH_KNOTS ( 'NONE', 5, 5, ( 
 ( #12520, #21432, #28402, #3389, #26085, #1490 ),
 ( #21710, #19382, #14988, #25674, #19110, #12383 ),
 ( #19243, #5569, #3525, #17196, #12660, #10329 ),
 ( #3936, #1759, #25944, #8166, #28259, #17053 ),
 ( #19517, #14451, #27995, #12253, #25815, #1218 ),
 ( #21571, #10059, #21294, #1346, #10194, #16921 ) ),
 .UNSPECIFIED., .F., .F., .F.,
 ( 6, 6 ),
 ( 6, 6 ),
 ( 1.601061932509999952, 3.163829236780000276 ),
 ( 0.000000000000000000, 2.000000000000000000 ),
 .UNSPECIFIED. ) ;
#21475 = CARTESIAN_POINT ( 'NONE',  ( 0.000000000000000000, -16.10310889129999623, 0.000000000000000000 ) ) ;
#21476 = DIRECTION ( 'NONE',  ( 0.000000000000000000, 1.000000000000000000, 0.000000000000000000 ) ) ;
#21477 = VERTEX_POINT ( 'NONE', #21457 ) ;
#21478 = CARTESIAN_POINT ( 'NONE',  ( -40.00000000000000000, -63.00000000000000000, 0.000000000000000000 ) ) ;
#21479 = DIRECTION ( 'NONE',  ( 0.000000000000000000, 1.000000000000000000, 0.000000000000000000 ) ) ;
#21480 = EDGE_LOOP ( 'NONE', ( #4629, #16256, #18909, #13216 ) ) ;
#21481 = EDGE_CURVE ( 'NONE', #17168, #10513, #23348, .T. ) ;
#21482 = EDGE_CURVE ( 'NONE', #14724, #2204, #21468, .T. ) ;
#21483 = CARTESIAN_POINT ( 'NONE',  ( -0.8955242351559999925, -101.2530993039999885, -15.16897421750000063 ) ) ;
#21484 = CARTESIAN_POINT ( 'NONE',  ( -6.831813925109999630, -13.50000000000000000, -12.50555150689999984 ) ) ;
#21485 = CIRCLE ( 'NONE', #6114, 0.5000000000000004441 ) ;
#21486 = CARTESIAN_POINT ( 'NONE',  ( 13.53859855288502878, -92.62938374250892082, 27.33052066698929750 ) ) ;
#21487 = EDGE_CURVE ( 'NONE', #10298, #24581, #19266, .T. ) ;
#21488 = AXIS2_PLACEMENT_3D ( 'NONE', #22916, #25247, #8019 ) ;
#21489 = CARTESIAN_POINT ( 'NONE',  ( 26.60005552420000186, -73.86497505609999337, -28.90969314500000209 ) ) ;
#21490 = EDGE_CURVE ( 'NONE', #10529, #26232, #8879, .T. ) ;
#21491 = CARTESIAN_POINT ( 'NONE',  ( 16.13266937400000245, -84.75000000000000000, 29.53065320760000034 ) ) ;
#21492 = CARTESIAN_POINT ( 'NONE',  ( -12.84485488516277840, -101.3051320416489176, -9.329032816835999498 ) ) ;
#21493 = DIRECTION ( 'NONE',  ( 0.000000000000000000, 1.000000000000000000, 0.000000000000000000 ) ) ;
#21494 = CARTESIAN_POINT ( 'NONE',  ( -11.81899278030000033, -64.69849622489999774, -22.71259345900000071 ) ) ;
#21495 = CARTESIAN_POINT ( 'NONE',  ( 7.316573060279999652, -35.82074236369999909, -21.43354451849999975 ) ) ;
#21496 = CARTESIAN_POINT ( 'NONE',  ( -41.00000000000000000, -74.00000000000000000, 10.20110288159999890 ) ) ;
#21497 = ORIENTED_EDGE ( 'NONE', *, *, #22344, .F. ) ;
#21498 = CARTESIAN_POINT ( 'NONE',  ( -40.81117883860000006, -65.49083508809999898, 2.489060262989999828 ) ) ;
#21499 = EDGE_LOOP ( 'NONE', ( #281, #24008 ) ) ;
#21500 = CARTESIAN_POINT ( 'NONE',  ( 22.72991323779999817, -37.99098077740000434, -9.322992626879999634 ) ) ;
#21501 = AXIS2_PLACEMENT_3D ( 'NONE', #19458, #8527, #23980 ) ;
#21502 = CARTESIAN_POINT ( 'NONE',  ( -1.512642400649999885, -63.93339545899999621, -24.75805884960000114 ) ) ;
#21503 = CARTESIAN_POINT ( 'NONE',  ( -0.1868532263790000092, -101.1889999979999999, -16.79896085689999907 ) ) ;
#21504 = TOROIDAL_SURFACE ( 'NONE', #15927, 2.500000000000000000, 0.5000000000000000000 ) ;
#21505 = CARTESIAN_POINT ( 'NONE',  ( -0.6998919996272167099, -101.1416252791453161, -15.52603992147200174 ) ) ;
#21506 = ORIENTED_EDGE ( 'NONE', *, *, #663, .T. ) ;
#21507 = CARTESIAN_POINT ( 'NONE',  ( 21.18059972589999873, -34.84004059659999797, -7.857545738520000711 ) ) ;
#21508 = EDGE_CURVE ( 'NONE', #23613, #21377, #20542, .T. ) ;
#21509 = LINE ( 'NONE', #19329, #24139 ) ;
#21510 = EDGE_LOOP ( 'NONE', ( #16311, #15925, #27501, #15173 ) ) ;
#21511 = DIRECTION ( 'NONE',  ( 0.000000000000000000, 1.000000000000000000, 0.000000000000000000 ) ) ;
#21512 = EDGE_CURVE ( 'NONE', #19954, #28714, #23780, .T. ) ;
#21513 = PLANE ( 'NONE',  #5789 ) ;
#21514 = DIRECTION ( 'NONE',  ( 0.000000000000000000, 1.000000000000000000, 0.000000000000000000 ) ) ;
#21515 = EDGE_CURVE ( 'NONE', #13115, #5438, #25657, .T. ) ;
#21516 = CARTESIAN_POINT ( 'NONE',  ( 21.88147998950000073, -19.49009541680000268, 9.576298402129999943 ) ) ;
#21517 = PLANE ( 'NONE',  #6712 ) ;
#21518 = CARTESIAN_POINT ( 'NONE',  ( -39.50000000000000000, -63.30468293320000583, 2.309401076760000393 ) ) ;
#21519 = ORIENTED_EDGE ( 'NONE', *, *, #24844, .T. ) ;
#21520 = VECTOR ( 'NONE', #7441, 1000.000000000000000 ) ;
#21521 = CIRCLE ( 'NONE', #5255, 0.3500000000000003664 ) ;
#21522 = CARTESIAN_POINT ( 'NONE',  ( 21.80109759570151340, -96.92941680763301804, -3.102706385432779879 ) ) ;
#21523 = CARTESIAN_POINT ( 'NONE',  ( -12.40996983109999974, -101.1412505549999992, -10.36257240380000155 ) ) ;
#21524 = AXIS2_PLACEMENT_3D ( 'NONE', #16783, #16927, #1635 ) ;
#21525 = CARTESIAN_POINT ( 'NONE',  ( 19.53781279187136022, -93.86980009075321618, 16.40476867545000417 ) ) ;
#21526 = CARTESIAN_POINT ( 'NONE',  ( -7.880236046065482114, -100.4872618029792619, 14.96335263205392963 ) ) ;
#21528 = VERTEX_POINT ( 'NONE', #15741 ) ;
#21527 = B_SPLINE_CURVE_WITH_KNOTS ( 'NONE', 3,
 ( #12045, #20960, #23001, #11757, #1017, #27521, #25335, #3052, #11905, #874 ),
 .UNSPECIFIED., .F., .F.,
 ( 4, 2, 2, 2, 4 ),
 ( 0.000000000000000000, 0.2500000000000000000, 0.5000000000000000000, 0.7500000000000000000, 1.000000000000000000 ),
 .UNSPECIFIED. ) ;
#21529 = CARTESIAN_POINT ( 'NONE',  ( 11.21511754571216990, -69.74181458266943423, -26.64805835954446067 ) ) ;
#21530 = DIRECTION ( 'NONE',  ( 0.5193452265677850344, 0.000000000000000000, 0.8545645298286467240 ) ) ;
#21531 = CARTESIAN_POINT ( 'NONE',  ( 36.60240428190000017, -80.39630767040000592, -14.17343997929999944 ) ) ;
#21532 = VERTEX_POINT ( 'NONE', #24654 ) ;
#21533 = VECTOR ( 'NONE', #703, 1000.000000000000000 ) ;
#21534 = FACE_OUTER_BOUND ( 'NONE', #19240, .T. ) ;
#21535 = CARTESIAN_POINT ( 'NONE',  ( 6.660738224123119444, -101.1451610293114243, 14.97649247838033304 ) ) ;
#21536 = CARTESIAN_POINT ( 'NONE',  ( 11.89948051634188531, -101.2404586421460380, -10.39979277174668759 ) ) ;
#21537 = ORIENTED_EDGE ( 'NONE', *, *, #10717, .F. ) ;
#21538 = CARTESIAN_POINT ( 'NONE',  ( 47.17354815139999857, -74.60193236360001379, -1.119565185129999918 ) ) ;
#21539 = ORIENTED_EDGE ( 'NONE', *, *, #24715, .T. ) ;
#21540 = CARTESIAN_POINT ( 'NONE',  ( 22.51417952139999912, -55.00753887609999992, 10.12166766410000029 ) ) ;
#21541 = CARTESIAN_POINT ( 'NONE',  ( 21.75659477429999811, -111.0000000000000000, -13.30039788230000042 ) ) ;
#21542 = ORIENTED_EDGE ( 'NONE', *, *, #3790, .T. ) ;
#21543 = AXIS2_PLACEMENT_3D ( 'NONE', #25339, #14393, #3055 ) ;
#21544 = CARTESIAN_POINT ( 'NONE',  ( 11.97048044210000128, -101.2358105800000061, -9.395351924210000760 ) ) ;
#21545 = EDGE_CURVE ( 'NONE', #4293, #17438, #13053, .T. ) ;
#21546 = B_SPLINE_CURVE_WITH_KNOTS ( 'NONE', 3,
 ( #13193, #8670, #21955, #20054, #21801, #2144 ),
 .UNSPECIFIED., .F., .F.,
 ( 4, 2, 4 ),
 ( 0.000000000000000000, 0.5000000000000000000, 1.000000000000000000 ),
 .UNSPECIFIED. ) ;
#21547 = VERTEX_POINT ( 'NONE', #194 ) ;
#21548 = CARTESIAN_POINT ( 'NONE',  ( -21.91703890630000018, -80.37806415250000214, -32.56305777900000464 ) ) ;
#21549 = CARTESIAN_POINT ( 'NONE',  ( 20.14180970569999829, -45.99935878759999497, 11.02192488110000035 ) ) ;
#21550 = CARTESIAN_POINT ( 'NONE',  ( 0.000000000000000000, -15.49689110870000164, 0.000000000000000000 ) ) ;
#21551 = ORIENTED_EDGE ( 'NONE', *, *, #6811, .T. ) ;
#21552 = EDGE_CURVE ( 'NONE', #16196, #3267, #14931, .T. ) ;
#21553 = CARTESIAN_POINT ( 'NONE',  ( -18.76759046260000119, -96.83679385039999943, -9.979844675380000751 ) ) ;
#21554 = CARTESIAN_POINT ( 'NONE',  ( 13.53079842320000026, -100.4071172650000108, -9.942387125549998927 ) ) ;
#21555 = DIRECTION ( 'NONE',  ( 0.000000000000000000, 1.000000000000000000, 0.000000000000000000 ) ) ;
#21556 = CARTESIAN_POINT ( 'NONE',  ( 23.53303068880000026, -92.50000942380000879, -18.47479182160000022 ) ) ;
#21557 = CARTESIAN_POINT ( 'NONE',  ( -1.452960264739999952, -55.04870336940000186, -23.42848252749999816 ) ) ;
#21558 = AXIS2_PLACEMENT_3D ( 'NONE', #13597, #3133, #5004 ) ;
#21559 = CARTESIAN_POINT ( 'NONE',  ( 10.61988563626112558, -72.59634600277628635, -26.81031528543675435 ) ) ;
#21560 = LINE ( 'NONE', #23601, #3804 ) ;
#21561 = ORIENTED_EDGE ( 'NONE', *, *, #23587, .T. ) ;
#21562 = DIRECTION ( 'NONE',  ( 0.000000000000000000, 1.000000000000000000, 0.000000000000000000 ) ) ;
#21563 = CARTESIAN_POINT ( 'NONE',  ( 0.3059185938709999553, -92.50000000000000000, 14.72672055670000013 ) ) ;
#21564 = DIRECTION ( 'NONE',  ( 0.5762746169049438594, 0.000000000000000000, -0.8172561201429208166 ) ) ;
#21565 = CARTESIAN_POINT ( 'NONE',  ( -38.25000000000000000, -65.21397798589998729, 2.551096136590000008 ) ) ;
#21566 = CARTESIAN_POINT ( 'NONE',  ( -3.355978770230000130, -91.50000000000000000, -6.143077933229999843 ) ) ;
#21567 = AXIS2_PLACEMENT_3D ( 'NONE', #15147, #4530, #13411 ) ;
#21568 = EDGE_CURVE ( 'NONE', #6448, #23842, #11680, .T. ) ;
#21569 = ORIENTED_EDGE ( 'NONE', *, *, #1308, .F. ) ;
#21570 = AXIS2_PLACEMENT_3D ( 'NONE', #3862, #28191, #25355 ) ;
#21571 = CARTESIAN_POINT ( 'NONE',  ( 19.49544327699999968, -35.50000000000000000, -8.986258411389998813 ) ) ;
#21572 = ORIENTED_EDGE ( 'NONE', *, *, #26209, .F. ) ;
#21573 = AXIS2_PLACEMENT_3D ( 'NONE', #80, #9080, #20162 ) ;
#21574 = CARTESIAN_POINT ( 'NONE',  ( 21.57170138819999750, -37.33907283540000321, -8.016383387539999461 ) ) ;
#21575 = CARTESIAN_POINT ( 'NONE',  ( 9.038647564319999717, -35.72724395809999720, -19.55068592700000352 ) ) ;
#21576 = ORIENTED_EDGE ( 'NONE', *, *, #5324, .F. ) ;
#21577 = CARTESIAN_POINT ( 'NONE',  ( -12.47452166779999949, -101.1848541600000004, -8.829639320900001920 ) ) ;
#21578 = EDGE_CURVE ( 'NONE', #5350, #2148, #236, .T. ) ;
#21579 = DIRECTION ( 'NONE',  ( 0.000000000000000000, 1.000000000000000000, 0.000000000000000000 ) ) ;
#21580 = CARTESIAN_POINT ( 'NONE',  ( -7.925865731170000039, -99.78393592979999482, 15.40304860989999902 ) ) ;
#21581 = DIRECTION ( 'NONE',  ( 1.000000000000000000, 0.000000000000000000, 0.000000000000000000 ) ) ;
#21582 = CARTESIAN_POINT ( 'NONE',  ( 7.233371418730000002, -44.93343662230000035, -21.75421831149999718 ) ) ;
#21583 = AXIS2_PLACEMENT_3D ( 'NONE', #2952, #25245, #13562 ) ;
#21584 = DIRECTION ( 'NONE',  ( 0.4794255386042041156, 0.000000000000000000, 0.8775825618903722036 ) ) ;
#21585 = ORIENTED_EDGE ( 'NONE', *, *, #8902, .F. ) ;
#21586 = CARTESIAN_POINT ( 'NONE',  ( 13.55253169098114263, -100.5550990433908538, -10.02507008700657920 ) ) ;
#21587 = CARTESIAN_POINT ( 'NONE',  ( 23.90606501070000078, -57.45864775100000088, 0.8443138621939999533 ) ) ;
#21588 = CARTESIAN_POINT ( 'NONE',  ( 24.84525630199999924, -69.52108470319998901, 11.33455677210000090 ) ) ;
#21589 = CARTESIAN_POINT ( 'NONE',  ( 7.132709192110000096, -99.83167692499999646, 15.78738634319999967 ) ) ;
#21590 = ORIENTED_EDGE ( 'NONE', *, *, #5663, .F. ) ;
#21591 = CARTESIAN_POINT ( 'NONE',  ( -39.85912817270000374, -74.23958658479999428, 7.332335648789999993 ) ) ;
#21592 = CARTESIAN_POINT ( 'NONE',  ( -14.52836087100000029, -74.22231530550000400, 36.83217634790000261 ) ) ;
#21593 = CARTESIAN_POINT ( 'NONE',  ( -17.65264067069999854, -93.65249602680000862, 18.18801510169999958 ) ) ;
#21594 = CARTESIAN_POINT ( 'NONE',  ( -20.62076907760296507, -93.14879094580942365, 16.44113247062627181 ) ) ;
#21595 = EDGE_LOOP ( 'NONE', ( #2233, #6731, #3296, #17248 ) ) ;
#21596 = CONICAL_SURFACE ( 'NONE', #25345, 21.99999999999999645, 0.03490658503990158590 ) ;
#21597 = DIRECTION ( 'NONE',  ( 1.000000000000000000, 0.000000000000000000, 0.000000000000000000 ) ) ;
#21598 = AXIS2_PLACEMENT_3D ( 'NONE', #10610, #12670, #24044 ) ;
#21599 = B_SPLINE_CURVE_WITH_KNOTS ( 'NONE', 3,
 ( #2201, #26681, #13706, #2503, #11357, #20261, #3364, #14428, #27706, #9620, #1063, #23319, #7871 ),
 .UNSPECIFIED., .F., .F.,
 ( 4, 2, 1, 1, 1, 2, 2, 4 ),
 ( 0.000000000000000000, 0.2499999999999817923, 0.3749999999999705236, 0.4374999999999647504, 0.4687499999999620859, 0.4843749999999605316, 0.4999999999999589217, 1.000000000000000000 ),
 .UNSPECIFIED. ) ;
#21600 = CARTESIAN_POINT ( 'NONE',  ( -0.1779554536940000098, -101.6484611540000031, -15.99901033990000165 ) ) ;
#21601 = DIRECTION ( 'NONE',  ( 0.000000000000000000, 0.000000000000000000, -1.000000000000000000 ) ) ;
#21602 = CARTESIAN_POINT ( 'NONE',  ( 15.33316675979999921, -101.1045726949999874, 2.495933759240000160 ) ) ;
#21603 = CARTESIAN_POINT ( 'NONE',  ( 20.91274138339999666, -58.78702526330000211, 10.73875272749999965 ) ) ;
#21604 = CARTESIAN_POINT ( 'NONE',  ( -36.91568593819999933, -65.21397798589998729, 0.2399963883279999932 ) ) ;
#21605 = ORIENTED_EDGE ( 'NONE', *, *, #12276, .T. ) ;
#21606 = EDGE_CURVE ( 'NONE', #1588, #7139, #25214, .T. ) ;
#21607 = CARTESIAN_POINT ( 'NONE',  ( 6.895355905279999753, -99.94751438429999268, 15.70952527899999929 ) ) ;
#21608 = CARTESIAN_POINT ( 'NONE',  ( 15.13453645979999962, -101.1292389600000092, 3.376594308710000103 ) ) ;
#21609 = EDGE_CURVE ( 'NONE', #9115, #27225, #2405, .T. ) ;
#21610 = CARTESIAN_POINT ( 'NONE',  ( 7.595444726729600567E-15, -74.00000000000000000, 32.25000000000000000 ) ) ;
#21611 = AXIS2_PLACEMENT_3D ( 'NONE', #11703, #8063, #23646 ) ;
#21612 = CARTESIAN_POINT ( 'NONE',  ( -39.77168464789694724, -65.72207046437310396, -2.201769106273790744 ) ) ;
#21613 = CARTESIAN_POINT ( 'NONE',  ( 21.51248591490000095, -18.50000000000000000, 1.147234204320000117 ) ) ;
#21614 = VECTOR ( 'NONE', #21095, 1000.000000000000000 ) ;
#21615 = ADVANCED_FACE ( 'NONE', ( #13564 ), #26694, .T. ) ;
#21616 = CARTESIAN_POINT ( 'NONE',  ( -32.75000000000000000, -73.00000000000000000, 2.464695114669999848E-15 ) ) ;
#21617 = ORIENTED_EDGE ( 'NONE', *, *, #10924, .T. ) ;
#21618 = CARTESIAN_POINT ( 'NONE',  ( 4.474575075100000632, -92.65715406910000240, -27.57907939949999943 ) ) ;
#21619 = LINE ( 'NONE', #26418, #10219 ) ;
#21620 = CARTESIAN_POINT ( 'NONE',  ( -6.592280350930000310, -101.1848541609999899, 13.78765661559999955 ) ) ;
#21621 = VERTEX_POINT ( 'NONE', #20421 ) ;
#21622 = AXIS2_PLACEMENT_3D ( 'NONE', #22954, #22802, #18572 ) ;
#21623 =( NAMED_UNIT ( * ) PLANE_ANGLE_UNIT ( ) SI_UNIT ( $, .RADIAN. ) );
#21624 = CARTESIAN_POINT ( 'NONE',  ( -12.54500315030344382, -101.0147714269334074, -10.70743288971485363 ) ) ;
#21625 = ORIENTED_EDGE ( 'NONE', *, *, #26319, .F. ) ;
#21626 = DIRECTION ( 'NONE',  ( 0.4794255386042036715, 0.000000000000000000, 0.8775825618903723147 ) ) ;
#21627 = CARTESIAN_POINT ( 'NONE',  ( -38.67409491847346459, -73.94611239985914608, -7.370697001239630453 ) ) ;
#21628 = B_SPLINE_CURVE_WITH_KNOTS ( 'NONE', 5,
 ( #23051, #17939, #919, #22461, #18080, #7017 ),
 .UNSPECIFIED., .F., .F.,
 ( 6, 6 ),
 ( 0.000000000000000000, 1.000000000000000000 ),
 .UNSPECIFIED. ) ;
#21629 = CARTESIAN_POINT ( 'NONE',  ( 4.794255386040000566, -107.5000000000000000, 8.775825618900000791 ) ) ;
#21630 = DIRECTION ( 'NONE',  ( 0.4794255386042040046, 0.000000000000000000, 0.8775825618903722036 ) ) ;
#21631 = CARTESIAN_POINT ( 'NONE',  ( 16.19501884596224883, -94.70448199252453492, 17.23845109483602656 ) ) ;
#21632 = CARTESIAN_POINT ( 'NONE',  ( -22.52693219800000080, -70.43934371539999972, 17.54847698860000094 ) ) ;
#21633 = CIRCLE ( 'NONE', #8130, 2.500000000000002220 ) ;
#21634 = DIRECTION ( 'NONE',  ( -0.4794255386042028944, 0.000000000000000000, 0.8775825618903727587 ) ) ;
#21635 = CARTESIAN_POINT ( 'NONE',  ( -18.64599988254608220, -19.47504441210472592, 13.34621241184425244 ) ) ;
#21636 = CARTESIAN_POINT ( 'NONE',  ( 6.944365432299999696, -36.14100883020000055, -21.52374318029999856 ) ) ;
#21637 = DIRECTION ( 'NONE',  ( 0.000000000000000000, -1.000000000000000000, 0.000000000000000000 ) ) ;
#21638 = ORIENTED_EDGE ( 'NONE', *, *, #18095, .T. ) ;
#21639 = CARTESIAN_POINT ( 'NONE',  ( 22.02882315030000271, -19.46510050329999686, -0.4636558402470000173 ) ) ;
#21640 = AXIS2_PLACEMENT_3D ( 'NONE', #23095, #24977, #16220 ) ;
#21641 = ORIENTED_EDGE ( 'NONE', *, *, #22000, .F. ) ;
#21642 = ADVANCED_FACE ( 'NONE', ( #16042 ), #2362, .F. ) ;
#21643 = EDGE_CURVE ( 'NONE', #15494, #21689, #5212, .T. ) ;
#21644 = CARTESIAN_POINT ( 'NONE',  ( -2.486260167500000229, -58.65571127909999660, -24.68408288270000028 ) ) ;
#21645 = EDGE_CURVE ( 'NONE', #27146, #22782, #9899, .T. ) ;
#21646 = CARTESIAN_POINT ( 'NONE',  ( -29.08067107640000160, -92.50732182800000203, 4.792447498680000528 ) ) ;
#21647 = DIRECTION ( 'NONE',  ( 0.000000000000000000, -1.000000000000000000, 0.000000000000000000 ) ) ;
#21648 = EDGE_CURVE ( 'NONE', #1165, #5725, #17229, .T. ) ;
#21649 = CARTESIAN_POINT ( 'NONE',  ( -19.51583823490001279, -52.61368720150016998, 13.56962763330000676 ) ) ;
#21651 = CLOSED_SHELL ( 'NONE', ( #9812, #9036, #7730, #16433, #20443, #20983, #13241, #5216, #2085, #5346, #10744, #9007, #20316, #18378, #19317, #21832, #22757, #23085, #18401, #20810, #5930, #19849, #12034, #16149, #10428, #26188, #14118, #12480, #21231, #9828, #26241, #27571, #4010, #21176, #19647, #14359, #943, #22558, #7288, #14093, #23137, #28476, #28131, #13100, #24263, #27785, #19963, #21703, #14732, #12640, #11009, #28219, #24921, #28348, #8474, #22824, #467, #2992, #9706, #1840, #9617, #1134, #13746, #23815, #8963, #5481, #17290, #255, #16609, #2816, #19885, #19497, #14920, #11625, #368, #21142, #7792, #6754, #3027, #21099, #18274, #22447, #5351, #20171, #15305, #9859, #6013, #10242, #25774, #3253, #23749, #9347, #22992, #17631, #17890, #20945, #19532, #8097, #25767, #24009, #19399, #4817, #2240, #165, #2347, #16498, #10976, #17326, #20779, #15263, #21292, #1434, #6107, #25223, #16416, #8032, #5073, #28249, #13015, #27196, #20174, #14309, #17568, #6995, #22078, #125, #23942, #12381, #16999, #10000, #28409, #15100, #10623, #14542, #2457, #2154, #3878 ) ) ;
#21650 = CARTESIAN_POINT ( 'NONE',  ( 15.66940200309999831, -100.9678331089999972, 4.038298765579999561 ) ) ;
#21652 = VERTEX_POINT ( 'NONE', #7028 ) ;
#21653 = CARTESIAN_POINT ( 'NONE',  ( 21.47059222220000052, -36.19499449340000297, -7.248977034690000210 ) ) ;
#21654 = EDGE_LOOP ( 'NONE', ( #20492, #26568, #3903, #18510 ) ) ;
#21655 = CARTESIAN_POINT ( 'NONE',  ( 2.220446049249999745E-14, -11.00000000000000000, -31.00000000000000000 ) ) ;
#21656 = DIRECTION ( 'NONE',  ( 0.000000000000000000, -1.000000000000000000, 0.000000000000000000 ) ) ;
#21657 = B_SPLINE_CURVE_WITH_KNOTS ( 'NONE', 3,
 ( #28140, #12950, #8174, #17060, #28411, #4081 ),
 .UNSPECIFIED., .F., .F.,
 ( 4, 2, 4 ),
 ( 0.000000000000000000, 0.5000000000000000000, 1.000000000000000000 ),
 .UNSPECIFIED. ) ;
#21658 = CARTESIAN_POINT ( 'NONE',  ( 39.31221710949670012, -74.09469053480707146, 7.479534729103155755 ) ) ;
#21659 = CARTESIAN_POINT ( 'NONE',  ( -14.86016661329999877, -101.1848541609999899, 3.566077570999999669 ) ) ;
#21660 = CARTESIAN_POINT ( 'NONE',  ( -31.89935321680000158, -74.00000000000000000, -21.99985828019999801 ) ) ;
#21661 = CARTESIAN_POINT ( 'NONE',  ( -24.21840725559999896, -79.50000000000000000, -34.11790219230000076 ) ) ;
#21662 = ORIENTED_EDGE ( 'NONE', *, *, #12515, .T. ) ;
#21663 = DIRECTION ( 'NONE',  ( 0.000000000000000000, 1.000000000000000000, 0.000000000000000000 ) ) ;
#21664 = CARTESIAN_POINT ( 'NONE',  ( -12.50546161790000177, -100.7430069139999915, -10.75263243640000077 ) ) ;
#21665 = CARTESIAN_POINT ( 'NONE',  ( -7.571352933129060325, -101.1248211533539205, 14.55532840934864147 ) ) ;
#21666 = ORIENTED_EDGE ( 'NONE', *, *, #7093, .F. ) ;
#21667 = CARTESIAN_POINT ( 'NONE',  ( -1.007768741648868760, -101.5703832412493739, -16.02700633418644216 ) ) ;
#21668 = CARTESIAN_POINT ( 'NONE',  ( -32.33029131960000058, -74.08184093439999174, -21.92820895030000017 ) ) ;
#21669 = CARTESIAN_POINT ( 'NONE',  ( 36.61516926800000249, -79.38053706460000569, -14.70489075899999953 ) ) ;
#21670 = ORIENTED_EDGE ( 'NONE', *, *, #16751, .F. ) ;
#21671 = EDGE_CURVE ( 'NONE', #8189, #584, #26843, .T. ) ;
#21672 = CARTESIAN_POINT ( 'NONE',  ( 6.669130659221032431, -101.2111896145234340, 14.91624109844728707 ) ) ;
#21673 = AXIS2_PLACEMENT_3D ( 'NONE', #12102, #9918, #9777 ) ;
#21674 = CARTESIAN_POINT ( 'NONE',  ( -1.067886454847412958, -79.90307488451320239, 47.17292579724168888 ) ) ;
#21675 = ADVANCED_FACE ( 'NONE', ( #18241 ), #12622, .T. ) ;
#21676 = ORIENTED_EDGE ( 'NONE', *, *, #7329, .F. ) ;
#21677 = CARTESIAN_POINT ( 'NONE',  ( -12.08584015489836183, -69.49854784199777669, -25.11440668764106121 ) ) ;
#21678 = CARTESIAN_POINT ( 'NONE',  ( -20.42407875355905134, -94.65351867482938530, 12.05937522786372185 ) ) ;
#21679 = VERTEX_POINT ( 'NONE', #25659 ) ;
#21680 = CARTESIAN_POINT ( 'NONE',  ( 28.56790285990000200, -92.99999932720000118, 8.526057022789998996 ) ) ;
#21681 = CARTESIAN_POINT ( 'NONE',  ( 3.166345171159999694, -101.1889999979999999, -25.30265318609999881 ) ) ;
#21682 = CARTESIAN_POINT ( 'NONE',  ( -7.260248548399999891, -73.97917265380000629, -40.03821526680000176 ) ) ;
#21683 = VERTEX_POINT ( 'NONE', #1209 ) ;
#21684 = CARTESIAN_POINT ( 'NONE',  ( -5.025833696325614497, -96.36359510987577437, -21.36185927323176159 ) ) ;
#21685 = CARTESIAN_POINT ( 'NONE',  ( 22.60430443959684510, -36.06167118559999807, -10.71318590909911528 ) ) ;
#21686 = DIRECTION ( 'NONE',  ( 0.7071067811865470176, 0.000000000000000000, 0.7071067811865480168 ) ) ;
#21687 = CARTESIAN_POINT ( 'NONE',  ( -41.99080665327601736, -63.35144866726079016, -0.9204318062483302088 ) ) ;
#21688 = DIRECTION ( 'NONE',  ( 0.4794255386042038936, 0.000000000000000000, 0.8775825618903723147 ) ) ;
#21689 = VERTEX_POINT ( 'NONE', #18828 ) ;
#21690 = CARTESIAN_POINT ( 'NONE',  ( -22.22671705529999997, -94.70873613630000420, -8.207212726500001665 ) ) ;
#21691 = CARTESIAN_POINT ( 'NONE',  ( 12.38290840660000036, -101.0875971110000080, -9.170880648609999852 ) ) ;
#21692 = CARTESIAN_POINT ( 'NONE',  ( -8.841308419197195789, -80.50000000000000000, 38.90215371868703187 ) ) ;
#21693 = CARTESIAN_POINT ( 'NONE',  ( 23.79916314309999947, -94.54647010780000471, -7.453462340879999815 ) ) ;
#21694 = FACE_OUTER_BOUND ( 'NONE', #3595, .T. ) ;
#21695 = CARTESIAN_POINT ( 'NONE',  ( 29.97548914054884506, -92.50000000000001421, 5.633735048817801072 ) ) ;
#21696 = DIRECTION ( 'NONE',  ( -0.000000000000000000, 1.000000000000000000, 0.000000000000000000 ) ) ;
#21697 = EDGE_LOOP ( 'NONE', ( #11008, #2635, #16651, #20257 ) ) ;
#21698 = CARTESIAN_POINT ( 'NONE',  ( 0.000000000000000000, -10.95575221240000019, 0.000000000000000000 ) ) ;
#21699 = CARTESIAN_POINT ( 'NONE',  ( -18.80176912509999809, -93.00000000000000000, 23.77750384849999676 ) ) ;
#21700 = DIRECTION ( 'NONE',  ( 0.000000000000000000, 1.000000000000000000, 0.000000000000000000 ) ) ;
#21701 = CARTESIAN_POINT ( 'NONE',  ( 19.09701464850000008, -18.50000000000000000, 9.226637575699999871 ) ) ;
#21702 = CARTESIAN_POINT ( 'NONE',  ( 0.05579740145615928043, -92.84927079008861028, -30.49995016637035761 ) ) ;
#21703 = ADVANCED_FACE ( 'NONE', ( #18534 ), #26602, .F. ) ;
#21704 = DIRECTION ( 'NONE',  ( 0.000000000000000000, 0.000000000000000000, 1.000000000000000000 ) ) ;
#21705 = DIRECTION ( 'NONE',  ( 0.9295286103719527793, 0.000000000000000000, 0.3687499999999814260 ) ) ;
#21706 = EDGE_CURVE ( 'NONE', #1954, #3056, #11230, .T. ) ;
#21707 = ADVANCED_FACE ( 'NONE', ( #5130 ), #15404, .F. ) ;
#21708 = ORIENTED_EDGE ( 'NONE', *, *, #9238, .T. ) ;
#21709 = DIRECTION ( 'NONE',  ( 1.000000000000000000, 0.000000000000000000, 0.000000000000000000 ) ) ;
#21710 = CARTESIAN_POINT ( 'NONE',  ( 19.55164490770000185, -35.69157978159999800, -9.020399939569999859 ) ) ;
#21711 = VERTEX_POINT ( 'NONE', #3515 ) ;
#21712 = CARTESIAN_POINT ( 'NONE',  ( 19.55068585879999787, -35.72724450129999951, -9.038647844319999791 ) ) ;
#21713 = FACE_OUTER_BOUND ( 'NONE', #9685, .T. ) ;
#21714 = VERTEX_POINT ( 'NONE', #9628 ) ;
#21715 = CARTESIAN_POINT ( 'NONE',  ( -12.96301527429999823, -100.9938510739999913, -8.551186485709999729 ) ) ;
#21716 = DIRECTION ( 'NONE',  ( 0.000000000000000000, 1.000000000000000000, 0.000000000000000000 ) ) ;
#21717 = CARTESIAN_POINT ( 'NONE',  ( -8.209463909749999289, -99.53431386179998697, 15.35748980570000022 ) ) ;
#21718 = EDGE_LOOP ( 'NONE', ( #25490, #20530, #9786, #11743 ) ) ;
#21719 = CARTESIAN_POINT ( 'NONE',  ( -2.903042209430000131, -94.98812656900000206, 23.52859605189999925 ) ) ;
#21720 = DIRECTION ( 'NONE',  ( 1.000000000000000000, 0.000000000000000000, 0.000000000000000000 ) ) ;
#21721 = CARTESIAN_POINT ( 'NONE',  ( -9.752576846380001996, -18.50000000000000000, -19.83503857510000046 ) ) ;
#21722 = FACE_OUTER_BOUND ( 'NONE', #6415, .T. ) ;
#21723 = VERTEX_POINT ( 'NONE', #10043 ) ;
#21724 = CARTESIAN_POINT ( 'NONE',  ( 13.00837423133404158, -101.2637735886917625, -9.819042233897015137 ) ) ;
#21725 = CARTESIAN_POINT ( 'NONE',  ( 23.42943742290000131, -42.25468912520000231, 0.9114797856909999663 ) ) ;
#21726 = CARTESIAN_POINT ( 'NONE',  ( 22.90783306289999999, -66.63438074019998680, 12.00069599370000084 ) ) ;
#21727 = CARTESIAN_POINT ( 'NONE',  ( -15.62855498089999884, -101.6223710729999965, 3.522773483530000416 ) ) ;
#21728 = VERTEX_POINT ( 'NONE', #27582 ) ;
#21729 = FACE_OUTER_BOUND ( 'NONE', #476, .T. ) ;
#21730 = DIRECTION ( 'NONE',  ( 0.000000000000000000, 1.000000000000000000, 0.000000000000000000 ) ) ;
#21731 = LINE ( 'NONE', #1368, #21808 ) ;
#21732 = DIRECTION ( 'NONE',  ( 1.000000000000000000, 0.000000000000000000, 0.000000000000000000 ) ) ;
#21733 = VERTEX_POINT ( 'NONE', #18957 ) ;
#21734 = CIRCLE ( 'NONE', #13838, 12.00000000000000000 ) ;
#21735 = VECTOR ( 'NONE', #1395, 1000.000000000000000 ) ;
#21736 = FACE_OUTER_BOUND ( 'NONE', #12966, .T. ) ;
#21737 = DIRECTION ( 'NONE',  ( 1.000000000000000000, 0.000000000000000000, 0.000000000000000000 ) ) ;
#21738 = CARTESIAN_POINT ( 'NONE',  ( 26.73328265790000202, -93.00000450890000536, -12.41349335419999989 ) ) ;
#21739 = CARTESIAN_POINT ( 'NONE',  ( 15.14237901210000103, -101.1411470200000053, 2.745305927470000018 ) ) ;
#21740 = DIRECTION ( 'NONE',  ( -0.9852992387259376095, 0.000000000000000000, 0.1708373792999886009 ) ) ;
#21741 = CARTESIAN_POINT ( 'NONE',  ( -37.43882116139999994, -65.49083508809999898, 0.5420286502519999772 ) ) ;
#21742 = VERTEX_POINT ( 'NONE', #19096 ) ;
#21743 = EDGE_CURVE ( 'NONE', #10083, #8407, #20562, .T. ) ;
#21744 = CARTESIAN_POINT ( 'NONE',  ( 6.612443239639999248, -100.9678331089999972, 14.76866989470000213 ) ) ;
#21745 = CARTESIAN_POINT ( 'NONE',  ( 14.89070032189999893, -101.0875971110000080, 3.963397078339999879 ) ) ;
#21746 = AXIS2_PLACEMENT_3D ( 'NONE', #23479, #14845, #3927 ) ;
#21747 = CARTESIAN_POINT ( 'NONE',  ( 20.63161943080000071, -19.46510050319999863, -7.734358783100000245 ) ) ;
#21748 = CARTESIAN_POINT ( 'NONE',  ( 5.025650632445116450, -92.66455718074428205, -30.08309967992143896 ) ) ;
#21749 = DIRECTION ( 'NONE',  ( 0.9704142011833034598, 0.000000000000000000, -0.2414462220490750377 ) ) ;
#21750 = VERTEX_POINT ( 'NONE', #5416 ) ;
#21751 = CARTESIAN_POINT ( 'NONE',  ( 1.798767253769999908, -92.50732182800000203, -29.41797783070000349 ) ) ;
#21752 = DIRECTION ( 'NONE',  ( 0.000000000000000000, -1.000000000000000000, 0.000000000000000000 ) ) ;
#21753 = CIRCLE ( 'NONE', #9186, 7.750000000000000000 ) ;
#21754 = CARTESIAN_POINT ( 'NONE',  ( -1.108943289259999965, -101.2141467319999890, -15.20603369630000046 ) ) ;
#21755 = DIRECTION ( 'NONE',  ( 1.000000000000000000, 0.000000000000000000, -1.665334536939999828E-16 ) ) ;
#21756 = ORIENTED_EDGE ( 'NONE', *, *, #5630, .T. ) ;
#21757 = CARTESIAN_POINT ( 'NONE',  ( -12.17175180279999935, -57.47855601759999900, -19.93971687999999887 ) ) ;
#21758 = CARTESIAN_POINT ( 'NONE',  ( -12.59800300965208208, -100.8945630382227989, -10.79107909087879769 ) ) ;
#21759 = ORIENTED_EDGE ( 'NONE', *, *, #24577, .F. ) ;
#21760 = CARTESIAN_POINT ( 'NONE',  ( 23.56050310359999855, -94.79581646409999962, -2.314011072670000058 ) ) ;
#21761 = EDGE_LOOP ( 'NONE', ( #19153, #22463, #25990, #6011 ) ) ;
#21762 = CARTESIAN_POINT ( 'NONE',  ( -1.325730538359999988, -100.9728541479999961, -15.54355591019999849 ) ) ;
#21763 = EDGE_CURVE ( 'NONE', #3841, #2153, #18725, .T. ) ;
#21764 = DIRECTION ( 'NONE',  ( 0.000000000000000000, 1.000000000000000000, 0.000000000000000000 ) ) ;
#21765 = DIRECTION ( 'NONE',  ( 0.1237356522920125546, 0.000000000000000000, -0.9923152162251016595 ) ) ;
#21766 = CARTESIAN_POINT ( 'NONE',  ( 12.82422237299999956, -94.98812477769999418, -19.93894812050000098 ) ) ;
#21767 = DIRECTION ( 'NONE',  ( 0.000000000000000000, 1.000000000000000000, 0.000000000000000000 ) ) ;
#21768 = AXIS2_PLACEMENT_3D ( 'NONE', #9670, #11861, #1245 ) ;
#21769 = ORIENTED_EDGE ( 'NONE', *, *, #3002, .F. ) ;
#21770 = CARTESIAN_POINT ( 'NONE',  ( 15.04861839279999991, -100.9137139110000021, 4.234011249179999936 ) ) ;
#21771 = CARTESIAN_POINT ( 'NONE',  ( -22.67747013279999990, -69.73397779950001052, 15.15635250419999913 ) ) ;
#21772 = B_SPLINE_CURVE_WITH_KNOTS ( 'NONE', 5,
 ( #28148, #19261, #21727, #1777, #10620, #19536, #26391, #26255, #6278, #12960, #1507, #6420 ),
 .UNSPECIFIED., .F., .F.,
 ( 6, 3, 3, 6 ),
 ( 0.000000000000000000, 0.2661689441622204222, 0.5687008854760363663, 1.000000000000000000 ),
 .UNSPECIFIED. ) ;
#21773 = CARTESIAN_POINT ( 'NONE',  ( -12.78693177215897236, -101.2404586421391173, -9.286964095330146662 ) ) ;
#21774 = CARTESIAN_POINT ( 'NONE',  ( 13.76083776420598248, -100.1240332945478144, -10.32414654847229762 ) ) ;
#21775 = CARTESIAN_POINT ( 'NONE',  ( -19.02940910017253273, -19.48522775728694612, 13.93404945096885683 ) ) ;
#21776 = CARTESIAN_POINT ( 'NONE',  ( 7.146354963110000291, -36.17740051239999843, -21.48176990560000021 ) ) ;
#21777 = FACE_BOUND ( 'NONE', #9064, .T. ) ;
#21778 = VERTEX_POINT ( 'NONE', #14438 ) ;
#21779 = CARTESIAN_POINT ( 'NONE',  ( 36.62466543389999885, -74.65121094670000446, -14.68734461939999925 ) ) ;
#21780 = CARTESIAN_POINT ( 'NONE',  ( 21.78369645919999797, -36.06096454580000454, -10.41102218880000052 ) ) ;
#21781 = CARTESIAN_POINT ( 'NONE',  ( -1.156338024719999913, -58.78702526330000211, -23.48034166449999915 ) ) ;
#21782 = AXIS2_PLACEMENT_3D ( 'NONE', #17627, #6556, #24326 ) ;
#21783 = CARTESIAN_POINT ( 'NONE',  ( -26.99515064810000098, -93.07154530319999708, -0.5147607136670000472 ) ) ;
#21784 = CARTESIAN_POINT ( 'NONE',  ( -19.87158930579999705, -56.22908209860000284, 14.19280044929999995 ) ) ;
#21785 = CYLINDRICAL_SURFACE ( 'NONE', #23413, 16.00000000000000000 ) ;
#21786 = ORIENTED_EDGE ( 'NONE', *, *, #8960, .F. ) ;
#21787 = CARTESIAN_POINT ( 'NONE',  ( -17.89732362545216660, -97.43022994619724386, -10.14686946726538608 ) ) ;
#21788 = CARTESIAN_POINT ( 'NONE',  ( -13.14571738459999928, -100.8733984769999950, -8.628956128260000469 ) ) ;
#21789 = ORIENTED_EDGE ( 'NONE', *, *, #4069, .T. ) ;
#21790 = PLANE ( 'NONE',  #17296 ) ;
#21791 = CIRCLE ( 'NONE', #28297, 57.75000000000000000 ) ;
#21792 = FACE_OUTER_BOUND ( 'NONE', #10554, .T. ) ;
#21793 = CONICAL_SURFACE ( 'NONE', #24123, 21.60095686220001454, 0.7949521073230001456 ) ;
#21794 = CARTESIAN_POINT ( 'NONE',  ( 22.16575857890000023, -39.31812514059999586, 9.877484424130001273 ) ) ;
#21795 = CARTESIAN_POINT ( 'NONE',  ( -22.12521137138542215, -74.07932799455450379, -32.40737826886834938 ) ) ;
#21796 = EDGE_CURVE ( 'NONE', #22782, #11457, #3376, .T. ) ;
#21797 = CARTESIAN_POINT ( 'NONE',  ( 21.61044917590000480, -19.17414499179999865, 9.484325925899998566 ) ) ;
#21798 = CARTESIAN_POINT ( 'NONE',  ( -32.42291149912640691, -74.08416876105088988, -22.12919252830631933 ) ) ;
#21799 = CARTESIAN_POINT ( 'NONE',  ( -20.08103059729999984, -57.43018248439999951, 14.46712379729999931 ) ) ;
#21800 = ORIENTED_EDGE ( 'NONE', *, *, #24795, .F. ) ;
#21801 = CARTESIAN_POINT ( 'NONE',  ( -11.86518140747143235, -72.15620726827764031, -26.36366794161594385 ) ) ;
#21802 = CARTESIAN_POINT ( 'NONE',  ( -11.89545460579999947, -101.2530993010000060, -9.453770335970000716 ) ) ;
#21803 = ADVANCED_FACE ( 'NONE', ( #27426 ), #14570, .F. ) ;
#21804 = PRESENTATION_STYLE_ASSIGNMENT (( #2006 ) ) ;
#21805 = CARTESIAN_POINT ( 'NONE',  ( -7.068540044037536774, -101.5740747342563850, 14.41783971523548047 ) ) ;
#21806 = ORIENTED_EDGE ( 'NONE', *, *, #12761, .F. ) ;
#21807 = EDGE_CURVE ( 'NONE', #6300, #8623, #3657, .T. ) ;
#21808 = VECTOR ( 'NONE', #28283, 1000.000000000000000 ) ;
#21809 = FACE_OUTER_BOUND ( 'NONE', #9443, .T. ) ;
#21810 = CARTESIAN_POINT ( 'NONE',  ( -31.99064106590000023, -74.00000000000000000, -21.95840602359999849 ) ) ;
#21811 = ORIENTED_EDGE ( 'NONE', *, *, #13377, .F. ) ;
#21812 = CIRCLE ( 'NONE', #12947, 38.75000000000000000 ) ;
#21813 = AXIS2_PLACEMENT_3D ( 'NONE', #21085, #21493, #3578 ) ;
#21814 = CIRCLE ( 'NONE', #14346, 3.750000000000000000 ) ;
#21815 = CIRCLE ( 'NONE', #457, 21.14285714289999873 ) ;
#21816 = DIRECTION ( 'NONE',  ( 0.000000000000000000, 1.000000000000000000, 0.000000000000000000 ) ) ;
#21817 = CARTESIAN_POINT ( 'NONE',  ( -5.487412872479999315, -100.8733984769999950, 14.73625018059999903 ) ) ;
#21818 = CARTESIAN_POINT ( 'NONE',  ( 27.68147801010000109, -38.34400911419999858, 50.67060561630000137 ) ) ;
#21819 = ORIENTED_EDGE ( 'NONE', *, *, #22719, .F. ) ;
#21820 = CARTESIAN_POINT ( 'NONE',  ( -15.59829199139345413, -93.74885976911515684, -21.59132595434880031 ) ) ;
#21821 = ORIENTED_EDGE ( 'NONE', *, *, #11307, .T. ) ;
#21822 = CARTESIAN_POINT ( 'NONE',  ( 22.84303034490000073, -56.20810645120000260, 10.22595161340000125 ) ) ;
#21823 = ORIENTED_EDGE ( 'NONE', *, *, #24144, .T. ) ;
#21824 = CARTESIAN_POINT ( 'NONE',  ( 9.885503723209998483, -36.00000000000000000, -20.33566493420000043 ) ) ;
#21825 = CARTESIAN_POINT ( 'NONE',  ( -3.108624468950000298E-16, -74.00000000000000000, -1.554312234480000048E-16 ) ) ;
#21826 = TOROIDAL_SURFACE ( 'NONE', #1834, 55.85192378860000417, 0.3499999999999999778 ) ;
#21827 = CARTESIAN_POINT ( 'NONE',  ( 8.685017520700000659, -37.33819206249999922, -21.91842612469999807 ) ) ;
#21828 = CARTESIAN_POINT ( 'NONE',  ( -20.51427898140000394, -93.04780269089999933, -20.71378216980000175 ) ) ;
#21829 = CARTESIAN_POINT ( 'NONE',  ( 24.70601165868461990, -65.70112750257325729, 10.85168987944911656 ) ) ;
#21830 = EDGE_LOOP ( 'NONE', ( #13414, #5095, #23063, #25322, #5276, #5139 ) ) ;
#21832 = ADVANCED_FACE ( 'NONE', ( #14009 ), #26149, .F. ) ;
#21831 = CIRCLE ( 'NONE', #27463, 3.749999999999996447 ) ;
#21833 = CIRCLE ( 'NONE', #12064, 9.499999999999998224 ) ;
#21834 = CARTESIAN_POINT ( 'NONE',  ( -32.20769381560000255, -80.34292075950000367, -22.43272066100000117 ) ) ;
#21835 = CARTESIAN_POINT ( 'NONE',  ( 12.43657857140000011, -101.0151300849999814, -9.480717691399998870 ) ) ;
#21836 = CARTESIAN_POINT ( 'NONE',  ( 4.426600958609999879E-15, -69.00000000000000000, 43.75000000000000000 ) ) ;
#21837 = CARTESIAN_POINT ( 'NONE',  ( -1.993723132830000244, -52.61368720150000655, -23.68602550419999986 ) ) ;
#21838 = EDGE_CURVE ( 'NONE', #14636, #10981, #930, .T. ) ;
#21839 = CARTESIAN_POINT ( 'NONE',  ( 29.92224321301734946, -92.52048598158077652, 5.908436733558301235 ) ) ;
#21840 = CARTESIAN_POINT ( 'NONE',  ( -19.12703695859999797, -18.50000000000000000, 14.91269771249999998 ) ) ;
#21841 = ORIENTED_EDGE ( 'NONE', *, *, #11193, .T. ) ;
#21842 = EDGE_CURVE ( 'NONE', #7826, #19383, #25900, .T. ) ;
#21843 = DIRECTION ( 'NONE',  ( 1.000000000000000000, 0.000000000000000000, 0.000000000000000000 ) ) ;
#21844 = CARTESIAN_POINT ( 'NONE',  ( 20.30102379280000235, -72.00000000000000000, -30.97095677779999789 ) ) ;
#21845 = CARTESIAN_POINT ( 'NONE',  ( 4.656214649959999954E-15, -79.00000000000000000, 40.00000000000000000 ) ) ;
#21846 = CARTESIAN_POINT ( 'NONE',  ( 21.00696503170000184, -18.50000000000000000, 8.444293349240000524 ) ) ;
#21847 = CARTESIAN_POINT ( 'NONE',  ( -40.00000000000000000, -82.25000000000000000, 0.000000000000000000 ) ) ;
#21848 = SHAPE_DEFINITION_REPRESENTATION ( #5706, #10908 ) ;
#21849 = CARTESIAN_POINT ( 'NONE',  ( -11.60601438770000016, -94.60987696080000831, -20.74983651260000173 ) ) ;
#21850 = AXIS2_PLACEMENT_3D ( 'NONE', #13096, #17638, #28553 ) ;
#21851 = CIRCLE ( 'NONE', #27923, 25.11294200180000047 ) ;
#21852 = ORIENTED_EDGE ( 'NONE', *, *, #1888, .T. ) ;
#21853 = CARTESIAN_POINT ( 'NONE',  ( 0.000000000000000000, -19.09689110869999951, 0.000000000000000000 ) ) ;
#21854 = DIRECTION ( 'NONE',  ( 0.8775825618903722036, 0.000000000000000000, -0.4794255386042041156 ) ) ;
#21855 = ORIENTED_EDGE ( 'NONE', *, *, #27910, .F. ) ;
#21856 = CARTESIAN_POINT ( 'NONE',  ( 21.50685431550000004, -37.36994930320000208, -7.661821680550000124 ) ) ;
#21857 = DIRECTION ( 'NONE',  ( 0.000000000000000000, -1.000000000000000000, 0.000000000000000000 ) ) ;
#21858 = ORIENTED_EDGE ( 'NONE', *, *, #27055, .F. ) ;
#21859 = CARTESIAN_POINT ( 'NONE',  ( -12.94585355969999974, -101.5369810359999860, -9.402386697489999889 ) ) ;
#21860 = CARTESIAN_POINT ( 'NONE',  ( -3.378235408309124388, -68.15838326003131442, -27.58918776656260619 ) ) ;
#21861 = DIRECTION ( 'NONE',  ( 0.000000000000000000, 1.000000000000000000, 0.000000000000000000 ) ) ;
#21862 = VERTEX_POINT ( 'NONE', #9914 ) ;
#21863 = CARTESIAN_POINT ( 'NONE',  ( -1.640146184310000033, -93.85307999910000376, 24.85263355689999898 ) ) ;
#21864 = EDGE_CURVE ( 'NONE', #8967, #11422, #14450, .T. ) ;
#21865 = CARTESIAN_POINT ( 'NONE',  ( -30.40361236680223200, -92.82334897394798645, 2.422884163522351919 ) ) ;
#21866 = CARTESIAN_POINT ( 'NONE',  ( 40.65853658540000026, -84.00000000000000000, 6.717799458580000049 ) ) ;
#21867 = CARTESIAN_POINT ( 'NONE',  ( -10.53872106220000049, -18.50000000000000000, -18.20862928879999743 ) ) ;
#21868 = CARTESIAN_POINT ( 'NONE',  ( -39.57283196047948337, -65.66839995188320245, 2.267351524782069472 ) ) ;
#21869 = EDGE_LOOP ( 'NONE', ( #14712, #25672 ) ) ;
#21870 = EDGE_CURVE ( 'NONE', #24612, #26673, #4206, .T. ) ;
#21871 = CARTESIAN_POINT ( 'NONE',  ( 13.63023407945182619, -100.4166221066929836, -10.10576425320335048 ) ) ;
#21872 = CARTESIAN_POINT ( 'NONE',  ( 23.29682936289999873, -49.86909869750000013, 0.3487798571490000055 ) ) ;
#21873 = CARTESIAN_POINT ( 'NONE',  ( 22.77339862950000082, -64.89165510060000486, 10.97889282110000053 ) ) ;
#21874 = CARTESIAN_POINT ( 'NONE',  ( 38.90877162584872906, -73.50999119020812600, 7.168130346644877804 ) ) ;
#21875 = ORIENTED_EDGE ( 'NONE', *, *, #22419, .T. ) ;
#21876 = EDGE_CURVE ( 'NONE', #7380, #4012, #21560, .T. ) ;
#21877 = CARTESIAN_POINT ( 'NONE',  ( -38.68350751799999898, -73.93831497249999529, 7.318372426699999878 ) ) ;
#21878 = CARTESIAN_POINT ( 'NONE',  ( -17.23516852259999865, -93.34894302420001111, 19.23197678129999844 ) ) ;
#21879 = CARTESIAN_POINT ( 'NONE',  ( -20.53595003809872566, -92.95311892457516478, 17.44055191160039797 ) ) ;
#21880 = ORIENTED_EDGE ( 'NONE', *, *, #23715, .F. ) ;
#21881 = CIRCLE ( 'NONE', #26078, 57.75000000000000000 ) ;
#21882 = EDGE_CURVE ( 'NONE', #19526, #3430, #14975, .T. ) ;
#21883 = CARTESIAN_POINT ( 'NONE',  ( 27.79198761910000215, -68.38614792650000140, 2.092073158110000275 ) ) ;
#21884 = CARTESIAN_POINT ( 'NONE',  ( 0.6097187718590001415, -100.7430069139999915, -16.48132026290000240 ) ) ;
#21885 = CARTESIAN_POINT ( 'NONE',  ( 9.368358256079998725, -60.33817349190000101, -23.16693853690000182 ) ) ;
#21886 = CARTESIAN_POINT ( 'NONE',  ( 15.25760145080000107, -101.1292389600000092, 2.766195699469999436 ) ) ;
#21887 = DIRECTION ( 'NONE',  ( 1.000000000000000000, 0.000000000000000000, 0.000000000000000000 ) ) ;
#21888 = CARTESIAN_POINT ( 'NONE',  ( -11.90025794910000023, -42.27249569760000014, -19.48331447349999834 ) ) ;
#21889 = ORIENTED_EDGE ( 'NONE', *, *, #23981, .F. ) ;
#21890 = B_SPLINE_CURVE_WITH_KNOTS ( 'NONE', 5,
 ( #28386, #5951, #17470, #15247, #8417, #14835 ),
 .UNSPECIFIED., .F., .F.,
 ( 6, 6 ),
 ( 0.000000000000000000, 1.000000000000000000 ),
 .UNSPECIFIED. ) ;
#21891 = CARTESIAN_POINT ( 'NONE',  ( 6.435168149109999902, -100.5717442099999914, 15.00978900200000155 ) ) ;
#21892 = CARTESIAN_POINT ( 'NONE',  ( -15.60056067142878788, -92.58043237596167785, -24.03344884106981993 ) ) ;
#21893 = CARTESIAN_POINT ( 'NONE',  ( -17.19936155160000268, -93.49273751280000511, 18.87523342240000090 ) ) ;
#21894 = CARTESIAN_POINT ( 'NONE',  ( 5.095278765311285873, -92.64884742706659893, -30.07140691049922410 ) ) ;
#21895 = CARTESIAN_POINT ( 'NONE',  ( -42.25000000000000000, -65.63577453799999262, -0.7216878364880000563 ) ) ;
#21896 = ORIENTED_EDGE ( 'NONE', *, *, #28767, .T. ) ;
#21897 = CARTESIAN_POINT ( 'NONE',  ( 6.262252868900000102, -92.98481302140000082, -25.92940123820000053 ) ) ;
#21898 = CIRCLE ( 'NONE', #17264, 0.5000000000000004441 ) ;
#21899 = CIRCLE ( 'NONE', #3743, 0.4999999999999990563 ) ;
#21900 = CARTESIAN_POINT ( 'NONE',  ( 20.42956111930000063, -25.51643932219999655, -8.516251604709999867 ) ) ;
#21901 = CARTESIAN_POINT ( 'NONE',  ( -8.841308419149999764, -80.00000000000000000, 38.90215371869999927 ) ) ;
#21902 = CARTESIAN_POINT ( 'NONE',  ( -6.929612297000000254, -101.5216621940000152, 14.43317662559999981 ) ) ;
#21903 = ORIENTED_EDGE ( 'NONE', *, *, #13361, .T. ) ;
#21904 = CARTESIAN_POINT ( 'NONE',  ( -11.58789126345519982, -27.06771711593889407, -19.05193615919498740 ) ) ;
#21905 = B_SPLINE_CURVE_WITH_KNOTS ( 'NONE', 3,
 ( #7925, #1113, #27319, #20909, #9813, #10081, #12136, #21054, #20768, #5594, #16526, #14475, #5455, #9951, #7359, #18865, #23372, #19000 ),
 .UNSPECIFIED., .F., .F.,
 ( 4, 2, 2, 2, 1, 1, 1, 1, 2, 2, 4 ),
 ( 0.000000000000000000, 0.2500000000000449085, 0.3750000000000673905, 0.4375000000000786038, 0.4687500000000842104, 0.4843750000000877631, 0.4921875000000898170, 0.4960937500000907607, 0.4980468750000903166, 0.5000000000000898170, 1.000000000000000000 ),
 .UNSPECIFIED. ) ;
#21906 = CARTESIAN_POINT ( 'NONE',  ( -36.23922253580000330, -79.50000000000000000, -27.04683438039999999 ) ) ;
#21907 = ORIENTED_EDGE ( 'NONE', *, *, #22826, .T. ) ;
#21908 = CARTESIAN_POINT ( 'NONE',  ( 9.056984553609998656, -35.76308213440000117, -19.54972227260000039 ) ) ;
#21909 = CARTESIAN_POINT ( 'NONE',  ( 19.97576656849999921, -72.00000000000000000, -19.97576656849999921 ) ) ;
#21910 = EDGE_CURVE ( 'NONE', #22153, #7941, #23813, .T. ) ;
#21911 = CARTESIAN_POINT ( 'NONE',  ( -1.247133441849999969, -101.2306315440000049, -16.16540283980000225 ) ) ;
#21912 = CARTESIAN_POINT ( 'NONE',  ( 21.03849606329999844, -18.50000000000000000, -0.02248551888909999796 ) ) ;
#21913 = DIRECTION ( 'NONE',  ( 1.000000000000000000, 0.000000000000000000, 0.000000000000000000 ) ) ;
#21914 = CARTESIAN_POINT ( 'NONE',  ( -40.50000000000000000, -11.00000000000000000, 4.500000000000000000 ) ) ;
#21915 = ORIENTED_EDGE ( 'NONE', *, *, #9637, .T. ) ;
#21916 = EDGE_CURVE ( 'NONE', #19618, #5266, #5425, .T. ) ;
#21917 = CARTESIAN_POINT ( 'NONE',  ( -15.42268928690000074, -101.6484615499999933, 4.259183627459999677 ) ) ;
#21918 = CARTESIAN_POINT ( 'NONE',  ( -6.569756907160000381, -101.2530993010000060, 13.70087252790000143 ) ) ;
#21919 = CYLINDRICAL_SURFACE ( 'NONE', #21573, 7.249999999999999112 ) ;
#21920 = CARTESIAN_POINT ( 'NONE',  ( 29.17304402409999753, -10.00000000000000000, 53.40089889099999709 ) ) ;
#21921 = DIRECTION ( 'NONE',  ( 0.000000000000000000, -1.000000000000000000, 0.000000000000000000 ) ) ;
#21922 = DIRECTION ( 'NONE',  ( 0.000000000000000000, 1.000000000000000000, 0.000000000000000000 ) ) ;
#21923 = CARTESIAN_POINT ( 'NONE',  ( 24.29194483483871636, -94.04667188331129069, -9.262494893684873887 ) ) ;
#21924 = CARTESIAN_POINT ( 'NONE',  ( 19.26850085170000071, -29.42970386789999893, -8.998040626839999945 ) ) ;
#21925 = AXIS2_PLACEMENT_3D ( 'NONE', #969, #10216, #16656 ) ;
#21926 = ORIENTED_EDGE ( 'NONE', *, *, #20609, .F. ) ;
#21927 = AXIS2_PLACEMENT_3D ( 'NONE', #4818, #13696, #22598 ) ;
#21928 = CARTESIAN_POINT ( 'NONE',  ( -10.85248982675889273, -18.97801304286212343, -21.92849394884687086 ) ) ;
#21929 = CIRCLE ( 'NONE', #24258, 0.4999999999999982236 ) ;
#21930 = CARTESIAN_POINT ( 'NONE',  ( 22.15413943410000286, -37.05706116329999134, -9.219199529280000860 ) ) ;
#21931 = VERTEX_POINT ( 'NONE', #25802 ) ;
#21932 = ADVANCED_FACE ( 'NONE', ( #10453, #28247 ), #19788, .T. ) ;
#21933 = CARTESIAN_POINT ( 'NONE',  ( -0.8798048959290000193, -61.87790347820000392, -23.94595848790000048 ) ) ;
#21934 = CARTESIAN_POINT ( 'NONE',  ( -26.75452624049999883, -92.97898997910000674, -0.3867577180200000297 ) ) ;
#21935 = CARTESIAN_POINT ( 'NONE',  ( -19.84861352869999962, -53.84434310259999279, 12.07737518400000098 ) ) ;
#21936 = DIRECTION ( 'NONE',  ( -0.2414462220490755373, 0.000000000000000000, -0.9704142011833032377 ) ) ;
#21937 = VERTEX_POINT ( 'NONE', #12646 ) ;
#21938 = AXIS2_PLACEMENT_3D ( 'NONE', #26136, #28176, #12842 ) ;
#21939 = CARTESIAN_POINT ( 'NONE',  ( 21.28729238020000025, -35.15980207439999816, -7.664900974450000071 ) ) ;
#21940 = CARTESIAN_POINT ( 'NONE',  ( -16.67828388959999941, -74.00000000000000000, 44.75374114529999758 ) ) ;
#21941 = ORIENTED_EDGE ( 'NONE', *, *, #18097, .F. ) ;
#21942 = AXIS2_PLACEMENT_3D ( 'NONE', #22470, #2514, #16184 ) ;
#21943 = CARTESIAN_POINT ( 'NONE',  ( 7.693905362600673925, -37.38950372099960617, -21.51648389446061316 ) ) ;
#21944 = B_SPLINE_CURVE_WITH_KNOTS ( 'NONE', 5,
 ( #6018, #28042, #3568, #12426, #21339, #10240, #19155, #15172, #23949 ),
 .UNSPECIFIED., .F., .F.,
 ( 6, 3, 6 ),
 ( 0.000000000000000000, 0.5000000000000000000, 1.000000000000000000 ),
 .UNSPECIFIED. ) ;
#21945 = ORIENTED_EDGE ( 'NONE', *, *, #22654, .F. ) ;
#21946 = ADVANCED_FACE ( 'NONE', ( #1744 ), #14840, .F. ) ;
#21947 = FACE_OUTER_BOUND ( 'NONE', #27305, .T. ) ;
#21948 = CARTESIAN_POINT ( 'NONE',  ( 20.85236623999999850, -26.08233090739999938, 9.582502883489999235 ) ) ;
#21949 = DIRECTION ( 'NONE',  ( 1.000000000000000000, 0.000000000000000000, 0.000000000000000000 ) ) ;
#21950 = CARTESIAN_POINT ( 'NONE',  ( 22.13285133049999587, -19.49504784870000051, 9.709488547299999439 ) ) ;
#21951 = CARTESIAN_POINT ( 'NONE',  ( 9.438993784210000015, -64.72767716790001202, -23.93801147259999951 ) ) ;
#21952 = CARTESIAN_POINT ( 'NONE',  ( -17.54428855099999751, -94.59276292389999696, 16.07755916609999858 ) ) ;
#21953 = B_SPLINE_SURFACE_WITH_KNOTS ( 'NONE', 5, 5, ( 
 ( #4335, #22116, #10993, #2301, #4477, #4034, #21817, #1867, #19906 ),
 ( #17743, #19625, #11149, #27662, #7258, #866, #7403, #22699, #9276 ),
 ( #9856, #11449, #4776, #576, #2741, #9572, #13948, #14243, #22848 ),
 ( #3178, #12035, #2891, #9708, #16124, #23131, #16421, #2601, #1011 ),
 ( #18766, #27216, #24739, #16268, #14096, #18175, #13653, #25181, #11751 ),
 ( #22560, #27513, #25024, #11598, #5056, #20954, #18621, #20357, #20506 ) ),
 .UNSPECIFIED., .F., .F., .F.,
 ( 6, 6 ),
 ( 6, 3, 6 ),
 ( 10.27983904170000073, 28.98451592950000233 ),
 ( 0.000000000000000000, 0.2500000000000000000, 0.5000000000000000000 ),
 .UNSPECIFIED. ) ;
#21954 = ORIENTED_EDGE ( 'NONE', *, *, #6518, .T. ) ;
#21955 = CARTESIAN_POINT ( 'NONE',  ( -12.36776282346795597, -72.59721320749554252, -25.84214607925492402 ) ) ;
#21956 = CARTESIAN_POINT ( 'NONE',  ( -11.96873758509999952, -101.1030539030000028, -9.749858522220000268 ) ) ;
#21957 = SURFACE_SIDE_STYLE ('',( #8120 ) ) ;
#21958 = CARTESIAN_POINT ( 'NONE',  ( 22.36688849876826168, -59.04651452996991878, -7.100983198977605326 ) ) ;
#21959 = EDGE_LOOP ( 'NONE', ( #21444, #25579 ) ) ;
#21960 = CARTESIAN_POINT ( 'NONE',  ( 47.25000000000000000, -69.50000000000000000, 2.433892081919999696E-15 ) ) ;
#21961 = CARTESIAN_POINT ( 'NONE',  ( -32.51469473070000049, -74.18397341870000616, -21.79791327519999911 ) ) ;
#21962 = ORIENTED_EDGE ( 'NONE', *, *, #27354, .T. ) ;
#21963 = VECTOR ( 'NONE', #27628, 1000.000000000000000 ) ;
#21964 = EDGE_CURVE ( 'NONE', #25324, #27945, #25552, .T. ) ;
#21965 = CARTESIAN_POINT ( 'NONE',  ( 24.88097934669864131, -39.24428776213493109, 1.395120059140831037 ) ) ;
#21966 = ORIENTED_EDGE ( 'NONE', *, *, #6717, .F. ) ;
#21967 = CARTESIAN_POINT ( 'NONE',  ( -14.77445022520000073, -101.2530993010000060, 3.545507728379999612 ) ) ;
#21968 = CARTESIAN_POINT ( 'NONE',  ( -19.26870743061221347, -97.04550385075440033, 7.366219023504180008 ) ) ;
#21969 = EDGE_LOOP ( 'NONE', ( #27371, #9262, #27473, #636 ) ) ;
#21970 = CARTESIAN_POINT ( 'NONE',  ( 23.84088130539999995, -93.01125933519999478, 11.79630522170000084 ) ) ;
#21971 = CARTESIAN_POINT ( 'NONE',  ( 25.32712259480000228, -57.40875702469999453, 1.379782074460000230 ) ) ;
#21972 = ADVANCED_FACE ( 'NONE', ( #6388 ), #9885, .T. ) ;
#21973 = VERTEX_POINT ( 'NONE', #24318 ) ;
#21974 = CARTESIAN_POINT ( 'NONE',  ( -41.98619589785989348, -65.73347097107149750, 0.9353054002211724782 ) ) ;
#21975 = CARTESIAN_POINT ( 'NONE',  ( 1.678657213230000024E-14, -74.00000000000000000, 7.838174553849999450E-15 ) ) ;
#21976 = AXIS2_PLACEMENT_3D ( 'NONE', #26383, #6411, #12429 ) ;
#21977 = ORIENTED_EDGE ( 'NONE', *, *, #15529, .T. ) ;
#21978 = CARTESIAN_POINT ( 'NONE',  ( 9.237424541170000225, -36.00000000019999646, -20.64008957659999766 ) ) ;
#21979 = CARTESIAN_POINT ( 'NONE',  ( -11.46863496920000003, -57.40875702469999453, -22.62382260909999943 ) ) ;
#21980 = VECTOR ( 'NONE', #4011, 1000.000000000000000 ) ;
#21981 = CARTESIAN_POINT ( 'NONE',  ( -13.46646228700000059, -101.3150700380000018, -9.098096927170001180 ) ) ;
#21982 = ORIENTED_EDGE ( 'NONE', *, *, #19891, .F. ) ;
#21983 = DIRECTION ( 'NONE',  ( 0.000000000000000000, 1.000000000000000000, 0.000000000000000000 ) ) ;
#21984 = CARTESIAN_POINT ( 'NONE',  ( 12.86597616020000068, -100.8023006570000035, -9.130347141119999677 ) ) ;
#21985 = CARTESIAN_POINT ( 'NONE',  ( -18.26810397560000254, -94.98812477769999418, 16.32728546869999775 ) ) ;
#21986 = CARTESIAN_POINT ( 'NONE',  ( -2.583988345239999873, -57.40875702400000336, -25.23271569159999927 ) ) ;
#21987 = CARTESIAN_POINT ( 'NONE',  ( 26.66586753799999698, -92.50000000000000000, 13.56661073689999952 ) ) ;
#21988 = CARTESIAN_POINT ( 'NONE',  ( 11.31200901364189448, -72.30581792555656762, -26.97931566277052795 ) ) ;
#21989 = CARTESIAN_POINT ( 'NONE',  ( -4.439198032609999743E-16, -82.25000000000000000, 47.25000000000000000 ) ) ;
#21990 = ORIENTED_EDGE ( 'NONE', *, *, #4415, .F. ) ;
#21991 = DIRECTION ( 'NONE',  ( -0.9993816408608721114, 0.000000000000000000, 0.03516156865429537204 ) ) ;
#21992 = CARTESIAN_POINT ( 'NONE',  ( 0.000000000000000000, -11.50000000000000000, 0.000000000000000000 ) ) ;
#21993 = CARTESIAN_POINT ( 'NONE',  ( -23.89417554923151243, -92.74292563043789528, -18.95570639509220712 ) ) ;
#21994 = DIRECTION ( 'NONE',  ( 0.000000000000000000, 1.000000000000000000, 0.000000000000000000 ) ) ;
#21995 = CARTESIAN_POINT ( 'NONE',  ( 0.09048303299432611246, -92.89593097428102908, -30.49986667271737062 ) ) ;
#21996 = CARTESIAN_POINT ( 'NONE',  ( 79.28327401276546027, -3.469446951953614189E-15, -7.538194932341960808 ) ) ;
#21997 = CIRCLE ( 'NONE', #26120, 9.500000000000000000 ) ;
#21998 = VECTOR ( 'NONE', #14251, 1000.000000000000000 ) ;
#21999 = DIRECTION ( 'NONE',  ( 0.9995627462972741517, 0.000000000000000000, -0.02956883857460800707 ) ) ;
#22000 = EDGE_CURVE ( 'NONE', #26338, #3822, #24909, .T. ) ;
#22001 = CIRCLE ( 'NONE', #27614, 39.75000000000000000 ) ;
#22002 = FACE_BOUND ( 'NONE', #26165, .T. ) ;
#22003 = ADVANCED_FACE ( 'NONE', ( #2765 ), #14951, .T. ) ;
#22004 = VERTEX_POINT ( 'NONE', #20240 ) ;
#22005 = CARTESIAN_POINT ( 'NONE',  ( 19.73038513050000020, -98.60488090890000024, -0.3427724926369999925 ) ) ;
#22006 = ORIENTED_EDGE ( 'NONE', *, *, #16884, .F. ) ;
#22007 = CARTESIAN_POINT ( 'NONE',  ( -18.13877362739999910, -92.50000000000000000, -23.79298866759999598 ) ) ;
#22008 = CARTESIAN_POINT ( 'NONE',  ( 7.491375974803306192, -18.50000000000000000, -19.98345406245123357 ) ) ;
#22009 = ADVANCED_FACE ( 'NONE', ( #11622 ), #10292, .F. ) ;
#22010 = ORIENTED_EDGE ( 'NONE', *, *, #8866, .F. ) ;
#22011 = CARTESIAN_POINT ( 'NONE',  ( 28.89564796280000181, -73.80968813319999811, -26.61317346570000097 ) ) ;
#22012 = EDGE_CURVE ( 'NONE', #22934, #12631, #1265, .T. ) ;
#22013 = PRODUCT_DEFINITION_SHAPE ( 'NONE', 'NONE',  #28811 ) ;
#22014 = CARTESIAN_POINT ( 'NONE',  ( -14.10686381969999914, -92.91112761319999436, -23.69005823610000050 ) ) ;
#22015 = CARTESIAN_POINT ( 'NONE',  ( -11.16205616639999931, -94.83055275160000974, -21.09956017769999903 ) ) ;
#22016 = AXIS2_PLACEMENT_3D ( 'NONE', #15017, #17227, #7790 ) ;
#22017 = CARTESIAN_POINT ( 'NONE',  ( 1.312652382290000030, -94.71481430560001513, 24.32357623499999733 ) ) ;
#22018 = CARTESIAN_POINT ( 'NONE',  ( -20.20035178370000040, -94.89195255890000169, 12.35537463580000050 ) ) ;
#22019 = CARTESIAN_POINT ( 'NONE',  ( -29.68006920950033134, -92.66191076879675848, 7.024780034912508242 ) ) ;
#22020 = CARTESIAN_POINT ( 'NONE',  ( 11.88502995134358819, -99.07183862004048081, -15.04908790469807300 ) ) ;
#22021 = VERTEX_POINT ( 'NONE', #4801 ) ;
#22022 = DIRECTION ( 'NONE',  ( 1.000000000000000000, 0.000000000000000000, 0.000000000000000000 ) ) ;
#22023 = CARTESIAN_POINT ( 'NONE',  ( 23.66743934140000150, -49.85663837279999910, 0.8718307226189999648 ) ) ;
#22024 = CARTESIAN_POINT ( 'NONE',  ( 26.26491651929999804, -69.97113394359999461, 10.80126583880000091 ) ) ;
#22025 = CARTESIAN_POINT ( 'NONE',  ( 39.31656870519286429, -73.61799623138361426, 7.217717631475800033 ) ) ;
#22026 = VERTEX_POINT ( 'NONE', #2627 ) ;
#22027 = AXIS2_PLACEMENT_3D ( 'NONE', #3535, #25407, #5436 ) ;
#22028 = CARTESIAN_POINT ( 'NONE',  ( 0.000000000000000000, -108.5000000000000000, 0.000000000000000000 ) ) ;
#22029 = CARTESIAN_POINT ( 'NONE',  ( -15.01536691379999944, -92.56128749459999483, 24.94218803040000054 ) ) ;
#22030 = CARTESIAN_POINT ( 'NONE',  ( -20.53865360145708863, -92.95759695848158799, 17.41522175122109317 ) ) ;
#22031 = ORIENTED_EDGE ( 'NONE', *, *, #4275, .T. ) ;
#22032 = CARTESIAN_POINT ( 'NONE',  ( 8.831064126840001194, -94.59276292389999696, -22.09756266850000017 ) ) ;
#22033 = B_SPLINE_CURVE_WITH_KNOTS ( 'NONE', 3,
 ( #25666, #16913, #16344, #27722, #25252, #936, #5421, #7762, #7628, #16491, #25395, #5559 ),
 .UNSPECIFIED., .F., .F.,
 ( 4, 2, 1, 1, 2, 2, 4 ),
 ( 0.000000000000000000, 0.2500000000000220934, 0.3750000000000266454, 0.4375000000000288658, 0.4687500000000406342, 0.5000000000000524025, 1.000000000000000000 ),
 .UNSPECIFIED. ) ;
#22034 = CARTESIAN_POINT ( 'NONE',  ( 0.6195791821380000064, -100.2522625769999962, -17.00587765690000097 ) ) ;
#22035 = CARTESIAN_POINT ( 'NONE',  ( 23.80490084257870720, -74.13827441015507702, -31.01263663817537619 ) ) ;
#22036 = CARTESIAN_POINT ( 'NONE',  ( -12.07464971489999961, -68.03625990740000873, -24.51877662120000068 ) ) ;
#22037 = CARTESIAN_POINT ( 'NONE',  ( 22.00064631549999916, -63.98660223360000288, 11.26240653729999863 ) ) ;
#22038 = CARTESIAN_POINT ( 'NONE',  ( -10.91297770669999956, -42.23583340100000072, -21.40387953429999968 ) ) ;
#22039 = EDGE_LOOP ( 'NONE', ( #3877, #27356, #18090, #17158 ) ) ;
#22040 = CARTESIAN_POINT ( 'NONE',  ( 23.52622212079999997, -57.40875702419999982, -9.564509902230000193 ) ) ;
#22041 = CARTESIAN_POINT ( 'NONE',  ( -11.45174557199970522, -57.47815920938258216, 20.36405547779946090 ) ) ;
#22042 = AXIS2_PLACEMENT_3D ( 'NONE', #21629, #23669, #10518 ) ;
#22043 = EDGE_CURVE ( 'NONE', #21377, #26756, #14094, .T. ) ;
#22044 = ORIENTED_EDGE ( 'NONE', *, *, #5965, .T. ) ;
#22045 = CARTESIAN_POINT ( 'NONE',  ( 28.01404095332314625, -92.56492639277975343, 12.06120875835872042 ) ) ;
#22046 = CARTESIAN_POINT ( 'NONE',  ( 15.55009014945955315, -101.2404586421511965, 2.819223758050509954 ) ) ;
#22047 = CARTESIAN_POINT ( 'NONE',  ( -42.05565522495096076, -65.71171110559873796, -0.8680096503517884532 ) ) ;
#22048 = ORIENTED_EDGE ( 'NONE', *, *, #14459, .T. ) ;
#22049 = AXIS2_PLACEMENT_3D ( 'NONE', #13964, #11012, #19927 ) ;
#22050 = CARTESIAN_POINT ( 'NONE',  ( 8.472249407519999664, -94.22763312370000222, -22.74885336210000020 ) ) ;
#22051 = EDGE_CURVE ( 'NONE', #26855, #22409, #7514, .T. ) ;
#22052 = CARTESIAN_POINT ( 'NONE',  ( -0.8955242351559999925, -101.2530993039999885, -15.16897421750000063 ) ) ;
#22053 = DIRECTION ( 'NONE',  ( 0.000000000000000000, -1.000000000000000000, 0.000000000000000000 ) ) ;
#22054 = ORIENTED_EDGE ( 'NONE', *, *, #22754, .F. ) ;
#22055 = CARTESIAN_POINT ( 'NONE',  ( 27.19724826568005227, -72.11187000725442431, -11.65709713041382578 ) ) ;
#22056 = DIRECTION ( 'NONE',  ( 0.8775825618903722036, 0.000000000000000000, -0.4794255386042041156 ) ) ;
#22057 = EDGE_LOOP ( 'NONE', ( #4778, #16466, #4040, #12099 ) ) ;
#22058 = CARTESIAN_POINT ( 'NONE',  ( 8.125022609680000230, -36.17810633829999745, -21.26282345639999605 ) ) ;
#22059 = CARTESIAN_POINT ( 'NONE',  ( 26.58751350659999702, -92.65509162889999573, -7.785010380240000138 ) ) ;
#22060 = CARTESIAN_POINT ( 'NONE',  ( -1.108943289259999965, -101.2141467319999890, -15.20603369630000046 ) ) ;
#22061 = CIRCLE ( 'NONE', #9947, 18.64285714289999873 ) ;
#22062 = CARTESIAN_POINT ( 'NONE',  ( 23.09686208289999954, -18.86159979430000178, 1.490590284119999831 ) ) ;
#22063 = CARTESIAN_POINT ( 'NONE',  ( -43.29971333826889435, -63.05366661935828176, -0.03681143521561272558 ) ) ;
#22064 = AXIS2_PLACEMENT_3D ( 'NONE', #25867, #23816, #14771 ) ;
#22065 = CARTESIAN_POINT ( 'NONE',  ( -25.02601311510000315, -6.000000000000000000, -45.80980973070000317 ) ) ;
#22066 = DIRECTION ( 'NONE',  ( 0.000000000000000000, -1.000000000000000000, 0.000000000000000000 ) ) ;
#22067 = CARTESIAN_POINT ( 'NONE',  ( -7.476488366829999954, -100.9137139110000021, 13.72916197330000010 ) ) ;
#22068 = DIRECTION ( 'NONE',  ( 1.000000000000000000, 0.000000000000000000, 0.000000000000000000 ) ) ;
#22069 = CARTESIAN_POINT ( 'NONE',  ( -2.876553231629999985, -100.0000000000000000, -5.265495371340000119 ) ) ;
#22070 = CARTESIAN_POINT ( 'NONE',  ( 10.20110288159999890, -82.25000000000000000, 41.00000000000000000 ) ) ;
#22071 = DIRECTION ( 'NONE',  ( 1.000000000000000000, 0.000000000000000000, 0.000000000000000000 ) ) ;
#22072 = CIRCLE ( 'NONE', #16484, 7.249999999999999112 ) ;
#22073 = CARTESIAN_POINT ( 'NONE',  ( 24.76402736475559152, -93.25521310992057522, -13.40803308253799919 ) ) ;
#22074 = CARTESIAN_POINT ( 'NONE',  ( 20.81361611080448881, -94.60934249687453246, 13.89502885642193064 ) ) ;
#22075 = ORIENTED_EDGE ( 'NONE', *, *, #2333, .F. ) ;
#22076 = CARTESIAN_POINT ( 'NONE',  ( 8.697936417900001160, -18.86343732329999767, -19.75624699629999981 ) ) ;
#22077 = CIRCLE ( 'NONE', #23032, 10.00000000000000000 ) ;
#22078 = ADVANCED_FACE ( 'NONE', ( #10012, #16448 ), #27806, .F. ) ;
#22079 = CARTESIAN_POINT ( 'NONE',  ( 21.93668104079999992, -36.18298320059999895, -10.15270841880000141 ) ) ;
#22080 = EDGE_CURVE ( 'NONE', #18106, #28649, #8497, .T. ) ;
#22081 = CARTESIAN_POINT ( 'NONE',  ( -12.57842660070000029, -63.53964550370000097, 21.17786332950000272 ) ) ;
#22082 = CIRCLE ( 'NONE', #5333, 6.750000000000000000 ) ;
#22083 = CARTESIAN_POINT ( 'NONE',  ( 9.504972818060000606, -36.53320237809999327, -21.93059852529999887 ) ) ;
#22084 = DIRECTION ( 'NONE',  ( 0.03516156865429550388, 0.000000000000000000, 0.9993816408608722224 ) ) ;
#22085 = CARTESIAN_POINT ( 'NONE',  ( -19.49041480450000208, -52.62618816520016196, 12.93508487010000785 ) ) ;
#22086 = EDGE_CURVE ( 'NONE', #11556, #7139, #17908, .T. ) ;
#22087 = CARTESIAN_POINT ( 'NONE',  ( 16.16228525779999714, -100.3517545579999961, 4.402890113689999829 ) ) ;
#22088 = VERTEX_POINT ( 'NONE', #14677 ) ;
#22089 = CARTESIAN_POINT ( 'NONE',  ( 21.53806856769999811, -36.56992524600000394, -6.948750440460000455 ) ) ;
#22090 = CARTESIAN_POINT ( 'NONE',  ( -40.70731707320000226, -74.50000000000000000, -7.215414233289999757 ) ) ;
#22091 = ORIENTED_EDGE ( 'NONE', *, *, #6966, .F. ) ;
#22092 = DIRECTION ( 'NONE',  ( 0.000000000000000000, 1.000000000000000000, 0.000000000000000000 ) ) ;
#22093 = ORIENTED_EDGE ( 'NONE', *, *, #14502, .F. ) ;
#22094 = CARTESIAN_POINT ( 'NONE',  ( -14.24339565470000224, -80.06075086779999594, 36.77521474840000337 ) ) ;
#22095 = CARTESIAN_POINT ( 'NONE',  ( -9.824387680670000123, -18.50000000000000000, -22.02292149959999890 ) ) ;
#22096 = DIRECTION ( 'NONE',  ( 0.000000000000000000, 1.000000000000000000, 0.000000000000000000 ) ) ;
#22097 = CARTESIAN_POINT ( 'NONE',  ( -13.94900084250000027, -74.00000000000000000, 36.21247097760000599 ) ) ;
#22098 = CARTESIAN_POINT ( 'NONE',  ( -32.74642262723747876, -79.90759221510043631, -22.43672242427770769 ) ) ;
#22099 = CARTESIAN_POINT ( 'NONE',  ( -16.40265326879195129, -98.81923691017613010, 8.200441858953826824 ) ) ;
#22100 = EDGE_CURVE ( 'NONE', #6187, #21733, #8444, .T. ) ;
#22101 = VERTEX_POINT ( 'NONE', #15084 ) ;
#22102 = AXIS2_PLACEMENT_3D ( 'NONE', #24214, #17368, #10773 ) ;
#22103 = CARTESIAN_POINT ( 'NONE',  ( -15.38068916850000001, -101.6095197629999944, 4.516181925269999731 ) ) ;
#22104 = CARTESIAN_POINT ( 'NONE',  ( -29.17304402409999753, -10.50000000000000000, -53.40089889099999709 ) ) ;
#22105 = CARTESIAN_POINT ( 'NONE',  ( -12.50278151429999873, -101.3256027139999986, -9.834025437379999346 ) ) ;
#22106 = CARTESIAN_POINT ( 'NONE',  ( -7.173755656178061102, -73.51389412123563716, 38.94432755061352225 ) ) ;
#22107 = CARTESIAN_POINT ( 'NONE',  ( -40.70731707320000226, -74.50000000000000000, -7.215414233289999757 ) ) ;
#22108 = VERTEX_POINT ( 'NONE', #1859 ) ;
#22109 = CARTESIAN_POINT ( 'NONE',  ( 0.000000000000000000, -23.30310889129999907, 0.000000000000000000 ) ) ;
#22110 = CARTESIAN_POINT ( 'NONE',  ( -32.17538889770000310, -74.02659082439998883, -21.91468059299999993 ) ) ;
#22111 = CARTESIAN_POINT ( 'NONE',  ( -22.71848792900000191, -80.00000000000000000, -32.61798286559999838 ) ) ;
#22112 = ORIENTED_EDGE ( 'NONE', *, *, #26572, .F. ) ;
#22113 = ADVANCED_FACE ( 'NONE', ( #1714 ), #2893, .T. ) ;
#22114 = B_SPLINE_CURVE_WITH_KNOTS ( 'NONE', 3,
 ( #23852, #10988, #26332, #15221, #1717, #12756, #1863, #21667, #19471, #19620, #4176, #10702 ),
 .UNSPECIFIED., .F., .F.,
 ( 4, 2, 2, 2, 2, 4 ),
 ( 0.000000000000000000, 0.2500000000000487943, 0.3750000000000819900, 0.4375000000000869860, 0.5000000000000920375, 1.000000000000000000 ),
 .UNSPECIFIED. ) ;
#22115 = CARTESIAN_POINT ( 'NONE',  ( 7.105427357599999217E-15, -69.00000000000000000, -40.00000000000000000 ) ) ;
#22116 = CARTESIAN_POINT ( 'NONE',  ( -5.890278778139999893, -101.2306310700000012, 15.10563525420000097 ) ) ;
#22117 = CARTESIAN_POINT ( 'NONE',  ( -0.5459402786740000790, -58.79569603810000444, -23.43709083150000083 ) ) ;
#22118 = EDGE_LOOP ( 'NONE', ( #10859, #68, #1291, #7981 ) ) ;
#22119 = CARTESIAN_POINT ( 'NONE',  ( 0.000000000000000000, -82.25000000000000000, 40.00000000000000000 ) ) ;
#22120 = CARTESIAN_POINT ( 'NONE',  ( 41.00000000000000000, -82.25000000000000000, 10.20110288159999890 ) ) ;
#22121 = ORIENTED_EDGE ( 'NONE', *, *, #20134, .T. ) ;
#22122 = CARTESIAN_POINT ( 'NONE',  ( 23.93718440349999810, -92.97899053829999616, 11.95681231160000024 ) ) ;
#22123 = CARTESIAN_POINT ( 'NONE',  ( -14.94261203119999948, -100.8733967390000004, 4.897670397449999768 ) ) ;
#22124 = ORIENTED_EDGE ( 'NONE', *, *, #19792, .T. ) ;
#22125 = DIRECTION ( 'NONE',  ( 1.000000000000000000, 0.000000000000000000, 0.000000000000000000 ) ) ;
#22126 = CARTESIAN_POINT ( 'NONE',  ( -22.09862634569999784, -80.12422039649999306, -32.50322686590000387 ) ) ;
#22127 = ORIENTED_EDGE ( 'NONE', *, *, #16821, .F. ) ;
#22128 = DIRECTION ( 'NONE',  ( -0.3687499999999814260, 0.000000000000000000, 0.9295286103719527793 ) ) ;
#22129 = CARTESIAN_POINT ( 'NONE',  ( -21.81061053790000059, -92.49999926799999628, -19.59831469680000282 ) ) ;
#22130 = CARTESIAN_POINT ( 'NONE',  ( 0.000000000000000000, -2.000000000000000000, 0.000000000000000000 ) ) ;
#22131 = EDGE_LOOP ( 'NONE', ( #852, #25514, #12038, #7844 ) ) ;
#22132 = CARTESIAN_POINT ( 'NONE',  ( -41.75000000000000000, -63.30468293320000583, -1.587713240270000048 ) ) ;
#22133 = CARTESIAN_POINT ( 'NONE',  ( 12.68316649459999823, -100.8772072149999985, -9.423397405859999409 ) ) ;
#22134 = FACE_OUTER_BOUND ( 'NONE', #12843, .T. ) ;
#22135 = EDGE_CURVE ( 'NONE', #6364, #17271, #11705, .T. ) ;
#22136 = DIRECTION ( 'NONE',  ( 0.000000000000000000, 1.000000000000000000, 0.000000000000000000 ) ) ;
#22137 = TOROIDAL_SURFACE ( 'NONE', #17013, 0.5000000000000000000, 0.5000000000000000000 ) ;
#22138 = LINE ( 'NONE', #28667, #13404 ) ;
#22139 = CARTESIAN_POINT ( 'NONE',  ( 10.16635616659465136, -72.73332183106052184, -26.84588916250481105 ) ) ;
#22140 = DIRECTION ( 'NONE',  ( 0.9999792992113792911, 0.000000000000000000, 0.006434372441722326086 ) ) ;
#22141 = ORIENTED_EDGE ( 'NONE', *, *, #8750, .T. ) ;
#22142 = CARTESIAN_POINT ( 'NONE',  ( 9.438993784957457223, -64.72767717259272047, -23.93801147444352395 ) ) ;
#22143 = CARTESIAN_POINT ( 'NONE',  ( 20.33037861331306217, -73.74757277672107136, -31.96328472817131683 ) ) ;
#22144 = CARTESIAN_POINT ( 'NONE',  ( -24.15301378228902252, -92.58608763742770975, -18.62476874987404329 ) ) ;
#22145 = FACE_OUTER_BOUND ( 'NONE', #12625, .T. ) ;
#22146 = FACE_OUTER_BOUND ( 'NONE', #22974, .T. ) ;
#22147 = AXIS2_PLACEMENT_3D ( 'NONE', #13456, #24536, #22071 ) ;
#22148 = CARTESIAN_POINT ( 'NONE',  ( -15.42363691649999957, -45.73899999920000425, 22.84488648889999851 ) ) ;
#22149 = FACE_OUTER_BOUND ( 'NONE', #14052, .T. ) ;
#22150 = ORIENTED_EDGE ( 'NONE', *, *, #19776, .F. ) ;
#22151 = DIRECTION ( 'NONE',  ( 0.000000000000000000, 1.000000000000000000, 0.000000000000000000 ) ) ;
#22152 = CARTESIAN_POINT ( 'NONE',  ( 20.62756379660000050, -97.01506440939999720, -2.488770823180000313 ) ) ;
#22153 = VERTEX_POINT ( 'NONE', #3610 ) ;
#22154 = DIRECTION ( 'NONE',  ( 0.000000000000000000, 1.000000000000000000, 0.000000000000000000 ) ) ;
#22155 = CARTESIAN_POINT ( 'NONE',  ( -43.20000000000000284, -65.14977478849999670, -0.1732050807570000017 ) ) ;
#22156 = ORIENTED_EDGE ( 'NONE', *, *, #3977, .F. ) ;
#22157 = CARTESIAN_POINT ( 'NONE',  ( 15.91666809940000071, -101.0685849509999912, 2.371725914449999806 ) ) ;
#22158 = EDGE_LOOP ( 'NONE', ( #6100, #8437, #6460 ) ) ;
#22159 = CARTESIAN_POINT ( 'NONE',  ( 22.29272167938353633, -65.04696937986301464, 11.61829170019522017 ) ) ;
#22160 = DIRECTION ( 'NONE',  ( -1.186916062510446772E-15, 0.000000000000000000, 1.000000000000000000 ) ) ;
#22161 = FACE_OUTER_BOUND ( 'NONE', #15506, .T. ) ;
#22162 = CARTESIAN_POINT ( 'NONE',  ( -29.69325694440044572, -92.68577957612751561, 6.968726778918060027 ) ) ;
#22163 = CARTESIAN_POINT ( 'NONE',  ( 47.19378694702872679, -79.33057058301108100, -1.140171656175917647 ) ) ;
#22164 = ORIENTED_EDGE ( 'NONE', *, *, #6470, .F. ) ;
#22165 = CARTESIAN_POINT ( 'NONE',  ( 11.32290720589999822, -93.36531860510000058, -23.59732887200000206 ) ) ;
#22166 = CARTESIAN_POINT ( 'NONE',  ( 24.76695232029999971, -34.59963798460000106, 1.400254471660000055 ) ) ;
#22167 = CARTESIAN_POINT ( 'NONE',  ( -14.25482831575127030, -80.47374551902997553, 36.57016602121424143 ) ) ;
#22168 = ADVANCED_FACE ( 'NONE', ( #10553 ), #19468, .F. ) ;
#22169 = CARTESIAN_POINT ( 'NONE',  ( -13.26851675973651545, -92.83160374581382257, 27.46263779841126507 ) ) ;
#22170 = EDGE_LOOP ( 'NONE', ( #6240, #19550, #1556, #817 ) ) ;
#22171 = CARTESIAN_POINT ( 'NONE',  ( -4.123059632000000363, -17.00000000000000000, -7.547210032260000645 ) ) ;
#22172 = CARTESIAN_POINT ( 'NONE',  ( -16.67583898440000212, -92.84059452359998943, 21.54669423090000180 ) ) ;
#22173 = CARTESIAN_POINT ( 'NONE',  ( -6.569460039029999976, -101.6484611540000031, 14.03895276709999962 ) ) ;
#22174 = ORIENTED_EDGE ( 'NONE', *, *, #669, .T. ) ;
#22175 = EDGE_CURVE ( 'NONE', #6793, #19902, #22457, .T. ) ;
#22176 = DIRECTION ( 'NONE',  ( 0.000000000000000000, -1.000000000000000000, 0.000000000000000000 ) ) ;
#22177 = CARTESIAN_POINT ( 'NONE',  ( 0.9829826817099999170, -100.1512121650000040, -16.61044266980000117 ) ) ;
#22178 = DIRECTION ( 'NONE',  ( 1.000000000000000000, 0.000000000000000000, 0.000000000000000000 ) ) ;
#22179 = CARTESIAN_POINT ( 'NONE',  ( 15.80445266879999799, -101.5026188610000020, 2.634903237490000105 ) ) ;
#22180 = EDGE_CURVE ( 'NONE', #11057, #11437, #9221, .T. ) ;
#22181 = CARTESIAN_POINT ( 'NONE',  ( -12.04115840220000067, -49.87553805839999654, -19.70837320809999937 ) ) ;
#22182 = EDGE_CURVE ( 'NONE', #26536, #20079, #6765, .T. ) ;
#22183 = CARTESIAN_POINT ( 'NONE',  ( 22.95932757850121675, -57.43039251884066942, -9.307781678040345952 ) ) ;
#22184 = ORIENTED_EDGE ( 'NONE', *, *, #27969, .F. ) ;
#22185 = CARTESIAN_POINT ( 'NONE',  ( -2.987826573587363477, -18.62337006874621181, -24.35058480141394099 ) ) ;
#22186 = FACE_OUTER_BOUND ( 'NONE', #18501, .T. ) ;
#22187 = CARTESIAN_POINT ( 'NONE',  ( -2.986711995579999890, -94.79581469870001342, 23.48470869699999852 ) ) ;
#22188 = EDGE_LOOP ( 'NONE', ( #28401, #14323, #13769, #9636 ) ) ;
#22189 = CARTESIAN_POINT ( 'NONE',  ( 20.48885040240000066, -93.05538536990000864, 16.53376986659999659 ) ) ;
#22190 = CARTESIAN_POINT ( 'NONE',  ( 22.71753027169577521, -19.47230399480618246, 1.004254908788112965 ) ) ;
#22191 = CARTESIAN_POINT ( 'NONE',  ( -7.155293904009999650, -101.2927714249999980, 14.37234474879999979 ) ) ;
#22192 = EDGE_LOOP ( 'NONE', ( #24388, #9734, #17804, #26274, #25232, #14406 ) ) ;
#22193 = CARTESIAN_POINT ( 'NONE',  ( -16.49390888960000368, -80.00000000000000000, 44.28897684009999836 ) ) ;
#22194 = CARTESIAN_POINT ( 'NONE',  ( -12.91282149864488460, -100.3796496173521007, -11.05327605674254166 ) ) ;
#22195 = ORIENTED_EDGE ( 'NONE', *, *, #19792, .F. ) ;
#22196 = CARTESIAN_POINT ( 'NONE',  ( 7.642421028099999347, -37.32903481230000153, -21.50491099470000123 ) ) ;
#22197 = CARTESIAN_POINT ( 'NONE',  ( 26.20717514349999888, -93.01085527740001169, -7.939310658160000145 ) ) ;
#22198 = CARTESIAN_POINT ( 'NONE',  ( 9.119802927630001221, -98.28914429610000525, 16.69368728350000097 ) ) ;
#22199 = CARTESIAN_POINT ( 'NONE',  ( 22.02376134869999902, -19.15747282889999781, -0.1818244595100000083 ) ) ;
#22200 = CARTESIAN_POINT ( 'NONE',  ( -25.37284092810000047, -93.00000000000000000, 2.543411731580000001 ) ) ;
#22201 = CARTESIAN_POINT ( 'NONE',  ( -20.33391829737038492, -92.64884742716812127, -22.73286488652288639 ) ) ;
#22202 = EDGE_LOOP ( 'NONE', ( #21915, #25687 ) ) ;
#22203 = CARTESIAN_POINT ( 'NONE',  ( 11.34527656030000031, -101.0555477039999914, -10.55639998680000069 ) ) ;
#22204 = DIRECTION ( 'NONE',  ( 0.4794255386042000078, 0.000000000000000000, 0.8775825618903743131 ) ) ;
#22205 = CARTESIAN_POINT ( 'NONE',  ( 16.32839208820038834, -94.64093351176255453, 17.22545126736804022 ) ) ;
#22206 = EDGE_CURVE ( 'NONE', #19169, #12443, #18590, .T. ) ;
#22207 = AXIS2_PLACEMENT_3D ( 'NONE', #7786, #21052, #14047 ) ;
#22208 = DIRECTION ( 'NONE',  ( 1.000000000000000000, 0.000000000000000000, 0.000000000000000000 ) ) ;
#22209 = CARTESIAN_POINT ( 'NONE',  ( -12.68184371739999960, -66.93519943800001215, -22.70010485369999742 ) ) ;
#22210 = CARTESIAN_POINT ( 'NONE',  ( -30.34790777679999962, -111.0000000000000000, 3.042119914239999723 ) ) ;
#22211 = CARTESIAN_POINT ( 'NONE',  ( 27.44308006103930708, -93.08694455168847526, 9.636015041101046563 ) ) ;
#22212 = ORIENTED_EDGE ( 'NONE', *, *, #16593, .F. ) ;
#22213 = ADVANCED_FACE ( 'NONE', ( #6660 ), #12214, .T. ) ;
#22214 = CARTESIAN_POINT ( 'NONE',  ( -10.17458377400000025, -18.50000000000000000, -22.50859265919999785 ) ) ;
#22215 = CARTESIAN_POINT ( 'NONE',  ( 7.799868133589999530, -101.0912156119999992, 13.74000810979999798 ) ) ;
#22216 = AXIS2_PLACEMENT_3D ( 'NONE', #7127, #20228, #17904 ) ;
#22217 = PRESENTATION_LAYER_ASSIGNMENT (  '', '', ( #8689 ) ) ;
#22218 = CARTESIAN_POINT ( 'NONE',  ( -14.55867151890000066, -64.24504444460001196, 22.15151624130000130 ) ) ;
#22219 = CARTESIAN_POINT ( 'NONE',  ( 0.000000000000000000, -72.82938648530000592, 0.000000000000000000 ) ) ;
#22220 = CARTESIAN_POINT ( 'NONE',  ( -24.70281971250000197, -94.64125147560000073, -3.583037810470000029 ) ) ;
#22221 = CARTESIAN_POINT ( 'NONE',  ( -20.53532388389999852, -56.19735282230000450, 14.83773643259999986 ) ) ;
#22222 = ORIENTED_EDGE ( 'NONE', *, *, #17062, .T. ) ;
#22223 = DIRECTION ( 'NONE',  ( 0.000000000000000000, 0.000000000000000000, -1.000000000000000000 ) ) ;
#22224 = CARTESIAN_POINT ( 'NONE',  ( 29.28697822896142711, -74.32957653769940976, -26.08612603725635992 ) ) ;
#22225 = DIRECTION ( 'NONE',  ( 1.000000000000000000, 0.000000000000000000, 0.000000000000000000 ) ) ;
#22226 = ORIENTED_EDGE ( 'NONE', *, *, #6311, .F. ) ;
#22227 = CYLINDRICAL_SURFACE ( 'NONE', #4742, 2.999999999999998668 ) ;
#22228 = VERTEX_POINT ( 'NONE', #25843 ) ;
#22229 = CARTESIAN_POINT ( 'NONE',  ( -12.03978574509999966, -15.00000000000000000, -22.03867997850000293 ) ) ;
#22230 = CARTESIAN_POINT ( 'NONE',  ( 19.36777041659999554, -19.46363745430000236, 10.50577160559999967 ) ) ;
#22231 = EDGE_CURVE ( 'NONE', #9894, #18698, #22690, .T. ) ;
#22232 = LINE ( 'NONE', #10975, #27530 ) ;
#22233 = CARTESIAN_POINT ( 'NONE',  ( 24.85760066650000155, -93.16461275549998788, -13.76036209870000171 ) ) ;
#22234 = EDGE_CURVE ( 'NONE', #2616, #2738, #6118, .T. ) ;
#22235 = AXIS2_PLACEMENT_3D ( 'NONE', #5526, #25907, #3623 ) ;
#22236 = CARTESIAN_POINT ( 'NONE',  ( 21.31224117700000065, -62.89055566329999891, 11.58369406600000140 ) ) ;
#22237 = CARTESIAN_POINT ( 'NONE',  ( 19.57843399940000140, -94.59276292389999696, 13.52682119470000011 ) ) ;
#22238 = CARTESIAN_POINT ( 'NONE',  ( 14.11489916659999899, -97.73638926259998527, -14.10864689489999968 ) ) ;
#22239 = ORIENTED_EDGE ( 'NONE', *, *, #13271, .T. ) ;
#22240 = CARTESIAN_POINT ( 'NONE',  ( 40.00000000000000000, -79.00000000000000000, 4.898587196589999938E-15 ) ) ;
#22241 = CARTESIAN_POINT ( 'NONE',  ( 7.678730999230412912, -101.6404041080485001, 14.04396369532980771 ) ) ;
#22242 = CARTESIAN_POINT ( 'NONE',  ( 21.42283722234454046, -19.48260761094563520, 9.476082331836883199 ) ) ;
#22243 = CARTESIAN_POINT ( 'NONE',  ( -40.34091732139999920, -74.29300278850000439, -7.252014196680000246 ) ) ;
#22244 = EDGE_LOOP ( 'NONE', ( #12638, #20311, #14653, #11245 ) ) ;
#22245 = EDGE_CURVE ( 'NONE', #519, #618, #24764, .T. ) ;
#22246 = CARTESIAN_POINT ( 'NONE',  ( 26.65335633700317430, -92.66455718076046821, -14.82729397443163499 ) ) ;
#22247 = VECTOR ( 'NONE', #18206, 1000.000000000000114 ) ;
#22248 = CARTESIAN_POINT ( 'NONE',  ( -32.52011734909999774, -74.20254482470001278, -21.99161358219999940 ) ) ;
#22249 = ORIENTED_EDGE ( 'NONE', *, *, #4942, .T. ) ;
#22250 = CARTESIAN_POINT ( 'NONE',  ( 0.000000000000000000, -39.32601556110000018, 0.000000000000000000 ) ) ;
#22251 = DIRECTION ( 'NONE',  ( 0.000000000000000000, 1.000000000000000000, 0.000000000000000000 ) ) ;
#22252 = DIRECTION ( 'NONE',  ( 1.000000000000000000, 0.000000000000000000, 0.000000000000000000 ) ) ;
#22253 = CARTESIAN_POINT ( 'NONE',  ( 11.95338359237086223, -101.3051320416555825, -10.44690246017028912 ) ) ;
#22254 = VERTEX_POINT ( 'NONE', #22988 ) ;
#22255 = AXIS2_PLACEMENT_3D ( 'NONE', #13227, #15854, #19786 ) ;
#22256 = DIRECTION ( 'NONE',  ( 0.000000000000000000, 1.000000000000000000, 0.000000000000000000 ) ) ;
#22257 = EDGE_LOOP ( 'NONE', ( #3935, #6544, #21590, #2440 ) ) ;
#22258 = CARTESIAN_POINT ( 'NONE',  ( -23.10281210965324306, -72.22683319543493496, 16.53369850595768753 ) ) ;
#22259 = CARTESIAN_POINT ( 'NONE',  ( 21.31694387499999976, -94.06807427549999545, 13.63926651669999934 ) ) ;
#22260 = DIRECTION ( 'NONE',  ( 0.000000000000000000, 1.000000000000000000, 0.000000000000000000 ) ) ;
#22261 = ORIENTED_EDGE ( 'NONE', *, *, #26819, .F. ) ;
#22262 = CARTESIAN_POINT ( 'NONE',  ( -36.59277592640000165, -77.00000000000000000, -27.40038777100000189 ) ) ;
#22263 = CARTESIAN_POINT ( 'NONE',  ( -21.85457011909999991, -79.72846757719999289, -32.66023316209999905 ) ) ;
#22264 = CARTESIAN_POINT ( 'NONE',  ( 20.64374438969968040, -57.47815920198944895, 10.93952083479982740 ) ) ;
#22265 = CARTESIAN_POINT ( 'NONE',  ( 8.702650270779999531, -36.72157724030000026, -21.61812616270000120 ) ) ;
#22266 = CARTESIAN_POINT ( 'NONE',  ( -14.06008659669999972, -93.67384740789999853, -21.43629181160000385 ) ) ;
#22267 = DIRECTION ( 'NONE',  ( 1.000000000000000000, 0.000000000000000000, 0.000000000000000000 ) ) ;
#22268 = VERTEX_POINT ( 'NONE', #715 ) ;
#22269 = CARTESIAN_POINT ( 'NONE',  ( -1.283023294879999998, -101.3150694429999987, -16.20107482390000087 ) ) ;
#22270 = EDGE_CURVE ( 'NONE', #21377, #19473, #12969, .T. ) ;
#22271 = CARTESIAN_POINT ( 'NONE',  ( -2.785765053610000042, -64.19655116939999573, -26.34478359919999946 ) ) ;
#22272 = CARTESIAN_POINT ( 'NONE',  ( -39.54176628510000313, -73.97626148509999666, 7.314390784519999578 ) ) ;
#22273 = CARTESIAN_POINT ( 'NONE',  ( -22.07235328799999863, -74.12815218200000800, -32.48152077880000377 ) ) ;
#22274 = CARTESIAN_POINT ( 'NONE',  ( -5.658845926663969017, -98.25430909850952332, -19.43178140796045028 ) ) ;
#22275 = CARTESIAN_POINT ( 'NONE',  ( -13.83118819819999956, -111.0000000000000000, 21.42307711379999802 ) ) ;
#22276 = CARTESIAN_POINT ( 'NONE',  ( -7.307162633536313123, -73.99981221269277398, 39.53460932750543577 ) ) ;
#22277 = CARTESIAN_POINT ( 'NONE',  ( 7.215414233289999757, -74.50000000000000000, -40.70731707320000226 ) ) ;
#22278 = ORIENTED_EDGE ( 'NONE', *, *, #10054, .T. ) ;
#22279 = CIRCLE ( 'NONE', #13905, 20.64285714289999873 ) ;
#22280 = DIRECTION ( 'NONE',  ( 0.000000000000000000, 1.000000000000000000, 0.000000000000000000 ) ) ;
#22281 = CIRCLE ( 'NONE', #25561, 0.5000000000000001110 ) ;
#22282 = CIRCLE ( 'NONE', #26001, 0.9999999999999980016 ) ;
#22283 = CARTESIAN_POINT ( 'NONE',  ( 20.35242036615802519, -74.00000000000477485, -32.70839735534965342 ) ) ;
#22284 = CARTESIAN_POINT ( 'NONE',  ( 2.486899575159999765E-14, -80.50000000000000000, 7.105427357599999217E-15 ) ) ;
#22285 = CARTESIAN_POINT ( 'NONE',  ( -4.794255386040000566, -108.5000000000000000, -8.775825618900000791 ) ) ;
#22286 = CARTESIAN_POINT ( 'NONE',  ( 0.000000000000000000, -82.25000000000000000, 0.000000000000000000 ) ) ;
#22287 = CARTESIAN_POINT ( 'NONE',  ( -26.69293917519999937, -26.90310889129999694, -48.86109741659999628 ) ) ;
#22288 = DIRECTION ( 'NONE',  ( 1.000000000000000000, 0.000000000000000000, 0.000000000000000000 ) ) ;
#22289 = EDGE_LOOP ( 'NONE', ( #7581, #2427, #1802, #14912 ) ) ;
#22290 = ADVANCED_FACE ( 'NONE', ( #11891 ), #5484, .T. ) ;
#22291 = CARTESIAN_POINT ( 'NONE',  ( 26.69293917519999937, -19.70310889130000120, 48.86109741659999628 ) ) ;
#22292 = CARTESIAN_POINT ( 'NONE',  ( 17.89054857160000367, -99.82967635330000178, 1.194493289920000034 ) ) ;
#22294 = EDGE_LOOP ( 'NONE', ( #1220, #6096, #1513, #14696 ) ) ;
#22293 = VECTOR ( 'NONE', #14739, 999.9999999999998863 ) ;
#22295 = DIRECTION ( 'NONE',  ( 0.000000000000000000, 1.000000000000000000, 0.000000000000000000 ) ) ;
#22296 = CARTESIAN_POINT ( 'NONE',  ( -21.89190459030000113, -74.01117791779999777, -32.13651045809999829 ) ) ;
#22297 = ORIENTED_EDGE ( 'NONE', *, *, #21568, .F. ) ;
#22298 = CARTESIAN_POINT ( 'NONE',  ( 14.96040621690000094, -95.42941506580001487, 17.19850698980000203 ) ) ;
#22299 = AXIS2_PLACEMENT_3D ( 'NONE', #21090, #13168, #1690 ) ;
#22300 = CIRCLE ( 'NONE', #28341, 61.35000000000000142 ) ;
#22301 = AXIS2_PLACEMENT_3D ( 'NONE', #26335, #6816, #22252 ) ;
#22302 = CARTESIAN_POINT ( 'NONE',  ( 22.17953377930000158, -65.07443093669999712, 11.85657293289999892 ) ) ;
#22303 = CARTESIAN_POINT ( 'NONE',  ( 8.514116711873594312, -94.35876167791963098, -23.96130013197857878 ) ) ;
#22304 = CARTESIAN_POINT ( 'NONE',  ( -23.50862727400000196, -94.59276292389999696, -3.692480628369999796 ) ) ;
#22305 = CARTESIAN_POINT ( 'NONE',  ( 29.70835240799999966, -91.50000000000000000, 6.903897247299999762 ) ) ;
#22306 = CARTESIAN_POINT ( 'NONE',  ( -10.78318709900000094, -19.46528100780000159, -19.40120878459999787 ) ) ;
#22307 = CARTESIAN_POINT ( 'NONE',  ( 47.19667865516128558, -79.32224956671613825, -1.110774814387318177 ) ) ;
#22308 = ORIENTED_EDGE ( 'NONE', *, *, #23375, .F. ) ;
#22309 = CARTESIAN_POINT ( 'NONE',  ( 1.065814103639999922E-14, -18.50000000000000000, 2.664535259099999805E-15 ) ) ;
#22310 = EDGE_CURVE ( 'NONE', #1175, #3141, #10753, .T. ) ;
#22311 = CARTESIAN_POINT ( 'NONE',  ( -42.25000000000000000, -63.00000000000000000, -0.7216878364880000563 ) ) ;
#22312 = CARTESIAN_POINT ( 'NONE',  ( -32.63800352850000053, -74.22019266179999875, -21.66201587429999975 ) ) ;
#22313 = ORIENTED_EDGE ( 'NONE', *, *, #3572, .T. ) ;
#22314 = DIRECTION ( 'NONE',  ( 0.000000000000000000, 1.000000000000000000, 0.000000000000000000 ) ) ;
#22315 = CARTESIAN_POINT ( 'NONE',  ( 7.400235822239999983, -63.19606248799999548, -23.19730672580000075 ) ) ;
#22316 = VERTEX_POINT ( 'NONE', #26548 ) ;
#22317 = ADVANCED_FACE ( 'NONE', ( #12828 ), #27816, .T. ) ;
#22318 = CARTESIAN_POINT ( 'NONE',  ( 27.20825738430000129, -68.79186515250000866, 1.585888911440000104 ) ) ;
#22319 = CARTESIAN_POINT ( 'NONE',  ( 0.7684516987970000379, -100.0496341300000154, -16.89528639299999924 ) ) ;
#22320 = CARTESIAN_POINT ( 'NONE',  ( 20.86991714526983088, -74.00000000000196110, -32.73119363184984110 ) ) ;
#22321 = CARTESIAN_POINT ( 'NONE',  ( -20.08103059739376306, -57.43018248828013128, 14.46712379734940335 ) ) ;
#22322 = CARTESIAN_POINT ( 'NONE',  ( 0.000000000000000000, -14.30000000000000071, 0.000000000000000000 ) ) ;
#22323 = CIRCLE ( 'NONE', #6020, 11.00000000000000000 ) ;
#22324 = VECTOR ( 'NONE', #24758, 1000.000000000000000 ) ;
#22325 = CARTESIAN_POINT ( 'NONE',  ( 22.71963930830125022, -57.44066855174124697, -9.099147364980348485 ) ) ;
#22326 = CARTESIAN_POINT ( 'NONE',  ( -18.99756495820000168, -93.00000000000000000, -23.62136188200000220 ) ) ;
#22327 = B_SPLINE_CURVE_WITH_KNOTS ( 'NONE', 5,
 ( #20032, #16092, #11719, #20635, #24410, #97 ),
 .UNSPECIFIED., .F., .F.,
 ( 6, 6 ),
 ( 0.000000000000000000, 1.000000000000000000 ),
 .UNSPECIFIED. ) ;
#22328 = VERTEX_POINT ( 'NONE', #7035 ) ;
#22329 = B_SPLINE_CURVE_WITH_KNOTS ( 'NONE', 5,
 ( #27260, #9611, #2643, #13840, #4957, #20991, #11491, #23036, #25071 ),
 .UNSPECIFIED., .F., .F.,
 ( 6, 3, 6 ),
 ( 0.000000000000000000, 1.237573681350000010, 1.566718891480000098 ),
 .UNSPECIFIED. ) ;
#22330 = ADVANCED_FACE ( 'NONE', ( #13419 ), #22433, .F. ) ;
#22331 = CARTESIAN_POINT ( 'NONE',  ( 28.49579638229387513, -92.86276748840948869, 10.87457464806996299 ) ) ;
#22332 = DIRECTION ( 'NONE',  ( 0.4794255386042041156, 0.000000000000000000, 0.8775825618903722036 ) ) ;
#22333 = CARTESIAN_POINT ( 'NONE',  ( 0.000000000000000000, -28.10000000000000142, 0.000000000000000000 ) ) ;
#22334 = VERTEX_POINT ( 'NONE', #18246 ) ;
#22335 = CARTESIAN_POINT ( 'NONE',  ( 23.69288052678082934, -92.66191076872320309, -19.20680752137960567 ) ) ;
#22336 = CARTESIAN_POINT ( 'NONE',  ( 24.54087331869999744, -92.99999854809999533, 14.48417091049999961 ) ) ;
#22337 = DIRECTION ( 'NONE',  ( 0.000000000000000000, -1.000000000000000000, 0.000000000000000000 ) ) ;
#22338 = CARTESIAN_POINT ( 'NONE',  ( -7.429654490199999017, -101.3090757639999993, 14.46660187589999857 ) ) ;
#22339 = ORIENTED_EDGE ( 'NONE', *, *, #14258, .F. ) ;
#22340 = CARTESIAN_POINT ( 'NONE',  ( 27.06175282578147190, -72.22552502750772874, -11.46356654631565597 ) ) ;
#22341 = CARTESIAN_POINT ( 'NONE',  ( -12.45048480342227037, -101.4304678898350005, -10.31532340321227359 ) ) ;
#22342 = VERTEX_POINT ( 'NONE', #6882 ) ;
#22343 = CARTESIAN_POINT ( 'NONE',  ( 7.836612423160000063, -37.59151559440000057, -21.54406958319999887 ) ) ;
#22344 = EDGE_CURVE ( 'NONE', #28514, #15872, #9544, .T. ) ;
#22345 = AXIS2_PLACEMENT_3D ( 'NONE', #414, #15669, #4467 ) ;
#22346 = CARTESIAN_POINT ( 'NONE',  ( 9.024081099289999131, -19.49999992740000110, -18.94592230980000380 ) ) ;
#22347 = EDGE_LOOP ( 'NONE', ( #5868, #13698, #19248, #470 ) ) ;
#22348 = CIRCLE ( 'NONE', #18142, 0.5000000000000004441 ) ;
#22349 = FACE_OUTER_BOUND ( 'NONE', #12427, .T. ) ;
#22350 = CARTESIAN_POINT ( 'NONE',  ( -21.30003612899999865, -91.50000000000000000, -21.83021898440000186 ) ) ;
#22351 = CARTESIAN_POINT ( 'NONE',  ( -5.605778865269999578, -95.75647260680000272, -21.78235593370000345 ) ) ;
#22352 = CARTESIAN_POINT ( 'NONE',  ( -20.85062936798085786, -92.82334897400905049, -22.25985776189306620 ) ) ;
#22353 = CARTESIAN_POINT ( 'NONE',  ( 11.23915397940000105, -100.8869817940000075, -10.91500585829999892 ) ) ;
#22354 = DIRECTION ( 'NONE',  ( 0.000000000000000000, -1.000000000000000000, 0.000000000000000000 ) ) ;
#22355 = CARTESIAN_POINT ( 'NONE',  ( -15.46577867176106302, -100.1470170704337050, -8.781364183522299527 ) ) ;
#22356 = CARTESIAN_POINT ( 'NONE',  ( 7.066909182079999852, -57.47855601759999900, -22.26662627820000040 ) ) ;
#22357 = FACE_OUTER_BOUND ( 'NONE', #11590, .T. ) ;
#22358 = CARTESIAN_POINT ( 'NONE',  ( -13.05632738709999963, -66.36684605099999601, -22.18172164889999820 ) ) ;
#22359 = CARTESIAN_POINT ( 'NONE',  ( -38.31563671849563235, -65.09473604208548636, -2.838061730473900202 ) ) ;
#22360 = DIRECTION ( 'NONE',  ( 1.000000000000000000, 0.000000000000000000, 0.000000000000000000 ) ) ;
#22361 = FACE_OUTER_BOUND ( 'NONE', #18016, .T. ) ;
#22362 = ORIENTED_EDGE ( 'NONE', *, *, #16459, .F. ) ;
#22363 = DIRECTION ( 'NONE',  ( 1.000000000000000000, 0.000000000000000000, 0.000000000000000000 ) ) ;
#22364 = CARTESIAN_POINT ( 'NONE',  ( 7.995260568349999986, -101.2398794199999941, 13.96161139179999999 ) ) ;
#22365 = TOROIDAL_SURFACE ( 'NONE', #6051, 7.750000000000000000, 0.5000000000000000000 ) ;
#22366 = ORIENTED_EDGE ( 'NONE', *, *, #28364, .F. ) ;
#22367 = AXIS2_PLACEMENT_3D ( 'NONE', #6766, #21764, #6456 ) ;
#22368 = CARTESIAN_POINT ( 'NONE',  ( 21.24078103779999793, -96.65227117190001138, 0.9777240160550001447 ) ) ;
#22369 = DIRECTION ( 'NONE',  ( 0.04503285875970659130, 0.000000000000000000, 0.9989855062171465461 ) ) ;
#22370 = CARTESIAN_POINT ( 'NONE',  ( -40.00000000000000000, -73.50000000000000000, 3.397282455350000038E-15 ) ) ;
#22371 = CARTESIAN_POINT ( 'NONE',  ( -25.24361395089999860, -94.34469964519999508, -3.017224276749999934 ) ) ;
#22372 = EDGE_CURVE ( 'NONE', #3493, #21366, #13079, .T. ) ;
#22373 = DIRECTION ( 'NONE',  ( 0.000000000000000000, 1.000000000000000000, 0.000000000000000000 ) ) ;
#22374 = EDGE_CURVE ( 'NONE', #21778, #24612, #16191, .T. ) ;
#22375 = CARTESIAN_POINT ( 'NONE',  ( -11.22008280823478010, -57.43018266902328861, -22.06025754104976855 ) ) ;
#22376 = EDGE_LOOP ( 'NONE', ( #26137, #8031, #10704 ) ) ;
#22377 = DIRECTION ( 'NONE',  ( 0.000000000000000000, -1.000000000000000000, 0.000000000000000000 ) ) ;
#22378 = CARTESIAN_POINT ( 'NONE',  ( 7.627567457969999687, -74.00000025069999765, -38.62788781560000473 ) ) ;
#22379 = VERTEX_POINT ( 'NONE', #15748 ) ;
#22380 = EDGE_CURVE ( 'NONE', #6342, #15463, #4326, .T. ) ;
#22381 = CARTESIAN_POINT ( 'NONE',  ( 8.363467862889008231, -92.62800705134604584, 29.33100262325347884 ) ) ;
#22382 = EDGE_CURVE ( 'NONE', #13629, #25229, #16836, .T. ) ;
#22383 = CARTESIAN_POINT ( 'NONE',  ( 23.03829042120000281, -52.56313962710000709, 10.32398954119999956 ) ) ;
#22384 = CARTESIAN_POINT ( 'NONE',  ( -12.09704001540000107, -80.00000000000000000, 47.10905722069999513 ) ) ;
#22385 = CARTESIAN_POINT ( 'NONE',  ( 22.20719543259999895, -26.03958238319999907, 9.782350785770001167 ) ) ;
#22386 = AXIS2_PLACEMENT_3D ( 'NONE', #2586, #21079, #23670 ) ;
#22387 = CARTESIAN_POINT ( 'NONE',  ( 23.52739736179999852, -94.89419905519999077, -6.742685077560000018 ) ) ;
#22388 = AXIS2_PLACEMENT_3D ( 'NONE', #2527, #18101, #22627 ) ;
#22389 = AXIS2_PLACEMENT_3D ( 'NONE', #22793, #18271, #2833 ) ;
#22390 = CARTESIAN_POINT ( 'NONE',  ( 21.68405932330000141, -63.95915174670000169, 11.72027971770000043 ) ) ;
#22391 = CARTESIAN_POINT ( 'NONE',  ( 11.75050204837996048, -98.73470957942969051, 14.28466904018460504 ) ) ;
#22392 = CARTESIAN_POINT ( 'NONE',  ( -17.18418019329581981, -97.30182645328051194, 10.80309787203176697 ) ) ;
#22393 = ORIENTED_EDGE ( 'NONE', *, *, #19822, .F. ) ;
#22394 = B_SPLINE_CURVE_WITH_KNOTS ( 'NONE', 3,
 ( #23892, #10047, #8429, #1341, #17332, #5834, #3381, #3795, #1620, #5691, #12246, #10457, #1482, #21423, #21158, #14980, #23605 ),
 .UNSPECIFIED., .F., .F.,
 ( 4, 2, 2, 1, 1, 1, 1, 1, 2, 2, 4 ),
 ( 0.000000000000000000, 0.2500000000000329181, 0.3750000000000496270, 0.4375000000000587863, 0.4687500000000633937, 0.4843750000000668354, 0.4921875000000687783, 0.4960937500000701106, 0.4980468750000695555, 0.5000000000000690559, 1.000000000000000000 ),
 .UNSPECIFIED. ) ;
#22395 = CARTESIAN_POINT ( 'NONE',  ( -23.49132717730000053, -93.00000000000000000, -19.26887671769999955 ) ) ;
#22396 = CARTESIAN_POINT ( 'NONE',  ( -5.531648500956975134, -100.7167551761413620, 16.12067131280068821 ) ) ;
#22397 = CARTESIAN_POINT ( 'NONE',  ( -12.70399662470000024, -100.4071172650000108, -10.97916378790000103 ) ) ;
#22398 = CIRCLE ( 'NONE', #17268, 3.500000000000003109 ) ;
#22399 = DIRECTION ( 'NONE',  ( 1.000000000000000000, 0.000000000000000000, 0.000000000000000000 ) ) ;
#22400 = CARTESIAN_POINT ( 'NONE',  ( 23.44995121140226857, -63.81246114131585045, -7.514631542302712575 ) ) ;
#22401 = ORIENTED_EDGE ( 'NONE', *, *, #24510, .T. ) ;
#22402 = DIRECTION ( 'NONE',  ( 0.4794255386042041156, 0.000000000000000000, 0.8775825618903720926 ) ) ;
#22403 = ORIENTED_EDGE ( 'NONE', *, *, #26083, .F. ) ;
#22404 = DIRECTION ( 'NONE',  ( 0.000000000000000000, -1.000000000000000000, 0.000000000000000000 ) ) ;
#22405 = CARTESIAN_POINT ( 'NONE',  ( 25.13293939673078370, -49.51244866357122021, 1.380189421151490459 ) ) ;
#22406 = TOROIDAL_SURFACE ( 'NONE', #18211, 38.75000000000000000, 0.5000000000000000000 ) ;
#22407 = CARTESIAN_POINT ( 'NONE',  ( -18.27190991239673679, -94.89419557768216862, 16.28310526143894776 ) ) ;
#22408 = CIRCLE ( 'NONE', #19605, 3.000000000000002665 ) ;
#22409 = VERTEX_POINT ( 'NONE', #2962 ) ;
#22410 = EDGE_CURVE ( 'NONE', #13987, #14188, #16049, .T. ) ;
#22411 = AXIS2_PLACEMENT_3D ( 'NONE', #24572, #24871, #19898 ) ;
#22412 = VERTEX_POINT ( 'NONE', #9494 ) ;
#22413 = CARTESIAN_POINT ( 'NONE',  ( -23.16986609970000188, -72.82938648530000592, 16.90925194980000157 ) ) ;
#22414 = CARTESIAN_POINT ( 'NONE',  ( 21.36417435310000101, -94.15497231989999705, 13.67389954769999960 ) ) ;
#22415 = CARTESIAN_POINT ( 'NONE',  ( -15.50938051129999984, -101.3150705480000084, 4.855933523060000034 ) ) ;
#22416 = VERTEX_POINT ( 'NONE', #22478 ) ;
#22417 = CARTESIAN_POINT ( 'NONE',  ( 16.49890011910140331, -94.79581646409930329, 16.97758076399984617 ) ) ;
#22418 = CARTESIAN_POINT ( 'NONE',  ( -22.21526612139999912, -80.34842048189999275, -32.35915136539999537 ) ) ;
#22419 = EDGE_CURVE ( 'NONE', #19835, #5829, #11225, .T. ) ;
#22420 = CARTESIAN_POINT ( 'NONE',  ( -3.689713002109519024, -69.66052405845533713, -28.05308719045783405 ) ) ;
#22421 = CARTESIAN_POINT ( 'NONE',  ( 12.07615687260000037, -101.1292389600000092, -9.727384960349999332 ) ) ;
#22422 = CARTESIAN_POINT ( 'NONE',  ( -13.23807356550000058, -93.85715850769999236, -21.09154035150000084 ) ) ;
#22423 = DIRECTION ( 'NONE',  ( 1.000000000000000000, 0.000000000000000000, 0.000000000000000000 ) ) ;
#22424 = ORIENTED_EDGE ( 'NONE', *, *, #663, .F. ) ;
#22425 = DIRECTION ( 'NONE',  ( 1.000000000000000000, 0.000000000000000000, 0.000000000000000000 ) ) ;
#22426 = B_SPLINE_CURVE_WITH_KNOTS ( 'NONE', 3,
 ( #13487, #22396, #11439, #27062, #20494, #275, #9117, #13785, #18018, #26916, #20345, #15818, #22687, #13640, #22548, #17581, #14504, #20800 ),
 .UNSPECIFIED., .F., .F.,
 ( 4, 2, 2, 2, 1, 1, 1, 1, 2, 2, 4 ),
 ( 0.000000000000000000, 0.2500000000000132672, 0.3750000000000190958, 0.4375000000000223710, 0.4687500000000239808, 0.4843750000000250910, 0.4921875000000259792, 0.4960937500000274225, 0.4980468750000278666, 0.5000000000000283107, 1.000000000000000000 ),
 .UNSPECIFIED. ) ;
#22427 = CARTESIAN_POINT ( 'NONE',  ( -2.585646220079999669, -58.19955242929999883, -25.25977730230000162 ) ) ;
#22428 = CARTESIAN_POINT ( 'NONE',  ( -40.32201634399999790, -74.31845592130000000, 7.253647055850000136 ) ) ;
#22429 = CARTESIAN_POINT ( 'NONE',  ( -22.22906645670000003, -74.39508596250000494, -32.83566817450000030 ) ) ;
#22430 = AXIS2_PLACEMENT_3D ( 'NONE', #1161, #6048, #12742 ) ;
#22431 = CARTESIAN_POINT ( 'NONE',  ( -2.707548242715575260, -100.1989206112474733, -17.50807487101777227 ) ) ;
#22432 = LINE ( 'NONE', #13372, #4583 ) ;
#22433 = CONICAL_SURFACE ( 'NONE', #27098, 1.732050807582486307, 1.047197551199999799 ) ;
#22434 = CARTESIAN_POINT ( 'NONE',  ( -7.494372175572003414, -73.99988466611407034, 38.93864016370615388 ) ) ;
#22435 = CARTESIAN_POINT ( 'NONE',  ( -17.93028678539999987, -18.50000000000000000, 10.99759328500000066 ) ) ;
#22436 = ORIENTED_EDGE ( 'NONE', *, *, #834, .T. ) ;
#22437 = CARTESIAN_POINT ( 'NONE',  ( -7.384731607069999981, -94.63960343449998902, -22.55849074379999664 ) ) ;
#22438 = CARTESIAN_POINT ( 'NONE',  ( -38.58844719860000083, -65.17124718639999514, -2.835686332019999867 ) ) ;
#22439 = CARTESIAN_POINT ( 'NONE',  ( -24.39543497051741738, -92.52048598158059178, -18.30609232284913190 ) ) ;
#22440 = DIRECTION ( 'NONE',  ( 0.9993816408608721114, 0.000000000000000000, -0.03516156865429537204 ) ) ;
#22441 = CARTESIAN_POINT ( 'NONE',  ( 22.14137210370000020, -52.59522851920000619, 10.05377507689999916 ) ) ;
#22442 = B_SPLINE_SURFACE_WITH_KNOTS ( 'NONE', 5, 5, ( 
 ( #23216, #9795, #23497, #18558, #5299, #12392, #1355, #18849, #14186 ),
 ( #23082, #7772, #27603, #23354, #3397, #7642, #3265, #12118, #1094 ),
 ( #27736, #16644, #21173, #21441, #28560, #1917, #2065, #21582, #8596 ),
 ( #1502, #28691, #10760, #5982, #19529, #24046, #3809, #14729, #17063 ),
 ( #17206, #17353, #6271, #14862, #12672, #19390, #8304, #26094, #6123 ),
 ( #26384, #19812, #28143, #10342, #24199, #23766, #28414, #19672, #28270 ) ),
 .UNSPECIFIED., .F., .F., .F.,
 ( 6, 6 ),
 ( 6, 3, 6 ),
 ( 36.59856967580000031, 66.18347591719999912 ),
 ( 0.000000000000000000, 1.000000000000000000, 2.000000000000000000 ),
 .UNSPECIFIED. ) ;
#22443 =( NAMED_UNIT ( * ) PLANE_ANGLE_UNIT ( ) SI_UNIT ( $, .RADIAN. ) );
#22444 = DIRECTION ( 'NONE',  ( 1.000000000000000000, 0.000000000000000000, 0.000000000000000000 ) ) ;
#22445 = CARTESIAN_POINT ( 'NONE',  ( -12.17175179449999867, -57.47855601710000428, -19.93971688569999756 ) ) ;
#22446 = ORIENTED_EDGE ( 'NONE', *, *, #20855, .F. ) ;
#22447 = ADVANCED_FACE ( 'NONE', ( #9050 ), #4257, .T. ) ;
#22448 = CONICAL_SURFACE ( 'NONE', #26166, 25.14975229270001833, 0.4276056667390000787 ) ;
#22449 = CARTESIAN_POINT ( 'NONE',  ( 17.98420307009999775, -100.0012764430000090, 1.149933891269999897 ) ) ;
#22450 = ORIENTED_EDGE ( 'NONE', *, *, #22182, .F. ) ;
#22451 = CARTESIAN_POINT ( 'NONE',  ( -10.92291579689999992, -42.27245207490000212, 20.04758140150000045 ) ) ;
#22452 = DIRECTION ( 'NONE',  ( 1.000000000000000000, 0.000000000000000000, 0.000000000000000000 ) ) ;
#22453 = VERTEX_POINT ( 'NONE', #24808 ) ;
#22454 = AXIS2_PLACEMENT_3D ( 'NONE', #12651, #10592, #6253 ) ;
#22455 = CARTESIAN_POINT ( 'NONE',  ( 14.93031796050000004, -95.36050459580000904, 17.28030220389999982 ) ) ;
#22456 = PLANE ( 'NONE',  #19655 ) ;
#22457 = B_SPLINE_CURVE_WITH_KNOTS ( 'NONE', 3,
 ( #4324, #28642, #17735, #4768, #28783, #2596 ),
 .UNSPECIFIED., .F., .F.,
 ( 4, 2, 4 ),
 ( 0.000000000000000000, 0.5000000000000000000, 1.000000000000000000 ),
 .UNSPECIFIED. ) ;
#22458 = CARTESIAN_POINT ( 'NONE',  ( 8.915186176627273085, -94.60934249679789332, -23.38371009848104976 ) ) ;
#22459 = CARTESIAN_POINT ( 'NONE',  ( -25.57735248450000043, -16.00000000000000000, -46.81902967690000139 ) ) ;
#22460 = DIRECTION ( 'NONE',  ( 1.000000000000000000, 0.000000000000000000, 0.000000000000000000 ) ) ;
#22461 = CARTESIAN_POINT ( 'NONE',  ( 26.84355216712550174, -67.87586260162430563, 1.442230305706864169 ) ) ;
#22462 = CARTESIAN_POINT ( 'NONE',  ( 21.60334004033046895, -37.79333402771170825, -8.049301293328291251 ) ) ;
#22463 = ORIENTED_EDGE ( 'NONE', *, *, #26829, .T. ) ;
#22464 = CARTESIAN_POINT ( 'NONE',  ( 6.962673402130000078, -92.84292488370000740, -28.64060064759999946 ) ) ;
#22465 = PLANE ( 'NONE',  #14482 ) ;
#22466 = DIRECTION ( 'NONE',  ( 0.000000000000000000, 1.000000000000000000, 0.000000000000000000 ) ) ;
#22467 = VERTEX_POINT ( 'NONE', #20736 ) ;
#22468 = CARTESIAN_POINT ( 'NONE',  ( -38.25000000001038103, -63.32098044081165256, -1.497193467875711503 ) ) ;
#22469 = CARTESIAN_POINT ( 'NONE',  ( -16.58866213250000143, -92.84298581140001261, 21.51064311520000061 ) ) ;
#22470 = CARTESIAN_POINT ( 'NONE',  ( 0.3059185938709999553, -101.1889999979999999, 14.72672055670000013 ) ) ;
#22471 = VERTEX_POINT ( 'NONE', #26700 ) ;
#22472 = FACE_OUTER_BOUND ( 'NONE', #17201, .T. ) ;
#22473 = ADVANCED_FACE ( 'NONE', ( #6741 ), #23402, .T. ) ;
#22474 = AXIS2_PLACEMENT_3D ( 'NONE', #11421, #18144, #7373 ) ;
#22475 = VECTOR ( 'NONE', #24932, 1000.000000000000000 ) ;
#22476 = CARTESIAN_POINT ( 'NONE',  ( 0.1603605168660000024, -101.1030539030000028, -15.43647320760000063 ) ) ;
#22477 = CARTESIAN_POINT ( 'NONE',  ( 7.084351940260000369, -59.04260968250000019, -22.31839619009999964 ) ) ;
#22478 = CARTESIAN_POINT ( 'NONE',  ( -22.27191869549999836, -94.59276292389999696, -8.381623179300000004 ) ) ;
#22479 = CARTESIAN_POINT ( 'NONE',  ( -10.76543513999999924, -34.63364287790000162, -21.24130719339999729 ) ) ;
#22480 = CIRCLE ( 'NONE', #20133, 0.3500000000000003664 ) ;
#22481 = CARTESIAN_POINT ( 'NONE',  ( 27.98858332410410199, -71.34444037274488437, 1.047634458806025126 ) ) ;
#22482 = ORIENTED_EDGE ( 'NONE', *, *, #1951, .T. ) ;
#22483 = ADVANCED_FACE ( 'NONE', ( #21284 ), #27434, .T. ) ;
#22484 = FACE_OUTER_BOUND ( 'NONE', #28279, .T. ) ;
#22485 = CARTESIAN_POINT ( 'NONE',  ( 0.000000000000000000, -10.95575221240000019, 0.000000000000000000 ) ) ;
#22486 = TOROIDAL_SURFACE ( 'NONE', #25748, 4.500000000000000000, 0.5000000000000000000 ) ;
#22487 = DIRECTION ( 'NONE',  ( 1.000000000000000000, 0.000000000000000000, 0.000000000000000000 ) ) ;
#22488 = ORIENTED_EDGE ( 'NONE', *, *, #16364, .F. ) ;
#22489 = CARTESIAN_POINT ( 'NONE',  ( 7.562763921490000207, -74.00035141509999903, 39.03055149349999908 ) ) ;
#22490 = DIRECTION ( 'NONE',  ( 0.000000000000000000, 1.000000000000000000, 0.000000000000000000 ) ) ;
#22491 = LINE ( 'NONE', #20290, #16876 ) ;
#22492 = EDGE_CURVE ( 'NONE', #3368, #2835, #22033, .T. ) ;
#22493 = CARTESIAN_POINT ( 'NONE',  ( 22.98461340545973641, -19.47630996313253959, 1.205578334398293538 ) ) ;
#22494 = CARTESIAN_POINT ( 'NONE',  ( -7.109873676839999490, -101.0147083550000104, 13.82755951569999908 ) ) ;
#22495 = EDGE_LOOP ( 'NONE', ( #5186, #16560, #23723, #18331 ) ) ;
#22496 = CARTESIAN_POINT ( 'NONE',  ( 27.03314449209916859, -72.25218846125086714, -11.41478320253755818 ) ) ;
#22497 = CARTESIAN_POINT ( 'NONE',  ( -20.58900368409999970, -58.81362829640000456, 14.87320149399999991 ) ) ;
#22498 = CARTESIAN_POINT ( 'NONE',  ( 8.339202836120000129, -36.74552967150000171, -21.40376449809999926 ) ) ;
#22499 = AXIS2_PLACEMENT_3D ( 'NONE', #22860, #10941, #4272 ) ;
#22500 = CARTESIAN_POINT ( 'NONE',  ( 21.56299924104185095, -36.38197226018986896, -6.848569379388298906 ) ) ;
#22501 = CARTESIAN_POINT ( 'NONE',  ( 7.994803016720000599, -99.33439196809999316, 16.09261115110000162 ) ) ;
#22502 = CARTESIAN_POINT ( 'NONE',  ( -10.00000000000000000, -42.50000000000000000, 1.224606353819999829E-15 ) ) ;
#22503 = CARTESIAN_POINT ( 'NONE',  ( -12.86681839629088131, -19.48210950177368517, 19.53479179472106608 ) ) ;
#22504 = CARTESIAN_POINT ( 'NONE',  ( -7.325370793560000315, -45.73899999920000425, -24.94672208400000102 ) ) ;
#22505 = DIRECTION ( 'NONE',  ( 0.000000000000000000, -1.000000000000000000, 0.000000000000000000 ) ) ;
#22506 = ORIENTED_EDGE ( 'NONE', *, *, #2685, .F. ) ;
#22507 = DIRECTION ( 'NONE',  ( 1.000000000000000000, 0.000000000000000000, 0.000000000000000000 ) ) ;
#22508 = CARTESIAN_POINT ( 'NONE',  ( -13.81324249570000084, -18.62337005500000231, 20.27492115300000108 ) ) ;
#22509 = DIRECTION ( 'NONE',  ( 0.000000000000000000, -1.000000000000000000, 0.000000000000000000 ) ) ;
#22510 = CARTESIAN_POINT ( 'NONE',  ( -37.94434432234054810, -65.71171096279377366, 0.8680092137352279913 ) ) ;
#22511 = EDGE_CURVE ( 'NONE', #2951, #6426, #14966, .T. ) ;
#22512 = CIRCLE ( 'NONE', #27170, 5.000000000000000000 ) ;
#22513 = CARTESIAN_POINT ( 'NONE',  ( -29.86363316589999783, -111.0000000000000000, 0.3450520984299999538 ) ) ;
#22514 = DIRECTION ( 'NONE',  ( 1.000000000000000000, 0.000000000000000000, 0.000000000000000000 ) ) ;
#22515 = CARTESIAN_POINT ( 'NONE',  ( 27.48096935534069019, -93.08384138313874701, 9.598179995941348963 ) ) ;
#22516 = EDGE_LOOP ( 'NONE', ( #17459, #20229, #11158, #6059 ) ) ;
#22517 = CARTESIAN_POINT ( 'NONE',  ( -29.74766882723250561, -92.84927079009166562, 6.732478952539187489 ) ) ;
#22518 = B_SPLINE_CURVE_WITH_KNOTS ( 'NONE', 3,
 ( #8780, #28468, #1971, #8504, #26300, #15482, #11257, #17691, #15182, #26437, #24096, #24392, #10814, #19723, #28611, #8642, #6466, #26579 ),
 .UNSPECIFIED., .F., .F.,
 ( 4, 2, 2, 2, 2, 2, 2, 2, 4 ),
 ( 0.000000000000000000, 0.1249999999999761302, 0.1874999999999816536, 0.2499999999999872324, 0.5000000000000115463, 0.6250000000000236478, 0.6875000000000296430, 0.7500000000000357492, 1.000000000000000000 ),
 .UNSPECIFIED. ) ;
#22519 = ADVANCED_FACE ( 'NONE', ( #8162 ), #28027, .T. ) ;
#22520 = CIRCLE ( 'NONE', #24843, 3.750000000000000000 ) ;
#22521 = ORIENTED_EDGE ( 'NONE', *, *, #10852, .F. ) ;
#22522 = CARTESIAN_POINT ( 'NONE',  ( -12.88897289979999883, -65.65850715019999484, 21.91133662320000042 ) ) ;
#22523 = CARTESIAN_POINT ( 'NONE',  ( -13.57564758800000071, -60.33093763760000172, 20.91920646410000018 ) ) ;
#22524 = CARTESIAN_POINT ( 'NONE',  ( -38.08875739639999836, -84.00000000000000000, 9.476764215410000247 ) ) ;
#22525 = DIRECTION ( 'NONE',  ( -0.000000000000000000, 1.000000000000000000, 0.000000000000000000 ) ) ;
#22526 = LINE ( 'NONE', #4591, #2260 ) ;
#22527 = DIRECTION ( 'NONE',  ( -0.9993816408608721114, 0.000000000000000000, 0.03516156865429537204 ) ) ;
#22528 = VECTOR ( 'NONE', #13376, 1000.000000000000000 ) ;
#22529 = CARTESIAN_POINT ( 'NONE',  ( 19.97062749839314577, -19.47948121987873193, -8.623729410243210936 ) ) ;
#22530 = CARTESIAN_POINT ( 'NONE',  ( 16.52251354239999870, -99.77922884479998800, 4.576493590060000116 ) ) ;
#22531 = ORIENTED_EDGE ( 'NONE', *, *, #1109, .T. ) ;
#22532 = CARTESIAN_POINT ( 'NONE',  ( -7.215414233289999757, -74.50000000000000000, -40.70731707320000226 ) ) ;
#22533 = DIRECTION ( 'NONE',  ( 0.000000000000000000, -1.000000000000000000, 0.000000000000000000 ) ) ;
#22534 = CARTESIAN_POINT ( 'NONE',  ( -15.43774787200000098, -99.62155223620000299, -8.682365224729998943 ) ) ;
#22535 = VERTEX_POINT ( 'NONE', #28541 ) ;
#22536 = CARTESIAN_POINT ( 'NONE',  ( 23.10863584609999677, -55.79355142130000900, 10.36080582650000004 ) ) ;
#22537 = CYLINDRICAL_SURFACE ( 'NONE', #13219, 0.8000000000000008216 ) ;
#22538 = CARTESIAN_POINT ( 'NONE',  ( 0.000000000000000000, -10.50000000000000000, 0.000000000000000000 ) ) ;
#22539 = CARTESIAN_POINT ( 'NONE',  ( -11.81899278133277775, -64.69849623153378104, -22.71259346144224978 ) ) ;
#22540 = CIRCLE ( 'NONE', #19726, 7.250000000000000000 ) ;
#22541 = CARTESIAN_POINT ( 'NONE',  ( 0.000000000000000000, -92.50000000000000000, 29.91857981989999971 ) ) ;
#22542 = CARTESIAN_POINT ( 'NONE',  ( 23.54313657470000010, -94.98812477599999227, -6.784142499889999733 ) ) ;
#22543 = CARTESIAN_POINT ( 'NONE',  ( 22.17953377930000158, -65.07443093669999712, 11.85657293289999892 ) ) ;
#22544 = CARTESIAN_POINT ( 'NONE',  ( -19.43609242099999790, -92.50000000000000000, -23.50506990850000122 ) ) ;
#22545 = CARTESIAN_POINT ( 'NONE',  ( -17.56540178540820918, -95.86369604245908249, 13.50288865853636366 ) ) ;
#22546 = EDGE_LOOP ( 'NONE', ( #12338, #4533, #7399, #662 ) ) ;
#22547 = FACE_OUTER_BOUND ( 'NONE', #19078, .T. ) ;
#22548 = CARTESIAN_POINT ( 'NONE',  ( -3.128864287929727706, -98.07255008584144207, 20.23552373180469388 ) ) ;
#22549 = CARTESIAN_POINT ( 'NONE',  ( -13.32816354210000043, -99.92967571559999840, -11.12411009090000036 ) ) ;
#22550 = CYLINDRICAL_SURFACE ( 'NONE', #10392, 15.99999999999999645 ) ;
#22551 = CARTESIAN_POINT ( 'NONE',  ( -39.85902549739999756, -74.23956954080000514, -7.332363419530000037 ) ) ;
#22552 = ORIENTED_EDGE ( 'NONE', *, *, #14543, .T. ) ;
#22553 = EDGE_CURVE ( 'NONE', #21733, #6187, #13098, .T. ) ;
#22554 = VECTOR ( 'NONE', #16577, 1000.000000000000000 ) ;
#22555 = CARTESIAN_POINT ( 'NONE',  ( 26.34145817392794342, -92.82334897396464157, -15.37457621828394672 ) ) ;
#22556 = EDGE_LOOP ( 'NONE', ( #8658, #25532, #6044, #15523 ) ) ;
#22557 = EDGE_CURVE ( 'NONE', #8623, #7572, #24138, .T. ) ;
#22558 = ADVANCED_FACE ( 'NONE', ( #3796 ), #5679, .T. ) ;
#22559 = CARTESIAN_POINT ( 'NONE',  ( -1.283023294879999998, -101.1889999979999999, -16.20107482390000087 ) ) ;
#22560 = CARTESIAN_POINT ( 'NONE',  ( 1.375203621220000061, -94.98812769030000425, 24.46248643120000210 ) ) ;
#22561 = COLOUR_RGB ( '', 0.09019608, 0.27058824, 0.51372549) ;
#22562 = CARTESIAN_POINT ( 'NONE',  ( 8.039511664659999113, -92.65193295299998510, 26.91643347890000015 ) ) ;
#22563 = VERTEX_POINT ( 'NONE', #17333 ) ;
#22564 = AXIS2_PLACEMENT_3D ( 'NONE', #22115, #2156, #20210 ) ;
#22565 = ORIENTED_EDGE ( 'NONE', *, *, #9575, .T. ) ;
#22566 = CARTESIAN_POINT ( 'NONE',  ( -22.94912671726251219, -71.22806229626020524, 15.96158107121579661 ) ) ;
#22567 = CARTESIAN_POINT ( 'NONE',  ( 0.000000000000000000, -2.000000000000000000, 0.000000000000000000 ) ) ;
#22568 = CARTESIAN_POINT ( 'NONE',  ( 47.09015203950000483, -74.29080663029999698, -1.541671319510000027 ) ) ;
#22569 = ORIENTED_EDGE ( 'NONE', *, *, #22750, .T. ) ;
#22570 = CARTESIAN_POINT ( 'NONE',  ( 7.152485405711615840, -73.50000015768027595, -38.81101221961867509 ) ) ;
#22571 = CARTESIAN_POINT ( 'NONE',  ( -21.70609662629999903, -80.13404657770000483, -32.70204620079999813 ) ) ;
#22572 = CARTESIAN_POINT ( 'NONE',  ( -3.058911230670000148, -72.82938648530000592, -28.52031834779999997 ) ) ;
#22573 = DIRECTION ( 'NONE',  ( 1.000000000000000000, 0.000000000000000000, 0.000000000000000000 ) ) ;
#22574 = CARTESIAN_POINT ( 'NONE',  ( -23.69410943009695103, -94.52419745024906206, -3.934991533140109077 ) ) ;
#22575 = ORIENTED_EDGE ( 'NONE', *, *, #17966, .T. ) ;
#22576 = CARTESIAN_POINT ( 'NONE',  ( -32.25000000000000000, -74.00000000000000000, 2.464695114664749584E-15 ) ) ;
#22577 = CARTESIAN_POINT ( 'NONE',  ( -16.74373768950000141, -99.87169021820000125, 2.814689237420000101 ) ) ;
#22578 = CARTESIAN_POINT ( 'NONE',  ( -39.49475000900000765, -74.05254684259999465, 7.367397733549999828 ) ) ;
#22579 = CARTESIAN_POINT ( 'NONE',  ( -21.87483401080000078, -74.28769487450000497, -32.59760389210000397 ) ) ;
#22580 = CARTESIAN_POINT ( 'NONE',  ( -11.73626238637177899, -94.71481465629089769, -21.34524630996246586 ) ) ;
#22581 = CARTESIAN_POINT ( 'NONE',  ( -27.68682485439999752, -17.89999999999999858, -50.68039294919999804 ) ) ;
#22582 = CARTESIAN_POINT ( 'NONE',  ( -7.396579754587796707, -73.99963493658084701, 39.20624479181404354 ) ) ;
#22583 = CARTESIAN_POINT ( 'NONE',  ( -18.43157295690000197, -18.85467989400000022, 11.82421860260000024 ) ) ;
#22584 = ORIENTED_EDGE ( 'NONE', *, *, #20581, .F. ) ;
#22585 = ADVANCED_FACE ( 'NONE', ( #22145 ), #6146, .F. ) ;
#22586 = CARTESIAN_POINT ( 'NONE',  ( -13.18687770350000044, -93.32822605769999313, -23.58441588660000221 ) ) ;
#22587 = AXIS2_PLACEMENT_3D ( 'NONE', #19480, #8831, #9392 ) ;
#22588 = CARTESIAN_POINT ( 'NONE',  ( 22.64274859190000200, -63.79833278959999632, 10.75909410010000045 ) ) ;
#22589 = CARTESIAN_POINT ( 'NONE',  ( 8.798272373610000585, -34.78948601350000303, -20.39306157709999923 ) ) ;
#22590 = CARTESIAN_POINT ( 'NONE',  ( 15.69315028655411659, -101.4304678898235039, 3.891722348338785942 ) ) ;
#22591 = CARTESIAN_POINT ( 'NONE',  ( -15.42268960139999834, -101.6484611540000031, 4.259183661159999801 ) ) ;
#22592 = VERTEX_POINT ( 'NONE', #28674 ) ;
#22593 = CARTESIAN_POINT ( 'NONE',  ( -14.93121078260000090, -79.49999975080000070, 36.29905569799999654 ) ) ;
#22594 = EDGE_CURVE ( 'NONE', #20759, #15974, #24785, .T. ) ;
#22595 = DIRECTION ( 'NONE',  ( 0.000000000000000000, -1.000000000000000000, 0.000000000000000000 ) ) ;
#22596 = CARTESIAN_POINT ( 'NONE',  ( 9.525697108589946893, -93.08996184747134350, 27.45793313423234139 ) ) ;
#22597 = ORIENTED_EDGE ( 'NONE', *, *, #8750, .F. ) ;
#22598 = DIRECTION ( 'NONE',  ( 1.000000000000000000, 0.000000000000000000, 0.000000000000000000 ) ) ;
#22599 = CARTESIAN_POINT ( 'NONE',  ( 46.99997450946052169, -74.14530279077403918, -1.887577394871021719 ) ) ;
#22600 = ORIENTED_EDGE ( 'NONE', *, *, #11403, .T. ) ;
#22601 = DIRECTION ( 'NONE',  ( 1.000000000000000000, 0.000000000000000000, 0.000000000000000000 ) ) ;
#22602 = CARTESIAN_POINT ( 'NONE',  ( 2.042810365310000056E-12, -74.50000000000000000, -2.458477865729999957E-12 ) ) ;
#22603 = ORIENTED_EDGE ( 'NONE', *, *, #2048, .T. ) ;
#22604 = LINE ( 'NONE', #25230, #9892 ) ;
#22605 = AXIS2_PLACEMENT_3D ( 'NONE', #26067, #3643, #12369 ) ;
#22606 = CARTESIAN_POINT ( 'NONE',  ( 4.127715330941034821, -93.15741110422700899, -28.33879718941593495 ) ) ;
#22607 = DIRECTION ( 'NONE',  ( 1.000000000000000000, 0.000000000000000000, 0.000000000000000000 ) ) ;
#22608 = CARTESIAN_POINT ( 'NONE',  ( -19.02290610980000096, -97.53593570510001598, 6.397707897409999234 ) ) ;
#22609 = FACE_OUTER_BOUND ( 'NONE', #21654, .T. ) ;
#22610 = CARTESIAN_POINT ( 'NONE',  ( -10.20110288159999890, -82.25000000000000000, -41.00000000000000000 ) ) ;
#22611 = ORIENTED_EDGE ( 'NONE', *, *, #24757, .T. ) ;
#22612 = CARTESIAN_POINT ( 'NONE',  ( 7.085361681160000202, -92.56168957700000988, -28.78018708169999940 ) ) ;
#22613 = DIRECTION ( 'NONE',  ( 0.000000000000000000, 1.000000000000000000, 0.000000000000000000 ) ) ;
#22614 = DIRECTION ( 'NONE',  ( 0.4794255386042040046, 0.000000000000000000, 0.8775825618903722036 ) ) ;
#22615 = VERTEX_POINT ( 'NONE', #17624 ) ;
#22616 = EDGE_CURVE ( 'NONE', #2835, #27862, #23784, .T. ) ;
#22617 = FACE_OUTER_BOUND ( 'NONE', #6896, .T. ) ;
#22618 = DIRECTION ( 'NONE',  ( 0.000000000000000000, -1.000000000000000000, 0.000000000000000000 ) ) ;
#22619 = CARTESIAN_POINT ( 'NONE',  ( 28.19022166989999789, -39.75000000000000000, 51.60185463919999194 ) ) ;
#22620 = EDGE_CURVE ( 'NONE', #27211, #15688, #11727, .T. ) ;
#22621 = CARTESIAN_POINT ( 'NONE',  ( -2.903039748510000351, -94.98812477769999418, 23.52859306979999943 ) ) ;
#22622 = CARTESIAN_POINT ( 'NONE',  ( -18.44190124780000062, -19.46163090479999980, 12.50665444260000037 ) ) ;
#22623 = CYLINDRICAL_SURFACE ( 'NONE', #9580, 20.64285714289999873 ) ;
#22624 = CARTESIAN_POINT ( 'NONE',  ( 31.51289799120000268, -73.45782179829998881, -20.31705881479999931 ) ) ;
#22625 = CARTESIAN_POINT ( 'NONE',  ( 2.162714451969999821E-13, -111.0000000000000000, 6.000533403490000639E-12 ) ) ;
#22626 = EDGE_CURVE ( 'NONE', #23505, #23386, #10893, .T. ) ;
#22627 = DIRECTION ( 'NONE',  ( 1.000000000000000000, 0.000000000000000000, 0.000000000000000000 ) ) ;
#22628 = B_SPLINE_CURVE_WITH_KNOTS ( 'NONE', 3,
 ( #27267, #2794, #6719, #28 ),
 .UNSPECIFIED., .F., .F.,
 ( 4, 4 ),
 ( -0.1274251584810000004, -1.776356839400250465E-15 ),
 .UNSPECIFIED. ) ;
#22629 = ORIENTED_EDGE ( 'NONE', *, *, #25993, .F. ) ;
#22630 = CARTESIAN_POINT ( 'NONE',  ( 10.07773541299999920, -36.00000000000000000, -20.87139911950000126 ) ) ;
#22631 = CARTESIAN_POINT ( 'NONE',  ( 0.000000000000000000, -39.50000000000000000, 0.000000000000000000 ) ) ;
#22632 = CARTESIAN_POINT ( 'NONE',  ( -43.12299426110000411, -65.19264941160000149, 0.2176643648609999926 ) ) ;
#22633 = CARTESIAN_POINT ( 'NONE',  ( 0.000000000000000000, -82.50000000000000000, 0.000000000000000000 ) ) ;
#22634 = VERTEX_POINT ( 'NONE', #27674 ) ;
#22635 = AXIS2_PLACEMENT_3D ( 'NONE', #7953, #9849, #5486 ) ;
#22636 = CARTESIAN_POINT ( 'NONE',  ( 36.59060436630000623, -79.00000000000000000, -14.75000000000000000 ) ) ;
#22637 = CARTESIAN_POINT ( 'NONE',  ( 20.48611068019999948, -93.36531860659999893, 16.28991794210000066 ) ) ;
#22638 = CARTESIAN_POINT ( 'NONE',  ( 24.20787553755564048, -19.49659809026794832, 1.495029698088813142 ) ) ;
#22639 = CARTESIAN_POINT ( 'NONE',  ( -7.421872664780000406, -100.8815367389999977, 13.80620562409999863 ) ) ;
#22640 = CARTESIAN_POINT ( 'NONE',  ( 26.84513186441053989, -72.48886963431783670, -10.90665099628932388 ) ) ;
#22641 = CARTESIAN_POINT ( 'NONE',  ( -12.52509995851851166, -101.6297509123138099, -9.979436452931571111 ) ) ;
#22642 = CARTESIAN_POINT ( 'NONE',  ( 8.367124212330001143, -37.94838740809999678, -21.73111097249999801 ) ) ;
#22643 = CARTESIAN_POINT ( 'NONE',  ( 8.607817759397720536, -19.47905375331706423, -19.99126106825392313 ) ) ;
#22644 = EDGE_LOOP ( 'NONE', ( #22093, #1132, #10563, #16925 ) ) ;
#22645 = CARTESIAN_POINT ( 'NONE',  ( 7.813212629879998872, -99.08067767480000043, 16.22119575690000204 ) ) ;
#22646 = LINE ( 'NONE', #25275, #7959 ) ;
#22647 = DIRECTION ( 'NONE',  ( 0.000000000000000000, -1.000000000000000000, 0.000000000000000000 ) ) ;
#22648 = CARTESIAN_POINT ( 'NONE',  ( -14.65665286289999969, -74.50000000000000000, 36.94583910070000599 ) ) ;
#22649 = B_SPLINE_CURVE_WITH_KNOTS ( 'NONE', 3,
 ( #8145, #19361, #1734, #10574, #14827, #3775 ),
 .UNSPECIFIED., .F., .F.,
 ( 4, 2, 4 ),
 ( 0.000000000000000000, 0.5000000000000000000, 1.000000000000000000 ),
 .UNSPECIFIED. ) ;
#22650 = CARTESIAN_POINT ( 'NONE',  ( 11.33780648110000122, -100.8733988930000010, -10.89600415129999966 ) ) ;
#22651 = CARTESIAN_POINT ( 'NONE',  ( -0.5256375577959999656, -45.99906616869999709, -22.95427111080000060 ) ) ;
#22652 = CARTESIAN_POINT ( 'NONE',  ( 15.88351635808362516, -94.85336603632588037, 17.26556729870110729 ) ) ;
#22653 = ADVANCED_FACE ( 'NONE', ( #9867 ), #14544, .T. ) ;
#22654 = EDGE_CURVE ( 'NONE', #14960, #9596, #27038, .T. ) ;
#22655 = CARTESIAN_POINT ( 'NONE',  ( 23.50753042992814557, -19.50000000000000000, 9.440918867846139761 ) ) ;
#22656 = CARTESIAN_POINT ( 'NONE',  ( 16.41935458950000282, -111.0000000000000000, 3.555952033500000109 ) ) ;
#22657 = FACE_OUTER_BOUND ( 'NONE', #27921, .T. ) ;
#22658 = CARTESIAN_POINT ( 'NONE',  ( 0.000000000000000000, -111.0000000000000000, 0.000000000000000000 ) ) ;
#22659 = DIRECTION ( 'NONE',  ( -0.02411449919422837401, -0.9975499440283625008, 0.06567038980866957143 ) ) ;
#22660 = ORIENTED_EDGE ( 'NONE', *, *, #1721, .F. ) ;
#22661 = CARTESIAN_POINT ( 'NONE',  ( 36.36887021859999436, -74.91502851379999584, -14.85406864730000009 ) ) ;
#22662 = CARTESIAN_POINT ( 'NONE',  ( 22.50364785879999729, -95.66919271840001215, -0.5489143750859999393 ) ) ;
#22663 = CARTESIAN_POINT ( 'NONE',  ( -12.08447405829999965, -59.01570696489999790, 20.27932901980000224 ) ) ;
#22664 = CARTESIAN_POINT ( 'NONE',  ( -19.16019836899999618, -92.50000000000000000, 22.97842938279999814 ) ) ;
#22665 = CARTESIAN_POINT ( 'NONE',  ( 19.57843399940000140, -94.59276292389999696, 13.52682119470000011 ) ) ;
#22666 = DIRECTION ( 'NONE',  ( 1.000000000000000000, 0.000000000000000000, 0.000000000000000000 ) ) ;
#22667 = CARTESIAN_POINT ( 'NONE',  ( -12.07243358760000085, -67.46050599719998786, -24.77970463289999969 ) ) ;
#22668 = EDGE_CURVE ( 'NONE', #19973, #5424, #6619, .T. ) ;
#22669 = CARTESIAN_POINT ( 'NONE',  ( -38.08919256720000135, -63.35440207070000440, 1.043878858160000034 ) ) ;
#22670 = CARTESIAN_POINT ( 'NONE',  ( 16.30068969910000121, -100.0496341300000154, 4.508739917940000730 ) ) ;
#22671 = ORIENTED_EDGE ( 'NONE', *, *, #8007, .T. ) ;
#22672 = SURFACE_STYLE_FILL_AREA ( #10969 ) ;
#22673 = CARTESIAN_POINT ( 'NONE',  ( -17.92518616159999922, -98.60488091089999330, -8.251865930899999313 ) ) ;
#22674 = ORIENTED_EDGE ( 'NONE', *, *, #234, .T. ) ;
#22675 = CARTESIAN_POINT ( 'NONE',  ( 8.456806930322576576, -92.64884742711174681, 29.30416004283850739 ) ) ;
#22676 = ORIENTED_EDGE ( 'NONE', *, *, #3572, .F. ) ;
#22677 = CARTESIAN_POINT ( 'NONE',  ( -40.70731707320000226, -82.25000000000000000, -7.215414233289999757 ) ) ;
#22678 = CARTESIAN_POINT ( 'NONE',  ( -11.77131553929999974, -101.2010924020000004, -9.714008462309999814 ) ) ;
#22679 = B_SPLINE_CURVE_WITH_KNOTS ( 'NONE', 3,
 ( #28103, #5813, #25645, #1600, #5674, #28377 ),
 .UNSPECIFIED., .F., .F.,
 ( 4, 2, 4 ),
 ( 0.000000000000000000, 0.5000000000000002220, 1.000000000000000000 ),
 .UNSPECIFIED. ) ;
#22680 = CARTESIAN_POINT ( 'NONE',  ( 23.14927425619999823, -94.18458606750000683, -7.514520311420000098 ) ) ;
#22681 = CARTESIAN_POINT ( 'NONE',  ( 19.02936265269999794, -18.61794786970000359, 10.32221580289999885 ) ) ;
#22682 = CARTESIAN_POINT ( 'NONE',  ( 11.81986579350000000, -72.00000321289999761, -27.35691362350000233 ) ) ;
#22683 = CARTESIAN_POINT ( 'NONE',  ( 14.04239374870000212, -98.93445099689999722, -12.32916220780000138 ) ) ;
#22684 = B_SPLINE_SURFACE_WITH_KNOTS ( 'NONE', 5, 5, ( 
 ( #15641, #9534, #26746, #2563, #18435, #24542, #13909, #17991, #24696 ),
 ( #11412, #4585, #22364, #2411, #27324, #20172, #6925, #2703, #15790 ),
 ( #4733, #15492, #13311, #9386, #22215, #20313, #9230, #7078, #24842 ),
 ( #18289, #16085, #4881, #4440, #7218, #2262, #16229, #10087, #5738 ),
 ( #7523, #3558, #18872, #20774, #18729, #14343, #829, #7666, #14212 ),
 ( #25430, #27756, #12000, #3286, #12142, #21059, #16666, #25565, #23795 ) ),
 .UNSPECIFIED., .F., .F., .F.,
 ( 6, 6 ),
 ( 6, 3, 6 ),
 ( 4.057198812540000255, 5.368803751829999804 ),
 ( 0.000000000000000000, 0.2500000000000000000, 0.5000000000000000000 ),
 .UNSPECIFIED. ) ;
#22685 = ORIENTED_EDGE ( 'NONE', *, *, #27498, .T. ) ;
#22686 = CARTESIAN_POINT ( 'NONE',  ( -12.41137697900000170, -71.49590739120000649, -25.29708909809999895 ) ) ;
#22687 = CARTESIAN_POINT ( 'NONE',  ( -3.141019993213900463, -98.08323606068540812, 20.21953806862122249 ) ) ;
#22688 = CARTESIAN_POINT ( 'NONE',  ( -13.16264660049999868, -99.58396362730000817, -11.32285879039999799 ) ) ;
#22689 = CARTESIAN_POINT ( 'NONE',  ( 22.05314188356497596, -19.49371746077434153, 9.682146897022342102 ) ) ;
#22690 = LINE ( 'NONE', #16808, #2428 ) ;
#22691 = ORIENTED_EDGE ( 'NONE', *, *, #7763, .F. ) ;
#22692 = AXIS2_PLACEMENT_3D ( 'NONE', #5576, #16062, #1226 ) ;
#22693 = DIRECTION ( 'NONE',  ( -0.7071067811865474617, 0.000000000000000000, 0.7071067811865474617 ) ) ;
#22694 = ORIENTED_EDGE ( 'NONE', *, *, #25039, .T. ) ;
#22695 = AXIS2_PLACEMENT_3D ( 'NONE', #28123, #21700, #19509 ) ;
#22696 = CARTESIAN_POINT ( 'NONE',  ( -23.24818410940000035, -93.00000000000000000, -18.83197690249999923 ) ) ;
#22697 = TOROIDAL_SURFACE ( 'NONE', #19880, 3.500000000000000000, 0.5000000000000000000 ) ;
#22698 = CARTESIAN_POINT ( 'NONE',  ( 11.01541626710000088, -36.00000000000000000, -22.51853742030000305 ) ) ;
#22699 = CARTESIAN_POINT ( 'NONE',  ( -4.683949502529999975, -99.57131247770000471, 16.77925173899999933 ) ) ;
#22700 = CARTESIAN_POINT ( 'NONE',  ( 8.002737880409998894, -92.75793418959999315, 27.16184970260000142 ) ) ;
#22701 = VERTEX_POINT ( 'NONE', #22524 ) ;
#22702 = EDGE_CURVE ( 'NONE', #7043, #19884, #7113, .T. ) ;
#22703 = CARTESIAN_POINT ( 'NONE',  ( -19.73459501710000197, -19.50000000000000000, 14.41863426819999994 ) ) ;
#22704 = EDGE_LOOP ( 'NONE', ( #8720, #8372, #11530, #24734, #4620 ) ) ;
#22705 = CARTESIAN_POINT ( 'NONE',  ( -22.51871667277407241, -69.15146719725277080, 14.91063228687463749 ) ) ;
#22706 = DIRECTION ( 'NONE',  ( 0.000000000000000000, -1.000000000000000000, 0.000000000000000000 ) ) ;
#22707 = CARTESIAN_POINT ( 'NONE',  ( 47.03035266999999919, -74.24775846059999651, -1.795655436139999894 ) ) ;
#22708 = ORIENTED_EDGE ( 'NONE', *, *, #16271, .F. ) ;
#22709 = CARTESIAN_POINT ( 'NONE',  ( 7.232334316196594948, -73.68677077063769332, -39.48689401865327397 ) ) ;
#22710 = CARTESIAN_POINT ( 'NONE',  ( 26.69293917519999937, -16.10310889129999623, 48.86109741659999628 ) ) ;
#22711 = EDGE_CURVE ( 'NONE', #15706, #27953, #11254, .T. ) ;
#22712 = AXIS2_PLACEMENT_3D ( 'NONE', #12560, #14218, #19379 ) ;
#22713 = CARTESIAN_POINT ( 'NONE',  ( 7.584268328590000330, -101.6484612600000048, 14.08825304710000026 ) ) ;
#22714 = CARTESIAN_POINT ( 'NONE',  ( 9.028475982079999795, -35.72979163269999958, -19.84586683699999909 ) ) ;
#22715 = ADVANCED_FACE ( 'NONE', ( #18292 ), #27121, .T. ) ;
#22716 = CARTESIAN_POINT ( 'NONE',  ( 3.835404308829999831, -16.50000000000000000, 7.020660495120000455 ) ) ;
#22717 = DIRECTION ( 'NONE',  ( 0.000000000000000000, 1.000000000000000000, 0.000000000000000000 ) ) ;
#22718 = EDGE_LOOP ( 'NONE', ( #16776, #246, #580 ) ) ;
#22719 = EDGE_CURVE ( 'NONE', #20314, #11594, #18742, .T. ) ;
#22720 = CARTESIAN_POINT ( 'NONE',  ( 13.91983387960000051, -99.74726900420000675, -10.02745453350000027 ) ) ;
#22721 = CARTESIAN_POINT ( 'NONE',  ( 25.14695223519999701, -65.07442822920000935, -0.3759466136490000054 ) ) ;
#22722 = CARTESIAN_POINT ( 'NONE',  ( -22.19594408369999528, -74.22385006870000268, -32.69771557190000522 ) ) ;
#22723 = ORIENTED_EDGE ( 'NONE', *, *, #6214, .F. ) ;
#22724 = AXIS2_PLACEMENT_3D ( 'NONE', #28539, #6700, #6391 ) ;
#22725 = CARTESIAN_POINT ( 'NONE',  ( 26.85107532351766224, -65.44994441702223753, 1.633352019574016101 ) ) ;
#22726 = DIRECTION ( 'NONE',  ( -0.9037419867099893978, 0.000000000000000000, 0.4280775881279951789 ) ) ;
#22727 = CARTESIAN_POINT ( 'NONE',  ( -18.29779733850000056, -18.85499412049999890, 12.26174568899999962 ) ) ;
#22728 = ORIENTED_EDGE ( 'NONE', *, *, #2197, .F. ) ;
#22729 = DIRECTION ( 'NONE',  ( 1.000000000000000000, 0.000000000000000000, 0.000000000000000000 ) ) ;
#22730 = CARTESIAN_POINT ( 'NONE',  ( 23.58466923419999972, -94.98812477769999418, -2.405350023570000051 ) ) ;
#22731 = CARTESIAN_POINT ( 'NONE',  ( 7.623622776310000404, -34.72967069919999972, -21.24008983309999721 ) ) ;
#22732 = CARTESIAN_POINT ( 'NONE',  ( 15.81801911784844172, -101.2145573445017703, 4.083609699486570932 ) ) ;
#22733 = DIRECTION ( 'NONE',  ( 0.9952295494196654602, 0.000000000000000000, -0.09756097560976760563 ) ) ;
#22734 = EDGE_LOOP ( 'NONE', ( #13403, #14812, #2308, #24539 ) ) ;
#22735 = CARTESIAN_POINT ( 'NONE',  ( 47.25000000000000000, -79.00000000000000000, -7.709388683000000122E-13 ) ) ;
#22736 = TOROIDAL_SURFACE ( 'NONE', #22255, 55.85192378860000417, 0.3499999999999999778 ) ;
#22737 = ITEM_DEFINED_TRANSFORMATION ( 'NONE', 'NONE', #28754,  #26433 ) ;
#22738 = CARTESIAN_POINT ( 'NONE',  ( -12.04445256950000065, -60.59277760239999822, -20.32308874549999800 ) ) ;
#22739 = VECTOR ( 'NONE', #20234, 1000.000000000000000 ) ;
#22740 = DIRECTION ( 'NONE',  ( 0.9659258262889443003, 0.000000000000000000, 0.2588190451029837025 ) ) ;
#22741 = CARTESIAN_POINT ( 'NONE',  ( 9.610902359217210034, -93.08494104690983306, 27.46771387074625537 ) ) ;
#22742 = ORIENTED_EDGE ( 'NONE', *, *, #28182, .T. ) ;
#22743 = CARTESIAN_POINT ( 'NONE',  ( 47.00156242777739379, -74.14776025066879583, -1.881670998416149043 ) ) ;
#22744 = EDGE_LOOP ( 'NONE', ( #12382, #21131, #27738 ) ) ;
#22745 = CARTESIAN_POINT ( 'NONE',  ( -13.07981419989999949, -42.23578978099999404, 20.15285454340000015 ) ) ;
#22746 = DIRECTION ( 'NONE',  ( -0.8386955343508021299, 0.000000000000000000, -0.5446005881928723813 ) ) ;
#22747 = VERTEX_POINT ( 'NONE', #24549 ) ;
#22748 = EDGE_CURVE ( 'NONE', #22866, #14159, #3829, .T. ) ;
#22749 = CARTESIAN_POINT ( 'NONE',  ( 32.97008024890000399, -74.00000000000000000, -20.36016474349999683 ) ) ;
#22750 = EDGE_CURVE ( 'NONE', #23155, #11892, #9877, .T. ) ;
#22751 = CARTESIAN_POINT ( 'NONE',  ( -25.71126894084192216, -93.01584921936724015, -6.102654395426379885 ) ) ;
#22752 = CARTESIAN_POINT ( 'NONE',  ( -20.27480073103475178, -94.70873045429671322, 12.26046566542698102 ) ) ;
#22753 = CARTESIAN_POINT ( 'NONE',  ( -19.71577987869999760, -96.53868972700000484, 8.226325169349999911 ) ) ;
#22754 = EDGE_CURVE ( 'NONE', #16297, #26053, #17167, .T. ) ;
#22755 = CARTESIAN_POINT ( 'NONE',  ( 21.51900322300193125, -37.41278966410947504, -7.708623769554239225 ) ) ;
#22756 = VERTEX_POINT ( 'NONE', #20471 ) ;
#22757 = ADVANCED_FACE ( 'NONE', ( #2416 ), #20178, .T. ) ;
#22758 = AXIS2_PLACEMENT_3D ( 'NONE', #7245, #5046, #18611 ) ;
#22759 = CARTESIAN_POINT ( 'NONE',  ( -32.61798276849999922, -80.00000022860000115, -22.71848792340000145 ) ) ;
#22760 = CARTESIAN_POINT ( 'NONE',  ( -21.01946775511974153, -64.01693695481982616, 12.95761361222880659 ) ) ;
#22761 = AXIS2_PLACEMENT_3D ( 'NONE', #15471, #24379, #4422 ) ;
#22762 = CARTESIAN_POINT ( 'NONE',  ( -32.47291160230000173, -74.11800272920001476, -21.73792012110000016 ) ) ;
#22763 = VERTEX_POINT ( 'NONE', #22813 ) ;
#22764 = CARTESIAN_POINT ( 'NONE',  ( 3.835404308829999831, -8.750000000000000000, 7.020660495120000455 ) ) ;
#22765 = CARTESIAN_POINT ( 'NONE',  ( 2.220446049249999745E-14, -11.00000000000000000, -50.00000000000000000 ) ) ;
#22766 = CARTESIAN_POINT ( 'NONE',  ( 7.674432201710000179, -64.79179280459999291, -23.81666465429999846 ) ) ;
#22767 = VERTEX_POINT ( 'NONE', #15645 ) ;
#22768 = CARTESIAN_POINT ( 'NONE',  ( -17.62778457210000127, -98.60479852289999769, 8.869694630919999767 ) ) ;
#22769 = CARTESIAN_POINT ( 'NONE',  ( -18.87648895869999777, -32.72716367869999488, 12.65371557960000004 ) ) ;
#22770 = CARTESIAN_POINT ( 'NONE',  ( 0.000000000000000000, -2.000000000000000000, 0.000000000000000000 ) ) ;
#22771 = CARTESIAN_POINT ( 'NONE',  ( -16.49390888960000368, -74.50000000000000000, 44.28897684009999836 ) ) ;
#22772 = CARTESIAN_POINT ( 'NONE',  ( -16.95867319479999935, -80.00000000000000000, 44.10460184009999551 ) ) ;
#22773 =( NAMED_UNIT ( * ) PLANE_ANGLE_UNIT ( ) SI_UNIT ( $, .RADIAN. ) );
#22774 = AXIS2_PLACEMENT_3D ( 'NONE', #10861, #291, #26490 ) ;
#22775 = AXIS2_PLACEMENT_3D ( 'NONE', #19443, #8360, #17265 ) ;
#22776 = CIRCLE ( 'NONE', #9273, 52.35000000000000142 ) ;
#22777 = VERTEX_POINT ( 'NONE', #13912 ) ;
#22778 = CARTESIAN_POINT ( 'NONE',  ( 11.15108825559999950, -100.9197081840000010, -10.94438638200000113 ) ) ;
#22779 = CIRCLE ( 'NONE', #16228, 20.64285714289999873 ) ;
#22780 = EDGE_CURVE ( 'NONE', #7941, #21723, #10963, .T. ) ;
#22781 = CARTESIAN_POINT ( 'NONE',  ( 10.14993553289999895, -99.56347846010000069, 14.32348655080000022 ) ) ;
#22782 = VERTEX_POINT ( 'NONE', #8793 ) ;
#22783 = CARTESIAN_POINT ( 'NONE',  ( -11.41039530250000134, -19.15810975349999978, -18.83652256670000114 ) ) ;
#22784 = EDGE_CURVE ( 'NONE', #9115, #25644, #10187, .T. ) ;
#22785 = DIRECTION ( 'NONE',  ( -0.7071067811865474617, 0.000000000000000000, -0.7071067811865474617 ) ) ;
#22786 = CARTESIAN_POINT ( 'NONE',  ( -7.478713340969999734, -101.1191090859999946, 14.48799200630000072 ) ) ;
#22787 = CARTESIAN_POINT ( 'NONE',  ( 9.564509902230000193, -57.40875702419999982, -23.52622212079999997 ) ) ;
#22788 = CARTESIAN_POINT ( 'NONE',  ( 8.173922678290001187, -37.03252586920000056, -21.52373127659999952 ) ) ;
#22789 = CARTESIAN_POINT ( 'NONE',  ( 7.579179873580000226, -101.3235621230000021, 13.98627925510000125 ) ) ;
#22790 = ORIENTED_EDGE ( 'NONE', *, *, #11670, .F. ) ;
#22791 = EDGE_CURVE ( 'NONE', #13203, #17392, #5375, .T. ) ;
#22792 = LINE ( 'NONE', #20154, #1624 ) ;
#22793 = CARTESIAN_POINT ( 'NONE',  ( -40.00000000000000000, -66.00000000000000000, 0.000000000000000000 ) ) ;
#22794 = CYLINDRICAL_SURFACE ( 'NONE', #27033, 7.999999999999998224 ) ;
#22795 = AXIS2_PLACEMENT_3D ( 'NONE', #193, #6874, #15740 ) ;
#22796 = CARTESIAN_POINT ( 'NONE',  ( -1.918209658487193048, -19.46987374641862445, -22.48175606853765274 ) ) ;
#22797 = CARTESIAN_POINT ( 'NONE',  ( 11.83254868180000052, -101.2490009469999990, -10.89135062169999912 ) ) ;
#22798 = CARTESIAN_POINT ( 'NONE',  ( -1.158253037809999997, -52.63055504180000099, -23.23212522879999753 ) ) ;
#22799 = CARTESIAN_POINT ( 'NONE',  ( -20.98832407942702005, -96.92941680200577537, -6.663699877346700440 ) ) ;
#22800 = VECTOR ( 'NONE', #14486, 1000.000000000000000 ) ;
#22801 = CIRCLE ( 'NONE', #6984, 39.25000000000000000 ) ;
#22802 = DIRECTION ( 'NONE',  ( 0.000000000000000000, -1.000000000000000000, 0.000000000000000000 ) ) ;
#22803 = CARTESIAN_POINT ( 'NONE',  ( 7.215414233289999757, -84.00000000000000000, 40.70731707320000226 ) ) ;
#22804 = CARTESIAN_POINT ( 'NONE',  ( 22.99217564430000138, -49.05622624239999396, -9.391640714770000287 ) ) ;
#22805 = CARTESIAN_POINT ( 'NONE',  ( 8.963581071913218068, -35.44265712976643812, -20.01429396093944391 ) ) ;
#22806 = CARTESIAN_POINT ( 'NONE',  ( 36.28164458690000060, -74.50000000000000000, -14.97346873880000118 ) ) ;
#22807 = VERTEX_POINT ( 'NONE', #27888 ) ;
#22808 = CARTESIAN_POINT ( 'NONE',  ( 36.70830950850000107, -75.00000021370000525, -14.75000047660000035 ) ) ;
#22809 = CARTESIAN_POINT ( 'NONE',  ( -32.66023294069999849, -74.45928706499999805, -21.85457041699999792 ) ) ;
#22810 = CARTESIAN_POINT ( 'NONE',  ( -22.50202996513547049, -79.94734758359761884, -32.71763195124997026 ) ) ;
#22811 = CARTESIAN_POINT ( 'NONE',  ( 22.48942068090000035, -95.85308664759999431, -0.6733658741689999561 ) ) ;
#22812 = CARTESIAN_POINT ( 'NONE',  ( 8.803829365699998633, -35.83655744470000570, -20.72386466589999898 ) ) ;
#22813 = CARTESIAN_POINT ( 'NONE',  ( 14.40601943769999949, -92.50000000000000000, 26.88338899689999906 ) ) ;
#22814 = CARTESIAN_POINT ( 'NONE',  ( -2.578307999469999778, -52.56313962710000709, -25.11373953509999879 ) ) ;
#22815 = DIRECTION ( 'NONE',  ( 0.4794255386042040046, 0.000000000000000000, 0.8775825618903722036 ) ) ;
#22816 = CARTESIAN_POINT ( 'NONE',  ( -17.55776206427488972, -93.39299082544175690, -21.35661493576082037 ) ) ;
#22817 = CIRCLE ( 'NONE', #21406, 9.999999999999998224 ) ;
#22818 = ADVANCED_FACE ( 'NONE', ( #5177 ), #14059, .T. ) ;
#22819 = EDGE_CURVE ( 'NONE', #15502, #24319, #3289, .T. ) ;
#22820 = ORIENTED_EDGE ( 'NONE', *, *, #12891, .F. ) ;
#22821 = CARTESIAN_POINT ( 'NONE',  ( -28.07036528529999941, -39.32601556110000018, -51.38245899869999533 ) ) ;
#22822 = CARTESIAN_POINT ( 'NONE',  ( -17.97171875919999806, -98.69238697859999832, -8.234156820420000855 ) ) ;
#22823 = ORIENTED_EDGE ( 'NONE', *, *, #5635, .T. ) ;
#22824 = ADVANCED_FACE ( 'NONE', ( #25298 ), #27478, .T. ) ;
#22825 = CARTESIAN_POINT ( 'NONE',  ( -30.49344753122725038, -92.49999999999998579, 0.6399496674373281735 ) ) ;
#22826 = EDGE_CURVE ( 'NONE', #14525, #26731, #18276, .T. ) ;
#22827 = CARTESIAN_POINT ( 'NONE',  ( 1.353583911619999998E-12, -74.50000000000000000, 1.342925770590000058E-12 ) ) ;
#22828 = CARTESIAN_POINT ( 'NONE',  ( -10.73983547945041472, -19.46468314325315419, 19.23955065568980771 ) ) ;
#22829 = DIRECTION ( 'NONE',  ( 0.8775825618903722036, 0.000000000000000000, -0.4794255386042041156 ) ) ;
#22830 = DIRECTION ( 'NONE',  ( 0.9295286103719527793, 0.000000000000000000, 0.3687499999999814260 ) ) ;
#22831 = CARTESIAN_POINT ( 'NONE',  ( -7.230685509177152248, -74.36482065499500038, -40.53346806266115010 ) ) ;
#22832 = CARTESIAN_POINT ( 'NONE',  ( -14.57413617419999952, -74.20280742140000996, 36.34762531509999661 ) ) ;
#22833 = CARTESIAN_POINT ( 'NONE',  ( -22.01499327390000005, -68.08608899289998817, 14.79936569140000024 ) ) ;
#22834 = CARTESIAN_POINT ( 'NONE',  ( -13.46276276179999876, -19.49999999970000175, 20.39865906480000035 ) ) ;
#22835 = ORIENTED_EDGE ( 'NONE', *, *, #4036, .F. ) ;
#22836 = CARTESIAN_POINT ( 'NONE',  ( -12.07668570139999886, -70.04473456239999507, -25.34381927969999992 ) ) ;
#22837 = DIRECTION ( 'NONE',  ( 1.000000000000000000, 0.000000000000000000, 0.000000000000000000 ) ) ;
#22838 = CARTESIAN_POINT ( 'NONE',  ( 0.000000000000000000, -15.49689110870000164, 0.000000000000000000 ) ) ;
#22839 = CARTESIAN_POINT ( 'NONE',  ( -13.18661234450000030, -92.50000000000000000, 26.85581265420000108 ) ) ;
#22840 = AXIS2_PLACEMENT_3D ( 'NONE', #26431, #23957, #3991 ) ;
#22841 = CARTESIAN_POINT ( 'NONE',  ( 15.98230758980000132, -101.4309749570000037, 2.416262475850000424 ) ) ;
#22842 = ORIENTED_EDGE ( 'NONE', *, *, #12208, .F. ) ;
#22843 = VECTOR ( 'NONE', #21579, 1000.000000000000000 ) ;
#22844 = AXIS2_PLACEMENT_3D ( 'NONE', #27687, #12344, #25628 ) ;
#22845 = EDGE_CURVE ( 'NONE', #16409, #10454, #17318, .T. ) ;
#22846 = EDGE_LOOP ( 'NONE', ( #319, #23493, #26614, #22436 ) ) ;
#22847 = CARTESIAN_POINT ( 'NONE',  ( -1.450351827910000058, -57.47122586340000083, -23.51019412459999813 ) ) ;
#22848 = CARTESIAN_POINT ( 'NONE',  ( -3.552756184370000181, -98.29702512609999587, 18.77134648699999886 ) ) ;
#22849 = CARTESIAN_POINT ( 'NONE',  ( 5.602941559059999577, -93.28216931219999708, 26.66162101379999783 ) ) ;
#22850 = ORIENTED_EDGE ( 'NONE', *, *, #4474, .T. ) ;
#22851 = EDGE_CURVE ( 'NONE', #3056, #27919, #5235, .T. ) ;
#22852 = CARTESIAN_POINT ( 'NONE',  ( -11.25326567110000120, -94.84395216780001192, -20.59896464009999661 ) ) ;
#22853 = ORIENTED_EDGE ( 'NONE', *, *, #27194, .F. ) ;
#22854 = DIRECTION ( 'NONE',  ( 0.4794255386042041156, 0.000000000000000000, 0.8775825618903720926 ) ) ;
#22855 = CARTESIAN_POINT ( 'NONE',  ( 21.92361644269999843, -37.64807918350000193, -8.681080957089999828 ) ) ;
#22856 = CARTESIAN_POINT ( 'NONE',  ( 47.16788169050000334, -74.59616887820000386, -1.399136062990000040 ) ) ;
#22857 = EDGE_LOOP ( 'NONE', ( #156, #20118, #3598, #6825, #22124, #12852, #23855, #24227, #10615, #17450, #10998, #230, #28778, #23134, #23546, #6329 ) ) ;
#22858 = CIRCLE ( 'NONE', #25190, 10.00000000000000000 ) ;
#22859 = CARTESIAN_POINT ( 'NONE',  ( 7.208933142638366043, -73.58711170886618902, -39.22862632807101591 ) ) ;
#22860 = CARTESIAN_POINT ( 'NONE',  ( 0.000000000000000000, -92.50000000000000000, 29.91857981989999971 ) ) ;
#22861 = CIRCLE ( 'NONE', #18187, 0.4999999999999967804 ) ;
#22862 = CIRCLE ( 'NONE', #25195, 9.500000000000001776 ) ;
#22863 = CARTESIAN_POINT ( 'NONE',  ( 23.50166587798742412, -64.58097839926523420, 10.73601817129581981 ) ) ;
#22864 = CARTESIAN_POINT ( 'NONE',  ( -1.546569514440000015, -66.56254540410000686, -25.78631783400000188 ) ) ;
#22865 = CARTESIAN_POINT ( 'NONE',  ( -16.35365950510000133, -70.21389208120000092, 23.31707131299999958 ) ) ;
#22866 = VERTEX_POINT ( 'NONE', #12004 ) ;
#22867 = DIRECTION ( 'NONE',  ( 0.000000000000000000, 1.000000000000000000, 0.000000000000000000 ) ) ;
#22868 = CARTESIAN_POINT ( 'NONE',  ( -2.587281614239999694, -58.59418584699999855, -25.28476954130000109 ) ) ;
#22869 = CARTESIAN_POINT ( 'NONE',  ( 23.68479145319999901, -60.57882006589999691, 0.02928418074640000077 ) ) ;
#22870 = CARTESIAN_POINT ( 'NONE',  ( -22.13232332860000184, -74.50000000000000000, -32.73892504640000567 ) ) ;
#22871 = VERTEX_POINT ( 'NONE', #5602 ) ;
#22872 = CARTESIAN_POINT ( 'NONE',  ( -11.32307664130000013, -92.50000000000000000, 9.421136869679999748 ) ) ;
#22873 = CARTESIAN_POINT ( 'NONE',  ( -7.377395436790557426, -73.99965292983208087, 39.26711817943528615 ) ) ;
#22874 = CARTESIAN_POINT ( 'NONE',  ( 36.46922389885823890, -74.05666263691847462, -14.08207577745026562 ) ) ;
#22875 = VERTEX_POINT ( 'NONE', #14485 ) ;
#22876 = CARTESIAN_POINT ( 'NONE',  ( -13.10651597679999902, -92.87496451630001104, -23.83817055480000136 ) ) ;
#22877 = EDGE_CURVE ( 'NONE', #22004, #25894, #3008, .T. ) ;
#22878 = CARTESIAN_POINT ( 'NONE',  ( 23.74633046639999989, -64.47177090210000472, 10.70095004270000061 ) ) ;
#22879 = CARTESIAN_POINT ( 'NONE',  ( -39.03811165380000148, -65.41419836839999391, -2.576072437790000169 ) ) ;
#22880 = CARTESIAN_POINT ( 'NONE',  ( 16.63653260355367891, -100.1406256088351796, 4.325926551192202929 ) ) ;
#22881 = CARTESIAN_POINT ( 'NONE',  ( 13.82610735156381487, -99.76647888977575462, -10.42913651524955121 ) ) ;
#22882 = ORIENTED_EDGE ( 'NONE', *, *, #13377, .T. ) ;
#22883 = CARTESIAN_POINT ( 'NONE',  ( -1.315109685649999971, -92.50000000000000000, -30.47163412939999816 ) ) ;
#22884 = CONICAL_SURFACE ( 'NONE', #27051, 55.67692378859999280, 1.047197551199999799 ) ;
#22885 = AXIS2_PLACEMENT_3D ( 'NONE', #15124, #8584, #12798 ) ;
#22886 = TOROIDAL_SURFACE ( 'NONE', #12602, 5.500000000000000000, 0.5000000000000000000 ) ;
#22887 = B_SPLINE_CURVE_WITH_KNOTS ( 'NONE', 3,
 ( #109, #20486, #2582, #13928 ),
 .UNSPECIFIED., .F., .F.,
 ( 4, 4 ),
 ( 0.000000000000000000, 1.000000000000000000 ),
 .UNSPECIFIED. ) ;
#22888 = PRODUCT_CONTEXT ( 'NONE', #15339, 'mechanical' ) ;
#22889 = CARTESIAN_POINT ( 'NONE',  ( -12.23534022509999986, -63.58862135099999335, -21.26946117359999988 ) ) ;
#22890 = EDGE_CURVE ( 'NONE', #5527, #21711, #16139, .T. ) ;
#22891 = CARTESIAN_POINT ( 'NONE',  ( 23.96368475870000125, -93.00000000000000000, 8.717328305520000598 ) ) ;
#22892 = CARTESIAN_POINT ( 'NONE',  ( -37.60355029590000697, -74.00000000000000000, -9.356041104380000917 ) ) ;
#22893 = ORIENTED_EDGE ( 'NONE', *, *, #23477, .T. ) ;
#22894 = DIRECTION ( 'NONE',  ( 0.7071067811865475727, 0.000000000000000000, 0.7071067811865475727 ) ) ;
#22895 = CARTESIAN_POINT ( 'NONE',  ( 47.14681262259601624, -74.43066600419328438, -1.228599301886279083 ) ) ;
#22896 = EDGE_LOOP ( 'NONE', ( #13714, #8767, #22308, #21371 ) ) ;
#22897 = CARTESIAN_POINT ( 'NONE',  ( 20.49588873660000132, -52.63280639840000674, 10.85734681379999955 ) ) ;
#22898 = CARTESIAN_POINT ( 'NONE',  ( -2.578307999469999778, -45.73899999920000425, -25.11373953509999879 ) ) ;
#22899 = EDGE_LOOP ( 'NONE', ( #21945, #1499, #14535, #5774, #13067, #26443 ) ) ;
#22900 = DIRECTION ( 'NONE',  ( 0.000000000000000000, 1.000000000000000000, 0.000000000000000000 ) ) ;
#22901 = CIRCLE ( 'NONE', #17764, 30.50000000000000000 ) ;
#22902 = CARTESIAN_POINT ( 'NONE',  ( -0.5380693342220000952, -55.86335041469999396, -23.29854462139999782 ) ) ;
#22903 = CARTESIAN_POINT ( 'NONE',  ( -10.54477336451839165, -19.46993844407590402, -19.95170415067392256 ) ) ;
#22904 = DIRECTION ( 'NONE',  ( 1.000000000000000000, 0.000000000000000000, 0.000000000000000000 ) ) ;
#22905 = CARTESIAN_POINT ( 'NONE',  ( -10.93437413680000070, -19.50000027030000282, -21.85842452360000010 ) ) ;
#22906 = AXIS2_PLACEMENT_3D ( 'NONE', #5923, #26330, #3889 ) ;
#22907 = CARTESIAN_POINT ( 'NONE',  ( 9.575769126168214740, -58.58842956003458369, -23.55923831042092331 ) ) ;
#22908 = ORIENTED_EDGE ( 'NONE', *, *, #21916, .F. ) ;
#22909 = AXIS2_PLACEMENT_3D ( 'NONE', #4655, #17626, #2487 ) ;
#22910 = CARTESIAN_POINT ( 'NONE',  ( -32.37889788280000403, -80.19684081550001054, -22.28728604720000206 ) ) ;
#22911 = CARTESIAN_POINT ( 'NONE',  ( 0.000000000000000000, -24.50000000000000000, 0.000000000000000000 ) ) ;
#22912 = CARTESIAN_POINT ( 'NONE',  ( 0.000000000000000000, -91.50000000000000000, 0.000000000000000000 ) ) ;
#22913 = VERTEX_POINT ( 'NONE', #1946 ) ;
#22914 = DIRECTION ( 'NONE',  ( 0.000000000000000000, -1.000000000000000000, 0.000000000000000000 ) ) ;
#22915 = FACE_OUTER_BOUND ( 'NONE', #20144, .T. ) ;
#22916 = CARTESIAN_POINT ( 'NONE',  ( 0.000000000000000000, -19.40000000000000213, 0.000000000000000000 ) ) ;
#22917 = EDGE_LOOP ( 'NONE', ( #18372, #3449, #20964, #3239 ) ) ;
#22918 = CARTESIAN_POINT ( 'NONE',  ( -18.24886543000000216, -94.80026553199999739, 16.23660559380000024 ) ) ;
#22919 = CARTESIAN_POINT ( 'NONE',  ( -18.99796627190000109, -26.09744228899999996, 11.61130727839999821 ) ) ;
#22920 = DIRECTION ( 'NONE',  ( -0.6710129359900831592, 0.000000000000000000, 0.7414456417930908039 ) ) ;
#22921 = DIRECTION ( 'NONE',  ( 0.000000000000000000, 1.000000000000000000, 0.000000000000000000 ) ) ;
#22922 = CARTESIAN_POINT ( 'NONE',  ( 22.95932757850000172, -57.43039251880000506, -9.307781678039997786 ) ) ;
#22923 = EDGE_CURVE ( 'NONE', #1616, #23041, #2966, .T. ) ;
#22924 = TOROIDAL_SURFACE ( 'NONE', #26622, 15.50000000000000000, 0.5000000000000000000 ) ;
#22925 = CARTESIAN_POINT ( 'NONE',  ( 26.67136988580000079, -64.89183635380001647, 1.586600751119999764 ) ) ;
#22926 = ADVANCED_FACE ( 'NONE', ( #23655 ), #10503, .F. ) ;
#22927 = AXIS2_PLACEMENT_3D ( 'NONE', #20318, #24703, #2265 ) ;
#22928 = EDGE_CURVE ( 'NONE', #28111, #9851, #9397, .T. ) ;
#22929 = ORIENTED_EDGE ( 'NONE', *, *, #9377, .F. ) ;
#22930 = CARTESIAN_POINT ( 'NONE',  ( 20.40611818609999872, -54.57118573399999661, 11.16247708059999866 ) ) ;
#22931 = DIRECTION ( 'NONE',  ( 1.000000000000000000, 0.000000000000000000, 0.000000000000000000 ) ) ;
#22932 = CARTESIAN_POINT ( 'NONE',  ( 21.78580818670000241, -37.64222968090000165, -8.476164596309999411 ) ) ;
#22933 = CARTESIAN_POINT ( 'NONE',  ( 17.49193124830000201, -96.07623110170000302, 14.96946685699999868 ) ) ;
#22934 = VERTEX_POINT ( 'NONE', #8203 ) ;
#22935 = FACE_OUTER_BOUND ( 'NONE', #26852, .T. ) ;
#22936 = CARTESIAN_POINT ( 'NONE',  ( 16.54057195469999897, -94.89197151650000706, 16.94454422099999746 ) ) ;
#22937 = B_SPLINE_SURFACE_WITH_KNOTS ( 'NONE', 5, 5, ( 
 ( #9051, #2220, #17955, #19978, #6742, #4105, #6590, #24363, #17374 ),
 ( #6884, #51, #4404, #26268, #24506, #13420, #2370, #12976, #1939 ),
 ( #19691, #17517, #26404, #24220, #4254, #25101, #5283, #645, #11964 ),
 ( #9779, #5135, #3111, #498, #14170, #20280, #9192, #27143, #18693 ),
 ( #27588, #13869, #5422, #14016, #937, #7629, #16494, #25397, #14306 ),
 ( #9495, #2964, #9346, #23201, #20878, #347, #22922, #20737, #11823 ) ),
 .UNSPECIFIED., .F., .F., .F.,
 ( 6, 6 ),
 ( 6, 3, 6 ),
 ( 26.76256113009999993, 37.28868011619999834 ),
 ( 0.000000000000000000, 1.000000000000000000, 2.000000000000000000 ),
 .UNSPECIFIED. ) ;
#22938 = PLANE ( 'NONE',  #23288 ) ;
#22939 = CARTESIAN_POINT ( 'NONE',  ( -10.46188072746246434, -93.89463536436431923, -23.23764647000281869 ) ) ;
#22940 = DIRECTION ( 'NONE',  ( 1.000000000000000000, 0.000000000000000000, 5.788992577199999305E-17 ) ) ;
#22941 = CARTESIAN_POINT ( 'NONE',  ( 7.235323095100000046, -101.2527939679999918, 13.36104842480000165 ) ) ;
#22942 = ORIENTED_EDGE ( 'NONE', *, *, #18056, .T. ) ;
#22943 = FACE_OUTER_BOUND ( 'NONE', #3107, .T. ) ;
#22944 = VECTOR ( 'NONE', #1398, 1000.000000000000000 ) ;
#22945 = CARTESIAN_POINT ( 'NONE',  ( 23.33156623710000233, -18.50000000000000000, 2.512796439940000237 ) ) ;
#22946 = CARTESIAN_POINT ( 'NONE',  ( 11.64683525529999919, -98.24904979019999018, -15.38395215939999972 ) ) ;
#22947 = VERTEX_POINT ( 'NONE', #17091 ) ;
#22948 = PLANE ( 'NONE',  #13179 ) ;
#22949 = CARTESIAN_POINT ( 'NONE',  ( 0.000000000000000000, -101.1889999979999999, 0.000000000000000000 ) ) ;
#22950 = AXIS2_PLACEMENT_3D ( 'NONE', #4045, #27967, #16749 ) ;
#22951 = CARTESIAN_POINT ( 'NONE',  ( -2.567353809430000133, -52.57401960330000179, -24.80239345940000106 ) ) ;
#22952 = B_SPLINE_CURVE_WITH_KNOTS ( 'NONE', 5,
 ( #22834, #5343, #13933, #11735, #5043, #11885, #25165, #16690, #7690 ),
 .UNSPECIFIED., .F., .F.,
 ( 6, 3, 6 ),
 ( -86.65534111079999491, -83.85288688999999351, -33.01978394879999712 ),
 .UNSPECIFIED. ) ;
#22953 = CARTESIAN_POINT ( 'NONE',  ( 14.16035994550885313, -95.68935540834247888, 17.33364939168795971 ) ) ;
#22954 = CARTESIAN_POINT ( 'NONE',  ( -7.325370793560000315, -45.73899999920000425, -24.94672208400000102 ) ) ;
#22955 = CARTESIAN_POINT ( 'NONE',  ( 11.86655840719999944, -101.3150700380000018, -11.10431293650000129 ) ) ;
#22956 = CARTESIAN_POINT ( 'NONE',  ( 21.56931441200000421, -36.56979899360000275, -6.850353673489999906 ) ) ;
#22957 = DIRECTION ( 'NONE',  ( 0.000000000000000000, 1.000000000000000000, 0.000000000000000000 ) ) ;
#22958 = CARTESIAN_POINT ( 'NONE',  ( -29.17304402409999753, -10.00000000000000000, -53.40089889099999709 ) ) ;
#22959 = ORIENTED_EDGE ( 'NONE', *, *, #2317, .F. ) ;
#22960 = EDGE_CURVE ( 'NONE', #13357, #23740, #13341, .T. ) ;
#22961 = CARTESIAN_POINT ( 'NONE',  ( -32.69645380010000224, -74.50000000299999670, -21.71458329220000039 ) ) ;
#22962 = CARTESIAN_POINT ( 'NONE',  ( -32.66023292159999869, -79.50000000000062528, -21.85457041760000152 ) ) ;
#22963 = EDGE_CURVE ( 'NONE', #11437, #9289, #3964, .T. ) ;
#22964 = CARTESIAN_POINT ( 'NONE',  ( -13.78120180950000062, -66.79737695549998477, 22.18107486459999933 ) ) ;
#22965 = CARTESIAN_POINT ( 'NONE',  ( 21.19870159919999963, -35.15967237200000284, -7.969913383650000682 ) ) ;
#22966 = CARTESIAN_POINT ( 'NONE',  ( 36.75261502460000429, -80.49999978700000725, -13.77875165610000074 ) ) ;
#22967 = AXIS2_PLACEMENT_3D ( 'NONE', #18669, #6085, #12632 ) ;
#22968 = CIRCLE ( 'NONE', #24824, 3.500000000000003109 ) ;
#22969 = DIRECTION ( 'NONE',  ( 0.4151946956541399669, 0.5000000000001689759, 0.7600087925152558821 ) ) ;
#22970 = DIRECTION ( 'NONE',  ( 0.8531997950690719534, 0.000000000000000000, -0.5215842306800441142 ) ) ;
#22971 = ORIENTED_EDGE ( 'NONE', *, *, #10407, .F. ) ;
#22972 = CARTESIAN_POINT ( 'NONE',  ( 37.60355029590000697, -84.50000000000000000, 9.356041104380000917 ) ) ;
#22973 = CARTESIAN_POINT ( 'NONE',  ( 6.114061450880000415, -92.50000000000000000, -13.40104985119999981 ) ) ;
#22974 = EDGE_LOOP ( 'NONE', ( #798, #2344, #9470, #21666 ) ) ;
#22975 = CARTESIAN_POINT ( 'NONE',  ( 13.12517053680000068, -111.0000000000000000, 27.53143473160000099 ) ) ;
#22976 = CARTESIAN_POINT ( 'NONE',  ( 0.2593320631483060357, -101.4728631013045970, -16.13356699571328789 ) ) ;
#22977 = FACE_OUTER_BOUND ( 'NONE', #5942, .T. ) ;
#22978 = CARTESIAN_POINT ( 'NONE',  ( -12.09704001540000107, -74.00000000000000000, 47.10905722069999513 ) ) ;
#22979 = CARTESIAN_POINT ( 'NONE',  ( 23.76251265679999847, -94.45168166330000759, -7.425192885069999527 ) ) ;
#22980 = CARTESIAN_POINT ( 'NONE',  ( -11.25326567110000120, -94.84395216780001192, -20.59896464009999661 ) ) ;
#22981 = CARTESIAN_POINT ( 'NONE',  ( 23.76679749976556266, -92.71619979444686521, -19.11516032664452780 ) ) ;
#22982 = VERTEX_POINT ( 'NONE', #19987 ) ;
#22983 = CARTESIAN_POINT ( 'NONE',  ( -13.09652604470000092, -71.22348525710000899, -24.69511647019999856 ) ) ;
#22984 = DIRECTION ( 'NONE',  ( 0.4794255386042036715, 0.000000000000000000, 0.8775825618903724257 ) ) ;
#22985 = DIRECTION ( 'NONE',  ( 0.000000000000000000, 1.000000000000000000, 0.000000000000000000 ) ) ;
#22986 = CIRCLE ( 'NONE', #1573, 16.00000000000000000 ) ;
#22987 = CARTESIAN_POINT ( 'NONE',  ( 3.907985046679999924E-15, -73.50000000000000000, -40.00000000000000000 ) ) ;
#22988 = CARTESIAN_POINT ( 'NONE',  ( -42.25000000000000000, -65.63577453799999262, 0.7216878364880000563 ) ) ;
#22989 = VERTEX_POINT ( 'NONE', #4261 ) ;
#22990 = ADVANCED_FACE ( 'NONE', ( #57 ), #21504, .F. ) ;
#22991 = ORIENTED_EDGE ( 'NONE', *, *, #21568, .T. ) ;
#22992 = ADVANCED_FACE ( 'NONE', ( #17816 ), #8928, .F. ) ;
#22993 = CARTESIAN_POINT ( 'NONE',  ( -0.8479729843809999945, -57.47815889169999792, -23.34776883199999986 ) ) ;
#22994 = VECTOR ( 'NONE', #20646, 1000.000000000000000 ) ;
#22995 = CYLINDRICAL_SURFACE ( 'NONE', #14407, 0.7499999999999996669 ) ;
#22996 = CARTESIAN_POINT ( 'NONE',  ( 1.316321141829999819, -94.80026165740000010, 24.39090473970000161 ) ) ;
#22997 = EDGE_LOOP ( 'NONE', ( #6911, #14607, #26706 ) ) ;
#22998 = CARTESIAN_POINT ( 'NONE',  ( -11.27245849040000003, -95.14589738820001230, -21.35309096379999971 ) ) ;
#22999 = CARTESIAN_POINT ( 'NONE',  ( -7.215414233289999757, -84.00000000000000000, -40.70731707320000226 ) ) ;
#23000 = CARTESIAN_POINT ( 'NONE',  ( -18.94992598540000017, -92.68283714880000446, -20.51038952960000117 ) ) ;
#23001 = CARTESIAN_POINT ( 'NONE',  ( 4.146788479588165544, -93.04141874247781629, 28.17739296888928280 ) ) ;
#23002 = EDGE_LOOP ( 'NONE', ( #15371, #13797 ) ) ;
#23003 = AXIS2_PLACEMENT_3D ( 'NONE', #27240, #27099, #20689 ) ;
#23004 = CARTESIAN_POINT ( 'NONE',  ( 3.166345171159999694, -93.00000000000000000, -25.30265318609999881 ) ) ;
#23005 = CARTESIAN_POINT ( 'NONE',  ( 21.75659477429999811, -92.50000000000000000, -13.30039788230000042 ) ) ;
#23006 = VERTEX_POINT ( 'NONE', #13579 ) ;
#23007 = EDGE_CURVE ( 'NONE', #27814, #12485, #1969, .T. ) ;
#23008 = CARTESIAN_POINT ( 'NONE',  ( 7.491164759823046637, -101.2404586314123520, 13.91530727530272493 ) ) ;
#23009 = CARTESIAN_POINT ( 'NONE',  ( -0.8905213842159999116, -65.59529275500000267, -25.37156472860000278 ) ) ;
#23010 = DIRECTION ( 'NONE',  ( 0.4794255386042040601, 0.000000000000000000, 0.8775825618903720926 ) ) ;
#23011 = ORIENTED_EDGE ( 'NONE', *, *, #19283, .T. ) ;
#23012 = CARTESIAN_POINT ( 'NONE',  ( -14.59815773840000830, -79.49999996002311775, 36.63377407710000000 ) ) ;
#23013 = CIRCLE ( 'NONE', #8098, 57.75000000000000000 ) ;
#23014 = CARTESIAN_POINT ( 'NONE',  ( -16.03245889869999985, -100.9307694150000003, 3.138388912410000398 ) ) ;
#23015 = CARTESIAN_POINT ( 'NONE',  ( 24.14381995990000007, -62.06858034060000762, 0.2946074132029999904 ) ) ;
#23016 = CARTESIAN_POINT ( 'NONE',  ( 19.47627435319999734, -35.29258001769999709, -8.987105447939999436 ) ) ;
#23017 = EDGE_LOOP ( 'NONE', ( #24671, #12583, #19905, #4707 ) ) ;
#23018 = CIRCLE ( 'NONE', #8542, 3.499999999999999556 ) ;
#23019 = CARTESIAN_POINT ( 'NONE',  ( -1.001103094699999918, -19.15716910929999628, -22.00374779629999722 ) ) ;
#23020 = CARTESIAN_POINT ( 'NONE',  ( 36.50961708847058418, -74.07907867045096850, -14.14048807786333661 ) ) ;
#23021 = EDGE_LOOP ( 'NONE', ( #17863, #22010, #13888, #27238 ) ) ;
#23023 = EDGE_CURVE ( 'NONE', #22254, #25894, #16824, .T. ) ;
#23022 = CARTESIAN_POINT ( 'NONE',  ( -11.53828505259999915, -18.50000000000000000, 18.05193266499999893 ) ) ;
#23024 = CARTESIAN_POINT ( 'NONE',  ( 23.67927593730000169, -62.35648592489999942, 10.61505170350000071 ) ) ;
#23025 = CARTESIAN_POINT ( 'NONE',  ( 8.791129346259999977, -34.94311270309999884, -20.42416734049999860 ) ) ;
#23026 = CARTESIAN_POINT ( 'NONE',  ( 15.78742501808848608, -101.2637735887499986, 4.048283812879304833 ) ) ;
#23027 = CARTESIAN_POINT ( 'NONE',  ( 0.000000000000000000, -39.50000000000000000, 0.000000000000000000 ) ) ;
#23028 = VERTEX_POINT ( 'NONE', #2377 ) ;
#23029 = CIRCLE ( 'NONE', #28587, 7.250000000000000000 ) ;
#23030 = DIRECTION ( 'NONE',  ( 0.9295286103719527793, 0.000000000000000000, 0.3687499999999814260 ) ) ;
#23031 = CARTESIAN_POINT ( 'NONE',  ( -11.20518065289999932, -58.91551295370000219, -21.78293632669999980 ) ) ;
#23032 = AXIS2_PLACEMENT_3D ( 'NONE', #7114, #4332, #18326 ) ;
#23033 = CARTESIAN_POINT ( 'NONE',  ( 19.97576656849999921, -17.00000000000000000, -19.97576656849999921 ) ) ;
#23034 = CYLINDRICAL_SURFACE ( 'NONE', #9672, 57.74999999999999289 ) ;
#23035 = ORIENTED_EDGE ( 'NONE', *, *, #18472, .T. ) ;
#23036 = CARTESIAN_POINT ( 'NONE',  ( -41.75000000000000000, -65.17124718639999514, -2.640283750799999662 ) ) ;
#23037 = EDGE_LOOP ( 'NONE', ( #6841, #9020, #28638, #24207 ) ) ;
#23038 = CONICAL_SURFACE ( 'NONE', #24876, 58.55000000000003979, 0.7853981633970000820 ) ;
#23039 = CARTESIAN_POINT ( 'NONE',  ( -11.09899533129999938, -34.67032517180000895, 19.64911088110000037 ) ) ;
#23040 = CARTESIAN_POINT ( 'NONE',  ( -6.000841078150000563, -101.4334236450000049, 14.90466326349999981 ) ) ;
#23041 = VERTEX_POINT ( 'NONE', #13131 ) ;
#23042 = DIRECTION ( 'NONE',  ( 0.000000000000000000, -1.000000000000000000, 0.000000000000000000 ) ) ;
#23043 = DIRECTION ( 'NONE',  ( 0.000000000000000000, 1.000000000000000000, 0.000000000000000000 ) ) ;
#23044 = EDGE_CURVE ( 'NONE', #10772, #21528, #19591, .T. ) ;
#23045 = B_SPLINE_CURVE_WITH_KNOTS ( 'NONE', 5,
 ( #5806, #10433, #15093, #12766, #21677, #10565 ),
 .UNSPECIFIED., .F., .F.,
 ( 6, 6 ),
 ( 0.000000000000000000, 1.000000000000000000 ),
 .UNSPECIFIED. ) ;
#23046 = ORIENTED_EDGE ( 'NONE', *, *, #27912, .F. ) ;
#23047 = EDGE_CURVE ( 'NONE', #5390, #20659, #25706, .T. ) ;
#23048 = CARTESIAN_POINT ( 'NONE',  ( 39.07223452259999874, -73.87252278319999732, 7.323177335930000531 ) ) ;
#23049 = CARTESIAN_POINT ( 'NONE',  ( -20.20035200647939888, -94.89195677473493618, 12.35537660001062754 ) ) ;
#23050 = CARTESIAN_POINT ( 'NONE',  ( 0.000000000000000000, -19.70310889130000120, 0.000000000000000000 ) ) ;
#23051 = CARTESIAN_POINT ( 'NONE',  ( 26.61465604159999998, -68.28989644159999273, 0.1578853838729999959 ) ) ;
#23052 = DIRECTION ( 'NONE',  ( 1.000000000000000000, 0.000000000000000000, 0.000000000000000000 ) ) ;
#23053 = VERTEX_POINT ( 'NONE', #26557 ) ;
#23054 = CARTESIAN_POINT ( 'NONE',  ( -32.73892504640000567, -79.50000000000000000, -22.13232332860000184 ) ) ;
#23055 = CARTESIAN_POINT ( 'NONE',  ( 18.35053352010000083, -98.58303758080000989, 3.544495826009999906 ) ) ;
#23056 = DIRECTION ( 'NONE',  ( 0.4794255386042041156, 0.000000000000000000, 0.8775825618903722036 ) ) ;
#23057 = CARTESIAN_POINT ( 'NONE',  ( -27.68682485439999752, -28.10000000000000142, -50.68039294919999804 ) ) ;
#23058 = ORIENTED_EDGE ( 'NONE', *, *, #26319, .T. ) ;
#23059 = CONICAL_SURFACE ( 'NONE', #28612, 55.67692378859999280, 1.047197551199999799 ) ;
#23060 = DIRECTION ( 'NONE',  ( 0.000000000000000000, 1.000000000000000000, 0.000000000000000000 ) ) ;
#23061 = CARTESIAN_POINT ( 'NONE',  ( -16.14562817639999892, -111.0000000000000000, 4.458832895280000486 ) ) ;
#23062 = CARTESIAN_POINT ( 'NONE',  ( 22.96745989159999723, -18.50000000000000000, 9.091461454319999191 ) ) ;
#23063 = ORIENTED_EDGE ( 'NONE', *, *, #8435, .T. ) ;
#23064 = CARTESIAN_POINT ( 'NONE',  ( -16.63714921780000111, -99.82961947799999791, 6.686300942209999931 ) ) ;
#23065 = VECTOR ( 'NONE', #9375, 1000.000000000000000 ) ;
#23066 = CARTESIAN_POINT ( 'NONE',  ( 0.3872054374930000153, -99.92967571559999840, -17.35614705709999939 ) ) ;
#23067 = CARTESIAN_POINT ( 'NONE',  ( 0.000000000000000000, -84.00000000000000000, 0.000000000000000000 ) ) ;
#23068 = CARTESIAN_POINT ( 'NONE',  ( 30.91973185770000043, -72.00365067099998839, -22.05221014440000005 ) ) ;
#23069 = CARTESIAN_POINT ( 'NONE',  ( -0.1779554536940000098, -101.6484611540000031, -15.99901033990000165 ) ) ;
#23070 = ORIENTED_EDGE ( 'NONE', *, *, #17966, .F. ) ;
#23071 = CARTESIAN_POINT ( 'NONE',  ( -39.40310785696919282, -73.65029154571925574, -7.225850277565577073 ) ) ;
#23072 = CIRCLE ( 'NONE', #22605, 5.500000000000000000 ) ;
#23073 = CARTESIAN_POINT ( 'NONE',  ( 21.59677465600000090, -37.21264878210000404, -8.299693975220000297 ) ) ;
#23074 = DIRECTION ( 'NONE',  ( 0.000000000000000000, 1.000000000000000000, 0.000000000000000000 ) ) ;
#23075 = ORIENTED_EDGE ( 'NONE', *, *, #2412, .T. ) ;
#23076 = CARTESIAN_POINT ( 'NONE',  ( 8.185346967789998374, -111.0000000000000000, 14.03998109830000018 ) ) ;
#23077 = CARTESIAN_POINT ( 'NONE',  ( -11.41594931139999858, -19.46510050329999686, -18.84569254350000023 ) ) ;
#23078 = EDGE_CURVE ( 'NONE', #3331, #8764, #4283, .T. ) ;
#23079 = CARTESIAN_POINT ( 'NONE',  ( 45.84677419350000349, -80.50000000000000000, -4.286925650119999709 ) ) ;
#23080 = CARTESIAN_POINT ( 'NONE',  ( 6.308882621530000456, -93.00000000000000000, -29.19167084780000110 ) ) ;
#23081 = B_SPLINE_CURVE_WITH_KNOTS ( 'NONE', 3,
 ( #15279, #24201, #4234, #13108, #22020, #19814, #23629, #12530, #14730, #18231, #2653, #6572, #185, #24346, #26981, #2203, #26835, #6724 ),
 .UNSPECIFIED., .F., .F.,
 ( 4, 2, 2, 2, 1, 1, 1, 1, 2, 2, 4 ),
 ( 0.000000000000000000, 0.2499999999999109601, 0.3749999999998656630, 0.4374999999998440137, 0.4687499999998328004, 0.4843749999998279154, 0.4921874999998258615, 0.4960937499998256395, 0.4980468749998255285, 0.4999999999998253619, 1.000000000000000000 ),
 .UNSPECIFIED. ) ;
#23082 = CARTESIAN_POINT ( 'NONE',  ( 9.414867375249999171, -40.68175103339999765, -23.05516474710000097 ) ) ;
#23083 = CARTESIAN_POINT ( 'NONE',  ( 7.577553826990000019, -101.4254869589999970, 14.05661196390000001 ) ) ;
#23084 = ORIENTED_EDGE ( 'NONE', *, *, #8164, .F. ) ;
#23085 = ADVANCED_FACE ( 'NONE', ( #22186 ), #2226, .T. ) ;
#23086 = CARTESIAN_POINT ( 'NONE',  ( -28.63163567490000005, -92.51556042380001088, -2.601810723099999834 ) ) ;
#23087 = CARTESIAN_POINT ( 'NONE',  ( 11.63343543059999874, -100.9405345029999950, -10.90407306190000014 ) ) ;
#23088 = VERTEX_POINT ( 'NONE', #14452 ) ;
#23089 = CARTESIAN_POINT ( 'NONE',  ( -0.5856137342820000313, -19.46510053389999939, -22.02591827759999887 ) ) ;
#23090 = EDGE_CURVE ( 'NONE', #26844, #25324, #24289, .T. ) ;
#23091 = CARTESIAN_POINT ( 'NONE',  ( 11.44042105569999990, -101.2530993000000024, -9.998588429439999814 ) ) ;
#23092 = CARTESIAN_POINT ( 'NONE',  ( -1.203638492820000128, -32.73099401719999690, -22.54375384349999933 ) ) ;
#23093 = CYLINDRICAL_SURFACE ( 'NONE', #10269, 39.24999999999998579 ) ;
#23094 = EDGE_CURVE ( 'NONE', #14431, #14119, #7606, .T. ) ;
#23095 = CARTESIAN_POINT ( 'NONE',  ( 1.598721155460000041E-15, -84.50000000000000000, 6.905587213169999654E-15 ) ) ;
#23096 = CARTESIAN_POINT ( 'NONE',  ( 20.36016146999999776, -74.00000000000000000, -32.97008227039999895 ) ) ;
#23097 = CARTESIAN_POINT ( 'NONE',  ( 23.05516474710000097, -40.68175103160000106, -9.414867375240000058 ) ) ;
#23098 = DIRECTION ( 'NONE',  ( 0.9995627462972740407, 0.000000000000000000, -0.02956883857460809381 ) ) ;
#23099 = DIRECTION ( 'NONE',  ( -0.7858270635388553416, 0.000000000000000000, 0.6184463001828854889 ) ) ;
#23100 = ORIENTED_EDGE ( 'NONE', *, *, #9769, .F. ) ;
#23101 = CARTESIAN_POINT ( 'NONE',  ( 6.468171908630000466, -101.1402801299999936, 13.91008216630000049 ) ) ;
#23102 = CARTESIAN_POINT ( 'NONE',  ( -20.45998242170000125, -19.50000000000000000, 14.78974999389999923 ) ) ;
#23103 = AXIS2_PLACEMENT_3D ( 'NONE', #28745, #4290, #13605 ) ;
#23104 = CARTESIAN_POINT ( 'NONE',  ( -11.30171162149999908, -94.71348074940000572, -20.91579854999999810 ) ) ;
#23105 = CARTESIAN_POINT ( 'NONE',  ( 19.43643868430000410, -34.66800417059999262, -8.988996095199999203 ) ) ;
#23106 = DIRECTION ( 'NONE',  ( 0.000000000000000000, 1.000000000000000000, 0.000000000000000000 ) ) ;
#23107 = CARTESIAN_POINT ( 'NONE',  ( -17.60846427396887393, -93.38554229068824952, -21.34790020497966267 ) ) ;
#23108 =( NAMED_UNIT ( * ) SI_UNIT ( $, .STERADIAN. ) SOLID_ANGLE_UNIT ( ) );
#23109 = ORIENTED_EDGE ( 'NONE', *, *, #12030, .T. ) ;
#23110 = DIRECTION ( 'NONE',  ( 1.000000000000000000, 0.000000000000000000, 0.000000000000000000 ) ) ;
#23111 = CARTESIAN_POINT ( 'NONE',  ( -18.69985100839999959, -93.00000000000000000, 22.78328762010000119 ) ) ;
#23112 = ORIENTED_EDGE ( 'NONE', *, *, #5536, .T. ) ;
#23113 = CARTESIAN_POINT ( 'NONE',  ( -30.40304712095338502, -92.82529299094046848, 2.429966744979142224 ) ) ;
#23114 = EDGE_LOOP ( 'NONE', ( #11932, #5732, #2263, #16512 ) ) ;
#23115 = EDGE_CURVE ( 'NONE', #11794, #22379, #1986, .T. ) ;
#23116 = CARTESIAN_POINT ( 'NONE',  ( 0.6129623820366252307, -100.5798851008108414, -16.82649590739602630 ) ) ;
#23117 = CARTESIAN_POINT ( 'NONE',  ( -25.37284092810000047, -101.1889999979999999, 2.543411731580000001 ) ) ;
#23118 = FACE_OUTER_BOUND ( 'NONE', #22192, .T. ) ;
#23119 = CARTESIAN_POINT ( 'NONE',  ( 20.30284733819999943, -72.62832350799999404, -31.03260099770000124 ) ) ;
#23120 = EDGE_CURVE ( 'NONE', #7945, #3120, #6165, .T. ) ;
#23121 = CARTESIAN_POINT ( 'NONE',  ( -34.06928787630000244, -74.00000000000000000, -24.16979293970000242 ) ) ;
#23122 = CARTESIAN_POINT ( 'NONE',  ( -17.64295153049999954, -98.69230457299998704, 8.917116780599998904 ) ) ;
#23123 = CARTESIAN_POINT ( 'NONE',  ( 6.114061450890000415, -92.50000000000000000, -13.40104985119999981 ) ) ;
#23124 = CARTESIAN_POINT ( 'NONE',  ( -1.065814103639999922E-14, -36.00000000000000000, 3.552713678799999608E-15 ) ) ;
#23125 = DIRECTION ( 'NONE',  ( 0.4151946956541399669, 0.5000000000001689759, 0.7600087925152558821 ) ) ;
#23126 = ORIENTED_EDGE ( 'NONE', *, *, #11306, .T. ) ;
#23127 = CARTESIAN_POINT ( 'NONE',  ( -40.96188834619999852, -65.41419836839999391, 2.576072437790000169 ) ) ;
#23128 = B_SPLINE_CURVE_WITH_KNOTS ( 'NONE', 5,
 ( #8706, #26659, #6846, #24322, #10, #10737, #17774, #13235, #6392 ),
 .UNSPECIFIED., .F., .F.,
 ( 6, 3, 6 ),
 ( 0.000000000000000000, 0.3499052706296189585, 1.000000000000000000 ),
 .UNSPECIFIED. ) ;
#23129 = ORIENTED_EDGE ( 'NONE', *, *, #499, .T. ) ;
#23130 = CARTESIAN_POINT ( 'NONE',  ( -2.565551289909999699, -58.22369335140000146, -24.95564358469999888 ) ) ;
#23131 = CARTESIAN_POINT ( 'NONE',  ( -2.412598911559999948, -96.96081043750000106, 20.83962799120000042 ) ) ;
#23132 = CARTESIAN_POINT ( 'NONE',  ( 1.631270863969999985, -94.59275870510001027, 23.74088086560000121 ) ) ;
#23133 = VERTEX_POINT ( 'NONE', #19595 ) ;
#23134 = ORIENTED_EDGE ( 'NONE', *, *, #1249, .F. ) ;
#23135 = CARTESIAN_POINT ( 'NONE',  ( 31.00000000000000000, -15.00000000000000000, 2.042810365310000258E-14 ) ) ;
#23136 = CARTESIAN_POINT ( 'NONE',  ( 25.26718046270000073, -45.73899999920000425, 6.129403842640000377 ) ) ;
#23137 = ADVANCED_FACE ( 'NONE', ( #8369 ), #8494, .F. ) ;
#23138 = CARTESIAN_POINT ( 'NONE',  ( 0.000000000000000000, -94.59276292389999696, 0.000000000000000000 ) ) ;
#23139 = ORIENTED_EDGE ( 'NONE', *, *, #20238, .F. ) ;
#23140 = CARTESIAN_POINT ( 'NONE',  ( -27.18988201479999844, -31.10155444569999617, -49.77074518290000071 ) ) ;
#23141 = DIRECTION ( 'NONE',  ( 1.000000000000000000, 0.000000000000000000, 0.000000000000000000 ) ) ;
#23142 = ORIENTED_EDGE ( 'NONE', *, *, #26289, .F. ) ;
#23143 = EDGE_CURVE ( 'NONE', #20652, #640, #26170, .T. ) ;
#23144 = CARTESIAN_POINT ( 'NONE',  ( -14.59464643419999952, -80.37541664939999464, 36.43768143699999484 ) ) ;
#23145 = FACE_OUTER_BOUND ( 'NONE', #7112, .T. ) ;
#23146 = CARTESIAN_POINT ( 'NONE',  ( -2.199961190620000284, -69.66720773099999064, -27.15830649919999829 ) ) ;
#23147 = CARTESIAN_POINT ( 'NONE',  ( 0.000000000000000000, -39.32601556110000018, 0.000000000000000000 ) ) ;
#23148 = EDGE_LOOP ( 'NONE', ( #4610, #23727, #27113, #21402 ) ) ;
#23149 = TOROIDAL_SURFACE ( 'NONE', #367, 55.85192378860000417, 0.3499999999999999778 ) ;
#23150 = ADVANCED_FACE ( 'NONE', ( #15347 ), #26016, .F. ) ;
#23151 = CARTESIAN_POINT ( 'NONE',  ( -14.93121078260000090, -79.49999975080000070, 36.29905569799999654 ) ) ;
#23152 = CARTESIAN_POINT ( 'NONE',  ( -15.32770678129999986, -100.9616777990000003, 2.981256516259999767 ) ) ;
#23153 = CARTESIAN_POINT ( 'NONE',  ( 24.71478484869999903, -57.43018266680000039, 1.313252026010000018 ) ) ;
#23154 = CARTESIAN_POINT ( 'NONE',  ( -20.51803184719999962, -63.41300277309999700, 14.12505980070000078 ) ) ;
#23155 = VERTEX_POINT ( 'NONE', #14926 ) ;
#23156 = CARTESIAN_POINT ( 'NONE',  ( -19.81272040990000249, -52.63293862049999916, 12.05498172269999912 ) ) ;
#23157 = CARTESIAN_POINT ( 'NONE',  ( -2.784644191329999963, -18.86932112550000085, -24.02237818909999945 ) ) ;
#23158 = CARTESIAN_POINT ( 'NONE',  ( 23.32816514950000197, -93.91547326110000427, -8.285286069360001449 ) ) ;
#23159 = ORIENTED_EDGE ( 'NONE', *, *, #5821, .T. ) ;
#23160 = DIRECTION ( 'NONE',  ( 0.000000000000000000, 1.000000000000000000, 0.000000000000000000 ) ) ;
#23161 = B_SPLINE_CURVE_WITH_KNOTS ( 'NONE', 3,
 ( #17876, #11136, #17733, #15519 ),
 .UNSPECIFIED., .F., .F.,
 ( 4, 4 ),
 ( 12.34870497440000037, 33.81329059570000339 ),
 .UNSPECIFIED. ) ;
#23162 = DIRECTION ( 'NONE',  ( 0.000000000000000000, -1.000000000000000000, 0.000000000000000000 ) ) ;
#23163 = CONICAL_SURFACE ( 'NONE', #10538, 55.67692378859999280, 1.047197551199999799 ) ;
#23164 = DIRECTION ( 'NONE',  ( -0.4913402003782836314, 0.000000000000000000, 0.8709677419355024153 ) ) ;
#23165 = CARTESIAN_POINT ( 'NONE',  ( 16.40445051276553912, -100.4103893716901865, 4.355817310233436324 ) ) ;
#23166 = CARTESIAN_POINT ( 'NONE',  ( -12.60252398833393528, -66.16746083529757527, 22.33844947683535409 ) ) ;
#23167 = ORIENTED_EDGE ( 'NONE', *, *, #27497, .F. ) ;
#23168 = B_SPLINE_SURFACE_WITH_KNOTS ( 'NONE', 5, 5, ( 
 ( #4164, #2437, #21951, #8965, #8668, #2588 ),
 ( #11435, #26467, #8813, #26771, #6652, #19894 ),
 ( #17729, #11291, #6501, #9113, #15664, #24567 ),
 ( #4314, #15814, #13190, #2141, #26612, #10978 ),
 ( #24424, #4462, #21082, #23261, #27343, #5342 ),
 ( #22682, #9845, #7241, #4901, #25314, #11734 ) ),
 .UNSPECIFIED., .F., .F., .F.,
 ( 6, 6 ),
 ( 6, 6 ),
 ( 39.35985658629999762, 51.33494166999999919 ),
 ( 0.000000000000000000, 2.000000000000000000 ),
 .UNSPECIFIED. ) ;
#23169 = CARTESIAN_POINT ( 'NONE',  ( -12.30135761330000044, -18.50000000000000000, 18.36349993190000163 ) ) ;
#23170 = CARTESIAN_POINT ( 'NONE',  ( 37.09123793775638944, -79.93210607435938186, -14.11230097129613981 ) ) ;
#23171 = CARTESIAN_POINT ( 'NONE',  ( 26.38214771250000013, -68.90972708120000334, -11.00107859539999922 ) ) ;
#23172 = DIRECTION ( 'NONE',  ( 1.000000000000000000, 0.000000000000000000, 0.000000000000000000 ) ) ;
#23173 = ORIENTED_EDGE ( 'NONE', *, *, #26651, .F. ) ;
#23174 = CIRCLE ( 'NONE', #1293, 39.25000000000000000 ) ;
#23175 = CARTESIAN_POINT ( 'NONE',  ( -11.78425688200000110, -72.00000000000000000, -26.58404760160000180 ) ) ;
#23176 = ORIENTED_EDGE ( 'NONE', *, *, #8271, .F. ) ;
#23177 = CARTESIAN_POINT ( 'NONE',  ( -13.20732654740000100, -27.02040028920000125, 19.97234870039999777 ) ) ;
#23178 = CARTESIAN_POINT ( 'NONE',  ( -6.083378538189999851, -101.1716782080000030, 14.51061107299999975 ) ) ;
#23179 = ORIENTED_EDGE ( 'NONE', *, *, #3223, .T. ) ;
#23180 = LINE ( 'NONE', #4961, #11271 ) ;
#23181 = EDGE_CURVE ( 'NONE', #5907, #5258, #11220, .T. ) ;
#23182 = FACE_OUTER_BOUND ( 'NONE', #3293, .T. ) ;
#23183 = CARTESIAN_POINT ( 'NONE',  ( -10.83440914901318308, -19.46558565663113072, -19.38001281541565390 ) ) ;
#23184 = DIRECTION ( 'NONE',  ( 0.4794255386042040046, 0.000000000000000000, 0.8775825618903722036 ) ) ;
#23185 = ADVANCED_FACE ( 'NONE', ( #8520 ), #21785, .F. ) ;
#23186 = CARTESIAN_POINT ( 'NONE',  ( 3.551183598479999925E-15, -73.50000000000000000, -32.75000000000000000 ) ) ;
#23187 = CARTESIAN_POINT ( 'NONE',  ( 47.01293135346697483, -79.64648171702511092, -2.320651118032621252 ) ) ;
#23188 = ORIENTED_EDGE ( 'NONE', *, *, #3977, .T. ) ;
#23189 = PLANE ( 'NONE',  #7896 ) ;
#23190 = CARTESIAN_POINT ( 'NONE',  ( 15.79772739633221157, -101.6174239712916432, 2.678369929592316456 ) ) ;
#23191 = DIRECTION ( 'NONE',  ( 0.01112221585590945742, 0.000000000000000000, 0.9999381462442837876 ) ) ;
#23192 = ORIENTED_EDGE ( 'NONE', *, *, #23432, .F. ) ;
#23193 = CARTESIAN_POINT ( 'NONE',  ( -0.7293611917560000046, -79.74815767519999099, 47.25048488379999867 ) ) ;
#23194 = DIRECTION ( 'NONE',  ( -1.000000000000000000, 0.000000000000000000, 0.000000000000000000 ) ) ;
#23195 = ORIENTED_EDGE ( 'NONE', *, *, #9705, .F. ) ;
#23196 = CIRCLE ( 'NONE', #25519, 2.000000000000002665 ) ;
#23197 = DIRECTION ( 'NONE',  ( 0.000000000000000000, 1.000000000000000000, 0.000000000000000000 ) ) ;
#23198 = CARTESIAN_POINT ( 'NONE',  ( -18.66186151429999995, -26.09432050510000067, 12.57601491380000169 ) ) ;
#23199 = DIRECTION ( 'NONE',  ( 0.000000000000000000, -1.000000000000000000, 0.000000000000000000 ) ) ;
#23200 = CARTESIAN_POINT ( 'NONE',  ( 29.97212741979999961, -73.66823234569999101, -25.11762090529999725 ) ) ;
#23201 = CARTESIAN_POINT ( 'NONE',  ( 22.16163108380000324, -57.47158985090000272, -7.992697376199999759 ) ) ;
#23202 = EDGE_CURVE ( 'NONE', #23575, #23580, #5259, .T. ) ;
#23203 = CARTESIAN_POINT ( 'NONE',  ( 25.54892705720000023, -65.52795386139999323, 0.7157854019699999570 ) ) ;
#23204 = B_SPLINE_CURVE_WITH_KNOTS ( 'NONE', 5,
 ( #17772, #19507, #6390, #22142, #17184, #15254 ),
 .UNSPECIFIED., .F., .F.,
 ( 6, 6 ),
 ( 0.000000000000000000, 1.000000000000000000 ),
 .UNSPECIFIED. ) ;
#23205 = AXIS2_PLACEMENT_3D ( 'NONE', #17483, #12934, #2046 ) ;
#23206 = ORIENTED_EDGE ( 'NONE', *, *, #2655, .T. ) ;
#23207 = CARTESIAN_POINT ( 'NONE',  ( -19.73459494445757656, -19.18584080450766294, 14.41863469506854045 ) ) ;
#23208 = CARTESIAN_POINT ( 'NONE',  ( 21.63730777760000024, -37.52726933430000145, -8.187370782949999537 ) ) ;
#23209 = CARTESIAN_POINT ( 'NONE',  ( -43.20000000000000284, -63.00000000000000000, 0.1732050807559999961 ) ) ;
#23210 = ORIENTED_EDGE ( 'NONE', *, *, #5241, .F. ) ;
#23211 = DIRECTION ( 'NONE',  ( 0.4794255386042041156, 0.000000000000000000, 0.8775825618903722036 ) ) ;
#23212 = AXIS2_PLACEMENT_3D ( 'NONE', #748, #20827, #7721 ) ;
#23213 = EDGE_CURVE ( 'NONE', #14549, #2835, #3733, .T. ) ;
#23214 = CARTESIAN_POINT ( 'NONE',  ( -21.35786096709999882, -65.07443093669999712, 13.27975207949999970 ) ) ;
#23215 = CARTESIAN_POINT ( 'NONE',  ( -18.78219790299999659, -19.46510053389999939, 11.52011550950000007 ) ) ;
#23216 = CARTESIAN_POINT ( 'NONE',  ( 9.381593461630000519, -36.50000000249999488, -22.93608650079999833 ) ) ;
#23217 = DIRECTION ( 'NONE',  ( 1.000000000000000000, 0.000000000000000000, 0.000000000000000000 ) ) ;
#23218 = ORIENTED_EDGE ( 'NONE', *, *, #22748, .F. ) ;
#23219 = CARTESIAN_POINT ( 'NONE',  ( -40.29126735535079007, -74.18164516875299341, 7.244146985818024298 ) ) ;
#23220 = CARTESIAN_POINT ( 'NONE',  ( -23.91694143229999980, -93.67869433890000153, -7.293500637750000237 ) ) ;
#23221 = FACE_OUTER_BOUND ( 'NONE', #13943, .T. ) ;
#23222 = CARTESIAN_POINT ( 'NONE',  ( 11.34550471930000093, -98.29702512450000995, -15.37091565870000132 ) ) ;
#23223 = ORIENTED_EDGE ( 'NONE', *, *, #14883, .T. ) ;
#23224 = CARTESIAN_POINT ( 'NONE',  ( 20.27108563890000070, -18.61794786490000320, -7.599202272009999426 ) ) ;
#23225 = DIRECTION ( 'NONE',  ( -0.9295286103719527793, 0.000000000000000000, -0.3687499999999814260 ) ) ;
#23226 = CARTESIAN_POINT ( 'NONE',  ( -0.8695967735199999771, -32.73235193869999904, -22.48267697900000428 ) ) ;
#23227 = CARTESIAN_POINT ( 'NONE',  ( -17.07087492460914291, -92.82044061136174662, 25.27519173372845174 ) ) ;
#23228 = FACE_OUTER_BOUND ( 'NONE', #19358, .T. ) ;
#23229 = CARTESIAN_POINT ( 'NONE',  ( -1.776356839399999804E-15, -19.00000000000000000, 0.000000000000000000 ) ) ;
#23230 = CARTESIAN_POINT ( 'NONE',  ( 23.11289036089999982, -53.23790003319999897, -9.427231679889999327 ) ) ;
#23231 = DIRECTION ( 'NONE',  ( 1.000000000000000000, 0.000000000000000000, 0.000000000000000000 ) ) ;
#23232 = CARTESIAN_POINT ( 'NONE',  ( 36.25873697209999591, -74.65899625289999619, -15.02897531189999825 ) ) ;
#23233 = EDGE_LOOP ( 'NONE', ( #9226, #11410, #710, #9135, #23791, #7265, #13103, #19267, #12664, #27276, #26720, #13710, #12551, #4077, #9185, #24910, #25883, #14858, #1444, #1829, #2224, #28218 ) ) ;
#23234 = AXIS2_PLACEMENT_3D ( 'NONE', #16415, #12028, #25459 ) ;
#23235 = AXIS2_PLACEMENT_3D ( 'NONE', #21550, #10309, #23878 ) ;
#23236 = ADVANCED_FACE ( 'NONE', ( #28484 ), #14092, .T. ) ;
#23237 = CARTESIAN_POINT ( 'NONE',  ( 7.060623116049999481, -101.3256027139999986, 14.25378149400000005 ) ) ;
#23238 = CARTESIAN_POINT ( 'NONE',  ( 13.30084296762267293, -95.75133629986981987, -18.44067507113092574 ) ) ;
#23239 = AXIS2_PLACEMENT_3D ( 'NONE', #16063, #24965, #13884 ) ;
#23240 = ADVANCED_FACE ( 'NONE', ( #4150 ), #12656, .T. ) ;
#23241 = DIRECTION ( 'NONE',  ( 0.000000000000000000, -1.000000000000000000, 0.000000000000000000 ) ) ;
#23242 = CARTESIAN_POINT ( 'NONE',  ( 21.16123614720000035, -35.01845205400000083, -8.005892107839999383 ) ) ;
#23243 = CARTESIAN_POINT ( 'NONE',  ( 7.234868202887432709, -73.70809116058434540, 39.52985788716055993 ) ) ;
#23244 = EDGE_CURVE ( 'NONE', #11422, #16727, #23369, .T. ) ;
#23245 = CARTESIAN_POINT ( 'NONE',  ( 35.14430554270000329, -74.00000000000000000, -13.75000000000000000 ) ) ;
#23246 = CARTESIAN_POINT ( 'NONE',  ( -38.96765197713227025, -74.02518802155771027, 7.561758309935756373 ) ) ;
#23247 = SURFACE_STYLE_USAGE ( .BOTH. , #27634 ) ;
#23248 = ORIENTED_EDGE ( 'NONE', *, *, #12301, .T. ) ;
#23249 = TOROIDAL_SURFACE ( 'NONE', #22795, 55.85192378860000417, 0.3499999999999999778 ) ;
#23250 = CARTESIAN_POINT ( 'NONE',  ( -2.143666143589857853, -70.80051932422085770, -27.67943868423927967 ) ) ;
#23251 = DIRECTION ( 'NONE',  ( 1.000000000000000000, 0.000000000000000000, 0.000000000000000000 ) ) ;
#23252 = VERTEX_POINT ( 'NONE', #27186 ) ;
#23253 = DIRECTION ( 'NONE',  ( 0.000000000000000000, -1.000000000000000000, 0.000000000000000000 ) ) ;
#23254 = CIRCLE ( 'NONE', #15780, 21.03431122519999974 ) ;
#23255 = CARTESIAN_POINT ( 'NONE',  ( 0.6119498907216414096, -100.5550990433582541, -16.84632490533061855 ) ) ;
#23256 = FACE_OUTER_BOUND ( 'NONE', #10636, .T. ) ;
#23257 = DIRECTION ( 'NONE',  ( 1.000000000000000000, 0.000000000000000000, 0.000000000000000000 ) ) ;
#23258 = CARTESIAN_POINT ( 'NONE',  ( 13.15187379876893559, -92.89593097429261093, 27.51868946396341542 ) ) ;
#23259 = CARTESIAN_POINT ( 'NONE',  ( -12.60062440519999960, -94.64125147549999895, -21.54742969149999965 ) ) ;
#23260 = CARTESIAN_POINT ( 'NONE',  ( 23.74158351679999868, -72.51566206409999893, -30.51711889939999978 ) ) ;
#23261 = CARTESIAN_POINT ( 'NONE',  ( 10.19708627540000023, -71.08735242909999386, -26.16648790640000044 ) ) ;
#23262 = CARTESIAN_POINT ( 'NONE',  ( 13.68846061079999998, -95.60035679230000483, -17.92298507690000164 ) ) ;
#23263 = CARTESIAN_POINT ( 'NONE',  ( -15.16614058563374989, -101.1716787529999237, 4.188334258669885735 ) ) ;
#23264 = CARTESIAN_POINT ( 'NONE',  ( 8.966803191690001285, -31.61664946020000144, -19.80394353770000038 ) ) ;
#23265 = PLANE ( 'NONE',  #18436 ) ;
#23266 = CARTESIAN_POINT ( 'NONE',  ( -41.45000000000000284, -65.14977478849999670, -2.857883832489999776 ) ) ;
#23267 = ORIENTED_EDGE ( 'NONE', *, *, #456, .T. ) ;
#23268 = CARTESIAN_POINT ( 'NONE',  ( -40.65756524500000069, -65.56519245710001087, 2.400371413390000264 ) ) ;
#23269 = ORIENTED_EDGE ( 'NONE', *, *, #19442, .T. ) ;
#23270 = EDGE_CURVE ( 'NONE', #22416, #6793, #22327, .T. ) ;
#23272 = ADVANCED_FACE ( 'NONE', ( #8947 ), #17339, .T. ) ;
#23271 = AXIS2_PLACEMENT_3D ( 'NONE', #1494, #14314, #27596 ) ;
#23273 = AXIS2_PLACEMENT_3D ( 'NONE', #28607, #17403, #15180 ) ;
#23274 = CARTESIAN_POINT ( 'NONE',  ( -4.500000000000000000, -11.00000000000000000, 50.00000000000000000 ) ) ;
#23275 = EDGE_CURVE ( 'NONE', #14280, #3592, #12152, .T. ) ;
#23276 = CARTESIAN_POINT ( 'NONE',  ( -28.36632169019999949, -93.16461275549998788, 1.612349139190000002 ) ) ;
#23277 = CARTESIAN_POINT ( 'NONE',  ( 21.34788034980000049, -35.28814072549999281, -7.426815654249999454 ) ) ;
#23278 = EDGE_CURVE ( 'NONE', #13014, #4106, #10803, .T. ) ;
#23279 = ORIENTED_EDGE ( 'NONE', *, *, #9972, .F. ) ;
#23280 = CARTESIAN_POINT ( 'NONE',  ( -7.188503037714309762, -73.76099369285560670, 38.70686955322251777 ) ) ;
#23281 = ORIENTED_EDGE ( 'NONE', *, *, #15954, .T. ) ;
#23282 = CARTESIAN_POINT ( 'NONE',  ( 0.000000000000000000, -94.59276292389999696, 0.000000000000000000 ) ) ;
#23283 = CARTESIAN_POINT ( 'NONE',  ( -11.77206978281909677, -63.23144003730045171, 21.39278812554018572 ) ) ;
#23284 = ORIENTED_EDGE ( 'NONE', *, *, #22754, .T. ) ;
#23285 = CARTESIAN_POINT ( 'NONE',  ( -1.800052354129999976, -69.76823842119999597, -27.23143641409999915 ) ) ;
#23286 = CIRCLE ( 'NONE', #14446, 57.73884739369999863 ) ;
#23287 = CARTESIAN_POINT ( 'NONE',  ( -15.78247551950000194, -71.67546720299999663, 23.43991392560000264 ) ) ;
#23288 = AXIS2_PLACEMENT_3D ( 'NONE', #954, #27734, #1223 ) ;
#23289 = CARTESIAN_POINT ( 'NONE',  ( 36.39633395910000502, -74.06425117190001117, -14.25343207329999906 ) ) ;
#23290 = CARTESIAN_POINT ( 'NONE',  ( -16.70751862240000207, -99.92474288910000269, 2.933832141839999963 ) ) ;
#23291 = CARTESIAN_POINT ( 'NONE',  ( -20.66472140539999813, -61.67888006879999807, 14.89894363559999846 ) ) ;
#23292 = ORIENTED_EDGE ( 'NONE', *, *, #20503, .T. ) ;
#23293 = DIRECTION ( 'NONE',  ( 1.836909530730000976E-16, 0.000000000000000000, -1.000000000000000000 ) ) ;
#23294 = CARTESIAN_POINT ( 'NONE',  ( -3.258095469229999708, -18.50000000000000000, -23.26304047400000030 ) ) ;
#23295 = CARTESIAN_POINT ( 'NONE',  ( -7.911012669536270359, -100.3266728694704000, 15.09234432844895046 ) ) ;
#23296 = ORIENTED_EDGE ( 'NONE', *, *, #23782, .F. ) ;
#23297 = CARTESIAN_POINT ( 'NONE',  ( -41.46399166428601291, -65.14196057592134537, -2.865961923652742271 ) ) ;
#23298 = DIRECTION ( 'NONE',  ( 0.000000000000000000, -1.000000000000000000, 0.000000000000000000 ) ) ;
#23299 = CARTESIAN_POINT ( 'NONE',  ( 36.78520401009999574, -79.52803893530000323, -14.62663614230000064 ) ) ;
#23300 = CARTESIAN_POINT ( 'NONE',  ( -3.058911230670000148, -72.82938648530000592, -28.52031834779999997 ) ) ;
#23301 = EDGE_LOOP ( 'NONE', ( #25660, #3624, #3161, #3724 ) ) ;
#23302 = EDGE_CURVE ( 'NONE', #23053, #11658, #19290, .T. ) ;
#23303 = CARTESIAN_POINT ( 'NONE',  ( 37.29611236860000645, -80.00000000000000000, -13.75000000000000000 ) ) ;
#23304 = AXIS2_PLACEMENT_3D ( 'NONE', #18679, #7752, #16760 ) ;
#23305 = FACE_OUTER_BOUND ( 'NONE', #17747, .T. ) ;
#23306 = CIRCLE ( 'NONE', #26561, 57.75000000000000000 ) ;
#23307 = EDGE_CURVE ( 'NONE', #21547, #19815, #15944, .T. ) ;
#23308 = ORIENTED_EDGE ( 'NONE', *, *, #8628, .F. ) ;
#23309 = CIRCLE ( 'NONE', #2832, 3.499999999999999556 ) ;
#23310 = CARTESIAN_POINT ( 'NONE',  ( 47.25000000000000000, -75.00000000000000000, -1.242228542250000064E-12 ) ) ;
#23311 = ORIENTED_EDGE ( 'NONE', *, *, #12195, .F. ) ;
#23312 = CARTESIAN_POINT ( 'NONE',  ( -12.36746679350000022, -27.05111851250000043, 19.36625172230000302 ) ) ;
#23313 = CARTESIAN_POINT ( 'NONE',  ( -5.890277023240000354, -101.2306315440000049, 15.10563561669999899 ) ) ;
#23314 = VERTEX_POINT ( 'NONE', #9062 ) ;
#23315 = CARTESIAN_POINT ( 'NONE',  ( -3.843858959260458619, -97.05288880177764099, -20.70537388607158391 ) ) ;
#23316 = CARTESIAN_POINT ( 'NONE',  ( 21.34788034980000049, -35.28814072549999281, -7.426815654249999454 ) ) ;
#23317 = B_SPLINE_CURVE_WITH_KNOTS ( 'NONE', 5,
 ( #12611, #10010, #28354, #28081, #21116, #1172 ),
 .UNSPECIFIED., .F., .F.,
 ( 6, 6 ),
 ( 0.000000000000000000, 1.000000000000000000 ),
 .UNSPECIFIED. ) ;
#23318 = CARTESIAN_POINT ( 'NONE',  ( -7.215414233289999757, -74.50000000000000000, -40.70731707320000226 ) ) ;
#23319 = CARTESIAN_POINT ( 'NONE',  ( 24.46180220976096464, -66.34775779038977817, -7.978790679046251277 ) ) ;
#23320 = CARTESIAN_POINT ( 'NONE',  ( -17.94180966909999597, -45.73899999920000425, 18.81731824139999887 ) ) ;
#23321 = CARTESIAN_POINT ( 'NONE',  ( -14.45392997149999914, -92.99999875040001029, 26.19394095939999900 ) ) ;
#23322 = ORIENTED_EDGE ( 'NONE', *, *, #6748, .F. ) ;
#23323 = CARTESIAN_POINT ( 'NONE',  ( -32.56379503299999811, -80.00863944699999308, -22.48295750460000164 ) ) ;
#23324 = CARTESIAN_POINT ( 'NONE',  ( 16.08037959500000014, -101.3150700380000018, 2.354223078750000031 ) ) ;
#23325 = CARTESIAN_POINT ( 'NONE',  ( 0.000000000000000000, -86.00000000000000000, 0.000000000000000000 ) ) ;
#23326 = ORIENTED_EDGE ( 'NONE', *, *, #11110, .F. ) ;
#23327 = CIRCLE ( 'NONE', #16354, 0.5000000000000027756 ) ;
#23328 = CARTESIAN_POINT ( 'NONE',  ( -1.482066257490000094, -79.94411376969999594, 47.15825498670000115 ) ) ;
#23329 = DIRECTION ( 'NONE',  ( -0.9704142011833034598, 0.000000000000000000, 0.2414462220490750932 ) ) ;
#23330 = ORIENTED_EDGE ( 'NONE', *, *, #17672, .F. ) ;
#23331 = VECTOR ( 'NONE', #14381, 1000.000000000000000 ) ;
#23332 = CARTESIAN_POINT ( 'NONE',  ( 23.53302756460000111, -93.00000000000000000, -18.47479450719999861 ) ) ;
#23333 = VECTOR ( 'NONE', #13693, 1000.000000000000000 ) ;
#23334 = PLANE ( 'NONE',  #25048 ) ;
#23335 = CARTESIAN_POINT ( 'NONE',  ( 6.153546133999999945, -93.00000450890000536, 28.82528558229999760 ) ) ;
#23336 = CARTESIAN_POINT ( 'NONE',  ( 30.57937519460000075, -72.84979523120000522, -23.65429679820000075 ) ) ;
#23337 = CARTESIAN_POINT ( 'NONE',  ( -14.18731548340253035, -69.93408613758896308, 23.39951299694514475 ) ) ;
#23338 = EDGE_CURVE ( 'NONE', #5567, #6872, #22491, .T. ) ;
#23339 = B_SPLINE_SURFACE_WITH_KNOTS ( 'NONE', 5, 5, ( 
 ( #25022, #20951, #3177, #13946, #12032, #22847, #16266, #22993, #20806 ),
 ( #2889, #9707, #719, #27511, #7559, #16420, #25327, #5357, #16565 ),
 ( #14242, #23130, #1010, #9855, #18764, #25461, #14379, #4145, #10401 ),
 ( #8517, #8228, #21644, #12447, #19448, #17124, #21781, #12730, #15194 ),
 ( #26310, #3730, #21360, #24111, #13020, #28480, #3585, #25742, #5768 ),
 ( #19319, #17418, #23683, #23550, #8366, #10678, #1418, #21933, #1981 ),
 ( #10824, #12590, #19733, #28195, #28621, #26167, #15059, #10263, #25879 ),
 ( #28335, #1833, #14655, #6332, #26012, #21502, #6037, #16849, #19592 ),
 ( #23969, #19174, #28063, #8099, #16989, #14922, #4005, #17272, #5903 ) ),
 .UNSPECIFIED., .F., .F., .F.,
 ( 6, 3, 6 ),
 ( 6, 3, 6 ),
 ( 112.4516929440000013, 115.4092999559999981, 122.9563471680000077 ),
 ( 0.000000000000000000, 1.000000000000000000, 2.000000000000000000 ),
 .UNSPECIFIED. ) ;
#23340 = DIRECTION ( 'NONE',  ( 0.000000000000000000, 1.000000000000000000, 0.000000000000000000 ) ) ;
#23341 = EDGE_CURVE ( 'NONE', #10820, #8919, #13618, .T. ) ;
#23342 = ORIENTED_EDGE ( 'NONE', *, *, #9383, .T. ) ;
#23343 = CARTESIAN_POINT ( 'NONE',  ( -40.25190969051858048, -74.15297958058674510, -7.245634850454607978 ) ) ;
#23344 = DIRECTION ( 'NONE',  ( 0.000000000000000000, -1.000000000000000000, 0.000000000000000000 ) ) ;
#23345 = CARTESIAN_POINT ( 'NONE',  ( 21.11247224599999939, -36.35195199729999871, -8.702043174359999966 ) ) ;
#23346 = CARTESIAN_POINT ( 'NONE',  ( 6.962669195700001090, -93.00000450890000536, -28.64060852350000275 ) ) ;
#23347 = ORIENTED_EDGE ( 'NONE', *, *, #25450, .T. ) ;
#23348 = CIRCLE ( 'NONE', #24254, 3.500000000000003109 ) ;
#23349 = CARTESIAN_POINT ( 'NONE',  ( -13.35118457799999980, -101.4309749570000037, -9.111440644229999108 ) ) ;
#23350 = CARTESIAN_POINT ( 'NONE',  ( 7.771052952609999345E-15, -82.25000000000000000, -47.25000000000000000 ) ) ;
#23351 = CIRCLE ( 'NONE', #21034, 38.75000000000000000 ) ;
#23352 = DIRECTION ( 'NONE',  ( 0.000000000000000000, 1.000000000000000000, 0.000000000000000000 ) ) ;
#23353 = CARTESIAN_POINT ( 'NONE',  ( -7.893993299629999960, -100.5229262450000078, 14.92267151810000136 ) ) ;
#23354 = CARTESIAN_POINT ( 'NONE',  ( 8.968806686069999756, -40.71455396189999476, -22.20693316839999909 ) ) ;
#23355 = CARTESIAN_POINT ( 'NONE',  ( 7.584268328590000330, -101.1889999979999999, 14.08825304710000026 ) ) ;
#23356 = ORIENTED_EDGE ( 'NONE', *, *, #22410, .T. ) ;
#23357 = CARTESIAN_POINT ( 'NONE',  ( -43.28598031665701740, -65.10234783420354177, 0.07523755578869117944 ) ) ;
#23358 = EDGE_CURVE ( 'NONE', #18300, #5668, #18843, .T. ) ;
#23359 = CARTESIAN_POINT ( 'NONE',  ( -23.90121231679999880, -94.07620464550001316, -7.056844240210001118 ) ) ;
#23360 = CARTESIAN_POINT ( 'NONE',  ( -13.46276276179999876, -19.49999999970000175, 20.39865906480000035 ) ) ;
#23361 = CARTESIAN_POINT ( 'NONE',  ( 10.37409836790000028, -95.71128647580000859, -20.04562559420000412 ) ) ;
#23362 = ORIENTED_EDGE ( 'NONE', *, *, #10335, .F. ) ;
#23363 = CARTESIAN_POINT ( 'NONE',  ( 19.45828891929999926, -18.50000000000000000, -8.201027286100000424 ) ) ;
#23364 = DIRECTION ( 'NONE',  ( 0.000000000000000000, -1.000000000000000000, 0.000000000000000000 ) ) ;
#23365 = CARTESIAN_POINT ( 'NONE',  ( -14.93121066289999987, -74.43375220249998847, 36.29905574720000061 ) ) ;
#23366 = CARTESIAN_POINT ( 'NONE',  ( -18.24886321460000005, -94.80026206440000180, 16.23660667690000281 ) ) ;
#23367 = CARTESIAN_POINT ( 'NONE',  ( -17.13188320504061934, -92.80045754877718878, 25.23390446720919655 ) ) ;
#23368 = CARTESIAN_POINT ( 'NONE',  ( 5.273680924649999824, -107.5000000000000000, 9.653408180790000515 ) ) ;
#23369 = B_SPLINE_CURVE_WITH_KNOTS ( 'NONE', 3,
 ( #22667, #17998, #9240, #7084 ),
 .UNSPECIFIED., .F., .F.,
 ( 4, 4 ),
 ( 0.000000000000000000, 1.000000000000000000 ),
 .UNSPECIFIED. ) ;
#23370 = CARTESIAN_POINT ( 'NONE',  ( 8.991798710090000313, -35.60470291170000223, -19.53731210289999964 ) ) ;
#23371 = CARTESIAN_POINT ( 'NONE',  ( 21.43629755400000292, -36.56833509949999694, -7.482057485250000362 ) ) ;
#23372 = CARTESIAN_POINT ( 'NONE',  ( 18.08741318713345692, -95.90275958024609793, 14.78486932492663897 ) ) ;
#23373 = AXIS2_PLACEMENT_3D ( 'NONE', #23571, #12754, #19617 ) ;
#23374 = EDGE_LOOP ( 'NONE', ( #14002, #21506, #1583, #1591 ) ) ;
#23375 = EDGE_CURVE ( 'NONE', #16619, #22108, #2938, .T. ) ;
#23376 = B_SPLINE_CURVE_WITH_KNOTS ( 'NONE', 5,
 ( #13130, #13426, #9055, #22185, #28716, #17960 ),
 .UNSPECIFIED., .F., .F.,
 ( 6, 6 ),
 ( 0.000000000000000000, 1.000000000000000000 ),
 .UNSPECIFIED. ) ;
#23377 = CARTESIAN_POINT ( 'NONE',  ( -32.67527182230000449, -74.45928706499999805, -22.00249031449999748 ) ) ;
#23378 = CARTESIAN_POINT ( 'NONE',  ( 13.08001772823451070, -95.36087494481114391, -19.20617372813112311 ) ) ;
#23379 = EDGE_CURVE ( 'NONE', #400, #25480, #14554, .T. ) ;
#23380 = CARTESIAN_POINT ( 'NONE',  ( 14.62430634820000108, -74.00000000000000000, 26.76961320899999919 ) ) ;
#23381 = CARTESIAN_POINT ( 'NONE',  ( 8.346761719239998101, -35.62468481330000003, -21.07000052020000069 ) ) ;
#23382 = CARTESIAN_POINT ( 'NONE',  ( 0.000000000000000000, -2.000000000000000000, 0.000000000000000000 ) ) ;
#23383 = CARTESIAN_POINT ( 'NONE',  ( -14.39036416260000095, -64.35840737179999849, 21.98073843050000065 ) ) ;
#23384 = CARTESIAN_POINT ( 'NONE',  ( -40.35493623782935657, -74.39269056238592270, 7.250053749311780038 ) ) ;
#23385 = CARTESIAN_POINT ( 'NONE',  ( 46.25000000000000000, -80.00000000000000000, -9.166287847479999584 ) ) ;
#23386 = VERTEX_POINT ( 'NONE', #9028 ) ;
#23387 = CARTESIAN_POINT ( 'NONE',  ( 8.188637977920000921, -100.9197082849999987, 13.30686163390000054 ) ) ;
#23388 = CARTESIAN_POINT ( 'NONE',  ( -26.33972759919999973, -79.50000000000000000, -36.23922253580000330 ) ) ;
#23389 = ORIENTED_EDGE ( 'NONE', *, *, #21022, .T. ) ;
#23390 = AXIS2_PLACEMENT_3D ( 'NONE', #388, #7081, #6783 ) ;
#23391 = CARTESIAN_POINT ( 'NONE',  ( -31.00000000000000000, -15.00000000000000000, -4.500000000000000000 ) ) ;
#23392 = ORIENTED_EDGE ( 'NONE', *, *, #16533, .F. ) ;
#23393 = CARTESIAN_POINT ( 'NONE',  ( 0.5678894871162830649, -100.9510322836843272, -16.53366320519699073 ) ) ;
#23394 = ADVANCED_FACE ( 'NONE', ( #13547 ), #22456, .T. ) ;
#23395 = CARTESIAN_POINT ( 'NONE',  ( 6.185491179879999635, -101.0875971110000080, 14.11315596670000083 ) ) ;
#23396 = B_SPLINE_CURVE_WITH_KNOTS ( 'NONE', 3,
 ( #20509, #27220, #18769, #5060, #9994, #27364 ),
 .UNSPECIFIED., .F., .F.,
 ( 4, 2, 4 ),
 ( 0.000000000000000000, 0.5000000000000000000, 1.000000000000000000 ),
 .UNSPECIFIED. ) ;
#23397 = CARTESIAN_POINT ( 'NONE',  ( 13.66357347539002731, -92.59055325467724629, 27.26823877034133403 ) ) ;
#23398 = EDGE_CURVE ( 'NONE', #13829, #15667, #5721, .T. ) ;
#23399 = CARTESIAN_POINT ( 'NONE',  ( 15.60984783840000034, -101.0640712160000021, 3.941010556740000670 ) ) ;
#23400 = CARTESIAN_POINT ( 'NONE',  ( 27.75394116159999669, -74.50000000000000000, -27.75394116159999669 ) ) ;
#23401 = FACE_OUTER_BOUND ( 'NONE', #6126, .T. ) ;
#23402 = B_SPLINE_SURFACE_WITH_KNOTS ( 'NONE', 5, 5, ( 
 ( #20279, #9344, #13724, #2668, #22624, #7182, #4981, #14443, #3650 ),
 ( #14576, #14305, #10185, #12247, #19101, #12103, #21159, #10048, #23068 ),
 ( #16627, #9778, #25523, #25809, #3382, #3110, #23336, #23606, #14168 ),
 ( #1214, #12514, #7890, #23481, #23200, #27989, #18962, #8024, #27845 ),
 ( #11963, #21019, #1080, #21424, #5835, #3247, #14716, #20877, #1483 ),
 ( #9919, #12376, #5692, #3520, #5281, #18833, #7482, #18691, #18539 ) ),
 .UNSPECIFIED., .F., .F., .F.,
 ( 6, 6 ),
 ( 6, 3, 6 ),
 ( 0.4663536434559999999, 13.03296576320000000 ),
 ( 0.000000000000000000, 1.000000000000000000, 2.000000000000000000 ),
 .UNSPECIFIED. ) ;
#23403 = CARTESIAN_POINT ( 'NONE',  ( 0.000000000000000000, -65.07443093669999712, 0.000000000000000000 ) ) ;
#23404 = CARTESIAN_POINT ( 'NONE',  ( 8.993760894959999419, -31.63434272479999976, -19.33939736140000321 ) ) ;
#23405 = DIRECTION ( 'NONE',  ( 0.000000000000000000, 1.000000000000000000, 0.000000000000000000 ) ) ;
#23406 = EDGE_CURVE ( 'NONE', #23820, #3841, #22480, .T. ) ;
#23407 = CARTESIAN_POINT ( 'NONE',  ( 19.98802563500222007, -19.46625705893007563, 9.814437999406528945 ) ) ;
#23408 = EDGE_LOOP ( 'NONE', ( #4910, #11799, #2087, #22226 ) ) ;
#23409 = CARTESIAN_POINT ( 'NONE',  ( -11.35954001540000036, -74.50000000000000000, 47.25000000000000000 ) ) ;
#23410 = AXIS2_PLACEMENT_3D ( 'NONE', #12141, #20915, #25141 ) ;
#23411 = VECTOR ( 'NONE', #20366, 999.9999999999998863 ) ;
#23412 = ORIENTED_EDGE ( 'NONE', *, *, #13382, .F. ) ;
#23413 = AXIS2_PLACEMENT_3D ( 'NONE', #10828, #15500, #19875 ) ;
#23414 = ORIENTED_EDGE ( 'NONE', *, *, #10628, .F. ) ;
#23415 = DIRECTION ( 'NONE',  ( 0.000000000000000000, 0.000000000000000000, 1.000000000000000000 ) ) ;
#23416 = CARTESIAN_POINT ( 'NONE',  ( -28.36339762329999914, -93.07693985719998864, 1.604523527660000060 ) ) ;
#23417 = CARTESIAN_POINT ( 'NONE',  ( 19.49544348199999888, -35.50000000000000000, -8.986258402430001624 ) ) ;
#23418 = DIRECTION ( 'NONE',  ( 0.000000000000000000, 1.000000000000000000, 0.000000000000000000 ) ) ;
#23419 = ORIENTED_EDGE ( 'NONE', *, *, #16493, .F. ) ;
#23420 = AXIS2_PLACEMENT_3D ( 'NONE', #15712, #463, #16013 ) ;
#23421 = CARTESIAN_POINT ( 'NONE',  ( -28.12914522643169590, -93.25521311031921812, 1.335511596251312660 ) ) ;
#23422 = ORIENTED_EDGE ( 'NONE', *, *, #3564, .F. ) ;
#23423 = DIRECTION ( 'NONE',  ( -0.3422283636740854340, 0.7003189540771749266, -0.6264448177271558782 ) ) ;
#23424 = CARTESIAN_POINT ( 'NONE',  ( 9.092656154049999273, -35.82930178739999860, -19.86172366460000305 ) ) ;
#23425 = VERTEX_POINT ( 'NONE', #11801 ) ;
#23426 = CARTESIAN_POINT ( 'NONE',  ( 26.67791892279999999, -92.70565333729999224, -10.13078936369999994 ) ) ;
#23427 = AXIS2_PLACEMENT_3D ( 'NONE', #23282, #21511, #19049 ) ;
#23428 = B_SPLINE_CURVE_WITH_KNOTS ( 'NONE', 5,
 ( #7342, #11540, #24677, #13591, #11395, #4997 ),
 .UNSPECIFIED., .F., .F.,
 ( 6, 6 ),
 ( 0.000000000000000000, 1.000000000000000000 ),
 .UNSPECIFIED. ) ;
#23429 = AXIS2_PLACEMENT_3D ( 'NONE', #9761, #20859, #25505 ) ;
#23430 = CARTESIAN_POINT ( 'NONE',  ( -19.16298526259999946, -18.50000000000000000, 15.26553041949999923 ) ) ;
#23431 = ORIENTED_EDGE ( 'NONE', *, *, #20847, .F. ) ;
#23432 = EDGE_CURVE ( 'NONE', #24445, #15756, #3225, .T. ) ;
#23433 = CARTESIAN_POINT ( 'NONE',  ( -15.35368226649999990, -101.3957230199999913, 4.453032938229999793 ) ) ;
#23434 = CARTESIAN_POINT ( 'NONE',  ( -15.39298286279999850, -100.9658258050000086, 3.068543784489999648 ) ) ;
#23435 = CARTESIAN_POINT ( 'NONE',  ( 23.90606521969999676, -57.45864773929999814, 0.8443132633689999222 ) ) ;
#23436 = CARTESIAN_POINT ( 'NONE',  ( -21.04849736790000136, -64.58097846009999898, 14.98503047890000062 ) ) ;
#23437 = EDGE_LOOP ( 'NONE', ( #17075, #7965, #20721, #21786 ) ) ;
#23438 = DIRECTION ( 'NONE',  ( 1.000000000000000000, 0.000000000000000000, 0.000000000000000000 ) ) ;
#23439 = EDGE_CURVE ( 'NONE', #12631, #22913, #10467, .T. ) ;
#23440 = CARTESIAN_POINT ( 'NONE',  ( -7.301026670105736471, -73.99985427505767177, 39.56397514584002550 ) ) ;
#23441 = CARTESIAN_POINT ( 'NONE',  ( 36.55403876290004916, -74.10879610147962637, -14.20614005299821159 ) ) ;
#23442 = ORIENTED_EDGE ( 'NONE', *, *, #19657, .T. ) ;
#23443 = EDGE_CURVE ( 'NONE', #1115, #22453, #9896, .T. ) ;
#23444 = CIRCLE ( 'NONE', #10830, 4.750000000000000888 ) ;
#23445 = DIRECTION ( 'NONE',  ( 0.000000000000000000, -1.000000000000000000, 0.000000000000000000 ) ) ;
#23446 = CARTESIAN_POINT ( 'NONE',  ( -41.78982036957599888, -65.72001381778289897, -1.308254260903399357 ) ) ;
#23447 = CARTESIAN_POINT ( 'NONE',  ( 36.80029846600000099, -80.01820861420000597, -14.08441020739999949 ) ) ;
#23448 = CARTESIAN_POINT ( 'NONE',  ( 13.98007502452994189, -99.57060688034719931, -10.30433862638093423 ) ) ;
#23449 = ORIENTED_EDGE ( 'NONE', *, *, #12006, .F. ) ;
#23450 = CARTESIAN_POINT ( 'NONE',  ( 36.78022402065349183, -79.46798840176322187, -14.63388022524676657 ) ) ;
#23451 = TOROIDAL_SURFACE ( 'NONE', #7174, 30.50381168839999901, 2.000000000000000000 ) ;
#23452 = CARTESIAN_POINT ( 'NONE',  ( -1.680150139059958248, -80.11422939166462243, 47.05278015009087511 ) ) ;
#23453 = VERTEX_POINT ( 'NONE', #3360 ) ;
#23454 = DIRECTION ( 'NONE',  ( 0.000000000000000000, 0.000000000000000000, -1.000000000000000000 ) ) ;
#23455 = EDGE_LOOP ( 'NONE', ( #7295, #14153, #22112, #2463 ) ) ;
#23456 = CARTESIAN_POINT ( 'NONE',  ( 28.21663026719999934, -92.49537389030000156, 8.246881169159999914 ) ) ;
#23457 = CARTESIAN_POINT ( 'NONE',  ( -5.897337460870000214, -101.1411470150000014, 14.21533967550000099 ) ) ;
#23458 = ORIENTED_EDGE ( 'NONE', *, *, #7780, .T. ) ;
#23459 = CARTESIAN_POINT ( 'NONE',  ( 14.01704999690000086, -99.70407914540000149, -9.961568965490000593 ) ) ;
#23460 = CARTESIAN_POINT ( 'NONE',  ( -29.47186832370000076, -93.00000450890000536, -0.4149655844399999793 ) ) ;
#23461 = AXIS2_PLACEMENT_3D ( 'NONE', #26071, #17620, #4059 ) ;
#23462 = AXIS2_PLACEMENT_3D ( 'NONE', #1142, #3304, #7389 ) ;
#23463 = CARTESIAN_POINT ( 'NONE',  ( 40.34091732210000458, -74.29300278819999903, 7.252014196640000243 ) ) ;
#23464 = CARTESIAN_POINT ( 'NONE',  ( -13.26381099438660982, -101.5019029710790477, -9.144658545510399250 ) ) ;
#23465 = CARTESIAN_POINT ( 'NONE',  ( 7.405704750090000843, -101.1273033739999931, 13.62605079230000094 ) ) ;
#23466 = CARTESIAN_POINT ( 'NONE',  ( 47.14083139015517787, -79.45829804079036762, -1.597024166738013840 ) ) ;
#23467 = VERTEX_POINT ( 'NONE', #18670 ) ;
#23468 = EDGE_CURVE ( 'NONE', #8977, #21937, #23847, .T. ) ;
#23469 = CARTESIAN_POINT ( 'NONE',  ( -18.71084207290000023, -96.58372172930000943, -10.18677576210000169 ) ) ;
#23470 = CARTESIAN_POINT ( 'NONE',  ( 15.85792770375962490, -101.5620304352200094, 2.570904433130984046 ) ) ;
#23471 = CARTESIAN_POINT ( 'NONE',  ( -4.500000000000000000, -11.00000000000000000, -50.00000000000000000 ) ) ;
#23472 = VERTEX_POINT ( 'NONE', #24933 ) ;
#23473 = STYLED_ITEM ( 'NONE', ( #21804 ), #25398 ) ;
#23474 = CARTESIAN_POINT ( 'NONE',  ( -2.675183968039999827E-13, -79.50000000000000000, 47.25000000000000000 ) ) ;
#23475 = CARTESIAN_POINT ( 'NONE',  ( 22.42985916568536808, -18.87168151092972934, 9.783895424303356236 ) ) ;
#23476 = EDGE_LOOP ( 'NONE', ( #24959, #25838, #2609, #20551 ) ) ;
#23477 = EDGE_CURVE ( 'NONE', #14668, #27292, #101, .T. ) ;
#23478 = DIRECTION ( 'NONE',  ( 0.8981584475625411512, 0.000000000000000000, 0.4396719266362661416 ) ) ;
#23479 = CARTESIAN_POINT ( 'NONE',  ( 0.000000000000000000, -19.70310889130000120, 0.000000000000000000 ) ) ;
#23480 = DIRECTION ( 'NONE',  ( 0.000000000000000000, 1.000000000000000000, 0.000000000000000000 ) ) ;
#23481 = CARTESIAN_POINT ( 'NONE',  ( 30.05801312899999900, -73.89113795069999924, -25.09024318069999993 ) ) ;
#23482 = CARTESIAN_POINT ( 'NONE',  ( 7.120909764619999412E-15, -69.50000000000000000, 40.00000000000000000 ) ) ;
#23483 = CARTESIAN_POINT ( 'NONE',  ( -17.94180966909999597, -72.00000000000000000, 18.81731824139999887 ) ) ;
#23484 = AXIS2_PLACEMENT_3D ( 'NONE', #11085, #15770, #17830 ) ;
#23485 = ORIENTED_EDGE ( 'NONE', *, *, #11122, .F. ) ;
#23486 = CARTESIAN_POINT ( 'NONE',  ( -40.21639064514770467, -74.12723354439698653, -7.246819345882184571 ) ) ;
#23487 = CARTESIAN_POINT ( 'NONE',  ( 21.67753623600000168, -37.30770946170000002, -8.432260248800000468 ) ) ;
#23488 = CARTESIAN_POINT ( 'NONE',  ( -35.61208719050000582, -69.00000000000000000, 2.397127693020000283 ) ) ;
#23489 = ORIENTED_EDGE ( 'NONE', *, *, #6922, .F. ) ;
#23490 = AXIS2_PLACEMENT_3D ( 'NONE', #7789, #9667, #23231 ) ;
#23491 = CARTESIAN_POINT ( 'NONE',  ( -12.92073601179999898, -101.4254868729999970, -9.384144184709999337 ) ) ;
#23492 = CARTESIAN_POINT ( 'NONE',  ( -18.05095945240000077, -93.00000167610001256, -23.30076308599999635 ) ) ;
#23493 = ORIENTED_EDGE ( 'NONE', *, *, #20265, .F. ) ;
#23494 = AXIS2_PLACEMENT_3D ( 'NONE', #22696, #11895, #25178 ) ;
#23495 = CARTESIAN_POINT ( 'NONE',  ( -10.19002250800000020, -74.00000000000000000, 42.30193224820000353 ) ) ;
#23496 = ADVANCED_FACE ( 'NONE', ( #19360 ), #17314, .T. ) ;
#23497 = CARTESIAN_POINT ( 'NONE',  ( 9.146761579599999692, -36.52243084939999562, -22.33517371059999945 ) ) ;
#23498 = CARTESIAN_POINT ( 'NONE',  ( 7.258489506040000094, -101.1848542409999823, 13.44827353360000188 ) ) ;
#23499 = ORIENTED_EDGE ( 'NONE', *, *, #20883, .T. ) ;
#23500 = EDGE_CURVE ( 'NONE', #8240, #20924, #22001, .T. ) ;
#23501 = CARTESIAN_POINT ( 'NONE',  ( 13.53766003414172303, -100.5798851008411958, -10.01191531143067515 ) ) ;
#23502 = DIRECTION ( 'NONE',  ( 1.000000000000000000, 0.000000000000000000, 2.220446049250004932E-16 ) ) ;
#23503 = CARTESIAN_POINT ( 'NONE',  ( 26.11117489990000351, -71.37991020869999659, 10.95904867260000159 ) ) ;
#23504 = CARTESIAN_POINT ( 'NONE',  ( 11.77817161740000174, -101.0685845459999967, -10.96540424870000052 ) ) ;
#23505 = VERTEX_POINT ( 'NONE', #23590 ) ;
#23506 = CIRCLE ( 'NONE', #5809, 28.68388914670000034 ) ;
#23507 = DIRECTION ( 'NONE',  ( 1.000000000000000000, 0.000000000000000000, 0.000000000000000000 ) ) ;
#23508 = CARTESIAN_POINT ( 'NONE',  ( 11.91396536729999944, -101.5026188610000020, -10.71358336220000140 ) ) ;
#23509 = CARTESIAN_POINT ( 'NONE',  ( -14.54102251839999838, -74.30694342880001102, 36.58803169640000164 ) ) ;
#23510 = CARTESIAN_POINT ( 'NONE',  ( -17.84952165019999981, -94.52419090329999563, 16.07137172610000064 ) ) ;
#23511 = CARTESIAN_POINT ( 'NONE',  ( -17.09135004194092744, -92.81370807125685474, 25.26135588419946743 ) ) ;
#23512 = EDGE_LOOP ( 'NONE', ( #13470, #23519, #1328, #8560 ) ) ;
#23513 = EDGE_CURVE ( 'NONE', #19506, #1569, #25721, .T. ) ;
#23514 = DIRECTION ( 'NONE',  ( 0.8270692982020247941, 0.000000000000000000, 0.5620999697310169463 ) ) ;
#23515 = CARTESIAN_POINT ( 'NONE',  ( -0.06019592984270000224, -101.1411470200000053, -15.38951065810000074 ) ) ;
#23516 = CARTESIAN_POINT ( 'NONE',  ( 26.73328043595045500, -92.86910576385056970, -12.41347163419055732 ) ) ;
#23517 = CARTESIAN_POINT ( 'NONE',  ( 15.32699008580000033, -101.0555477039999914, 2.288286655999999919 ) ) ;
#23518 = CARTESIAN_POINT ( 'NONE',  ( 6.850353625200000351, -36.56979901409999911, -21.56931447779999900 ) ) ;
#23519 = ORIENTED_EDGE ( 'NONE', *, *, #2317, .T. ) ;
#23520 = CARTESIAN_POINT ( 'NONE',  ( 6.467641717930000311, -99.94549701829998867, 15.61536050989999858 ) ) ;
#23521 = DIRECTION ( 'NONE',  ( 0.000000000000000000, -1.000000000000000000, 0.000000000000000000 ) ) ;
#23522 = CIRCLE ( 'NONE', #22587, 16.00000000000000000 ) ;
#23523 = CARTESIAN_POINT ( 'NONE',  ( -11.31666932600000131, -95.23931402160000914, -21.36057898460000004 ) ) ;
#23524 = CARTESIAN_POINT ( 'NONE',  ( 7.344927635980000424, -35.54843156109999569, -21.39482692749999870 ) ) ;
#23525 = CARTESIAN_POINT ( 'NONE',  ( 23.66024254313331454, -62.10681979203287284, 10.59952656403941162 ) ) ;
#23526 = CARTESIAN_POINT ( 'NONE',  ( -7.895913362729999996, -99.83167544280000527, 15.41983155350000168 ) ) ;
#23527 = CARTESIAN_POINT ( 'NONE',  ( 8.558808717420001599, -94.34469964509999329, -23.93930828130000066 ) ) ;
#23528 = CARTESIAN_POINT ( 'NONE',  ( 19.59884367089999913, -25.54957699810000094, -8.972031911080001976 ) ) ;
#23529 = DIRECTION ( 'NONE',  ( 0.4794255386042041711, 0.000000000000000000, 0.8775825618903720926 ) ) ;
#23530 = ORIENTED_EDGE ( 'NONE', *, *, #27869, .F. ) ;
#23531 = DIRECTION ( 'NONE',  ( 0.000000000000000000, 1.000000000000000000, 0.000000000000000000 ) ) ;
#23532 = VERTEX_POINT ( 'NONE', #8268 ) ;
#23533 = CARTESIAN_POINT ( 'NONE',  ( 24.78974732560000405, -64.24504771300000527, -10.08508462690000052 ) ) ;
#23534 = ADVANCED_FACE ( 'NONE', ( #5944 ), #1538, .T. ) ;
#23535 = CARTESIAN_POINT ( 'NONE',  ( 0.3657531947015631446, -101.3586211803499850, -16.22016006312202663 ) ) ;
#23536 = CARTESIAN_POINT ( 'NONE',  ( -7.249922272500000098, -74.00000000000000000, 40.03357376780000010 ) ) ;
#23537 = CIRCLE ( 'NONE', #9556, 3.000000000000002665 ) ;
#23538 = CARTESIAN_POINT ( 'NONE',  ( 13.33972531995206623, -92.72059904818746645, 27.42811962378058510 ) ) ;
#23539 = EDGE_CURVE ( 'NONE', #6357, #21012, #2526, .T. ) ;
#23540 = CARTESIAN_POINT ( 'NONE',  ( 27.75394116159999669, -74.50000000000000000, -27.75394116159999669 ) ) ;
#23541 = CARTESIAN_POINT ( 'NONE',  ( -22.15796614980000001, -69.30519277740000916, 16.22735913770000238 ) ) ;
#23542 = CARTESIAN_POINT ( 'NONE',  ( 20.49657866619999780, -57.47855601759999900, 11.20866246179999948 ) ) ;
#23543 = CARTESIAN_POINT ( 'NONE',  ( -11.96164838680000031, -64.89183635400000583, -23.89138425040000158 ) ) ;
#23544 = CARTESIAN_POINT ( 'NONE',  ( -41.75000000000000000, -63.07912966450000880, 2.684678751729999480 ) ) ;
#23545 = AXIS2_PLACEMENT_3D ( 'NONE', #8612, #6588, #24217 ) ;
#23546 = ORIENTED_EDGE ( 'NONE', *, *, #28542, .F. ) ;
#23547 = ORIENTED_EDGE ( 'NONE', *, *, #11336, .F. ) ;
#23548 = CARTESIAN_POINT ( 'NONE',  ( -42.75000000000000000, -65.00000000000000000, -1.587713240270000048 ) ) ;
#23549 = VERTEX_POINT ( 'NONE', #25918 ) ;
#23550 = CARTESIAN_POINT ( 'NONE',  ( -2.341796741959999650, -61.59774147150000090, -24.80816657779999801 ) ) ;
#23551 = B_SPLINE_CURVE_WITH_KNOTS ( 'NONE', 5,
 ( #16863, #3596, #5644, #14522, #7573, #11911 ),
 .UNSPECIFIED., .F., .F.,
 ( 6, 6 ),
 ( -66.18347591719999912, -36.59856967279999651 ),
 .UNSPECIFIED. ) ;
#23552 = CARTESIAN_POINT ( 'NONE',  ( -26.77683864449999973, -15.80000000000000071, -49.01467436490000296 ) ) ;
#23553 = CARTESIAN_POINT ( 'NONE',  ( 9.273496630181142564, -94.57749869816520061, -22.35125168207579804 ) ) ;
#23554 = CARTESIAN_POINT ( 'NONE',  ( 18.94592261899999741, -19.50000000000000000, -9.024080787800000891 ) ) ;
#23555 = EDGE_LOOP ( 'NONE', ( #8317, #23284, #11198, #11778 ) ) ;
#23556 = CARTESIAN_POINT ( 'NONE',  ( 0.000000000000000000, -56.78056608349999834, 0.000000000000000000 ) ) ;
#23557 = CARTESIAN_POINT ( 'NONE',  ( -7.435983481029870390, -74.13941005069941070, -39.48497135291631821 ) ) ;
#23558 = EDGE_LOOP ( 'NONE', ( #5860, #28357, #11584, #9068 ) ) ;
#23559 = CARTESIAN_POINT ( 'NONE',  ( 7.727581852389999284, -65.07443093669999712, -23.93312597839999967 ) ) ;
#23560 = CARTESIAN_POINT ( 'NONE',  ( 8.969779973459999667, -35.75711592580000087, -20.13916512639999823 ) ) ;
#23561 = CARTESIAN_POINT ( 'NONE',  ( 40.00441865787361451, -74.28334043028284839, 7.315281844182966786 ) ) ;
#23562 = ORIENTED_EDGE ( 'NONE', *, *, #203, .F. ) ;
#23563 = CARTESIAN_POINT ( 'NONE',  ( -14.69223322520000075, -101.0355888259999944, 4.860466037580000176 ) ) ;
#23564 = CARTESIAN_POINT ( 'NONE',  ( -15.58109701669999936, -101.5369810459999940, 3.638540083340000120 ) ) ;
#23565 = CARTESIAN_POINT ( 'NONE',  ( -32.31206904232557520, -74.05059202417167796, -22.10200946381351628 ) ) ;
#23566 = CARTESIAN_POINT ( 'NONE',  ( -19.86043801069999759, -60.48530148380000071, 13.73936412299999965 ) ) ;
#23567 = ORIENTED_EDGE ( 'NONE', *, *, #16219, .F. ) ;
#23568 = CARTESIAN_POINT ( 'NONE',  ( 20.42441471257877694, -98.07255008151754794, -1.452410518408777884 ) ) ;
#23569 = DIRECTION ( 'NONE',  ( 0.000000000000000000, -1.000000000000000000, 0.000000000000000000 ) ) ;
#23570 = CARTESIAN_POINT ( 'NONE',  ( -2.741827583460000106, -18.87168151170000030, -24.31677564899999666 ) ) ;
#23571 = CARTESIAN_POINT ( 'NONE',  ( 9.348798002780000616, -10.50000000000000000, 17.11285995690000306 ) ) ;
#23572 = ORIENTED_EDGE ( 'NONE', *, *, #1875, .T. ) ;
#23573 = CARTESIAN_POINT ( 'NONE',  ( 0.000000000000000000, -92.50000000000000000, 0.000000000000000000 ) ) ;
#23574 = CARTESIAN_POINT ( 'NONE',  ( 36.49642319969999704, -79.41084811649999153, -14.73518963879999966 ) ) ;
#23575 = VERTEX_POINT ( 'NONE', #17166 ) ;
#23576 = EDGE_CURVE ( 'NONE', #12207, #28514, #27908, .T. ) ;
#23577 = CARTESIAN_POINT ( 'NONE',  ( 6.880390998654439372, -100.3041487039077992, 15.60897913166483519 ) ) ;
#23578 = CARTESIAN_POINT ( 'NONE',  ( 8.852567479250000204, -98.72068567929999006, 16.20451607640000091 ) ) ;
#23579 = ADVANCED_FACE ( 'NONE', ( #8143 ), #2469, .F. ) ;
#23580 = VERTEX_POINT ( 'NONE', #14962 ) ;
#23581 = B_SPLINE_CURVE_WITH_KNOTS ( 'NONE', 5,
 ( #229, #24091, #6171, #15045, #23958, #21766 ),
 .UNSPECIFIED., .F., .F.,
 ( 6, 6 ),
 ( 0.000000000000000000, 1.000000000000000000 ),
 .UNSPECIFIED. ) ;
#23582 = CARTESIAN_POINT ( 'NONE',  ( -18.62868452085797344, -97.90567604392204260, 5.830860830108250070 ) ) ;
#23583 = ORIENTED_EDGE ( 'NONE', *, *, #16712, .T. ) ;
#23584 = CARTESIAN_POINT ( 'NONE',  ( 29.41463188180000188, -92.63555401869999173, 7.090046362370000743 ) ) ;
#23585 = DIRECTION ( 'NONE',  ( 0.000000000000000000, -1.000000000000000000, 0.000000000000000000 ) ) ;
#23586 = CARTESIAN_POINT ( 'NONE',  ( -5.811429032009999496, -101.0314399550000104, 14.75160927930000021 ) ) ;
#23587 = EDGE_CURVE ( 'NONE', #13587, #9278, #8029, .T. ) ;
#23588 = ORIENTED_EDGE ( 'NONE', *, *, #15571, .T. ) ;
#23589 = CARTESIAN_POINT ( 'NONE',  ( -0.8008942093612425595, -98.99956643305974069, -18.58022514274053094 ) ) ;
#23590 = CARTESIAN_POINT ( 'NONE',  ( 7.356933064080000584, -36.56811125840000187, -21.47791245320000186 ) ) ;
#23591 = CARTESIAN_POINT ( 'NONE',  ( 8.597788217099999741, -37.95525409580000087, -21.87044398639999798 ) ) ;
#23592 = CARTESIAN_POINT ( 'NONE',  ( 16.79922297439999923, -99.53431386179998697, 4.586272525910000120 ) ) ;
#23593 = CARTESIAN_POINT ( 'NONE',  ( 25.58626617267352898, -68.16965135175686896, 10.86867477486674183 ) ) ;
#23594 = ORIENTED_EDGE ( 'NONE', *, *, #25055, .F. ) ;
#23595 = FACE_OUTER_BOUND ( 'NONE', #1370, .T. ) ;
#23596 = CARTESIAN_POINT ( 'NONE',  ( 16.76165095789999882, -99.73367660430000115, 4.320137484619999135 ) ) ;
#23597 = DIRECTION ( 'NONE',  ( 0.000000000000000000, 1.000000000000000000, 0.000000000000000000 ) ) ;
#23598 = CARTESIAN_POINT ( 'NONE',  ( 24.02750282179999886, -93.67384740789999853, -8.937547196530001514 ) ) ;
#23599 = CARTESIAN_POINT ( 'NONE',  ( -2.493447086729999818, -53.79621871020000157, -24.52592544210000014 ) ) ;
#23600 = CARTESIAN_POINT ( 'NONE',  ( 0.000000000000000000, -107.5000000000000000, 0.000000000000000000 ) ) ;
#23601 = CARTESIAN_POINT ( 'NONE',  ( -27.18988201479999844, -32.89844555429999673, -49.77074518290000071 ) ) ;
#23602 = ORIENTED_EDGE ( 'NONE', *, *, #3564, .T. ) ;
#23603 = CARTESIAN_POINT ( 'NONE',  ( -15.43525743989999910, -101.1461852590000063, 4.782895807790000120 ) ) ;
#23604 = DIRECTION ( 'NONE',  ( 0.8775825618903722036, 0.000000000000000000, -0.4794255386042041156 ) ) ;
#23605 = CARTESIAN_POINT ( 'NONE',  ( 16.83483077069999823, -99.92967571559999840, 4.239603657359999112 ) ) ;
#23606 = CARTESIAN_POINT ( 'NONE',  ( 30.54128691159999676, -72.68262309459998960, -23.69343438309999783 ) ) ;
#23607 = LINE ( 'NONE', #3651, #13631 ) ;
#23608 = AXIS2_PLACEMENT_3D ( 'NONE', #8845, #17609, #4349 ) ;
#23609 = CIRCLE ( 'NONE', #13360, 7.750000000000000000 ) ;
#23610 = EDGE_CURVE ( 'NONE', #28111, #8881, #15452, .T. ) ;
#23611 = AXIS2_PLACEMENT_3D ( 'NONE', #14575, #26225, #10321 ) ;
#23612 = ADVANCED_FACE ( 'NONE', ( #12633 ), #17811, .F. ) ;
#23613 = VERTEX_POINT ( 'NONE', #24011 ) ;
#23614 = DIRECTION ( 'NONE',  ( -0.4151946956541399669, 0.5000000000001689759, -0.7600087925152558821 ) ) ;
#23615 = CARTESIAN_POINT ( 'NONE',  ( -40.70731707320000226, -74.50000000000000000, -7.215414233289999757 ) ) ;
#23616 = AXIS2_PLACEMENT_3D ( 'NONE', #8160, #12791, #23746 ) ;
#23617 = CARTESIAN_POINT ( 'NONE',  ( 21.48062417799999935, -36.74237083870000475, -7.706980317549999349 ) ) ;
#23618 = PLANE ( 'NONE',  #23271 ) ;
#23619 = EDGE_CURVE ( 'NONE', #25273, #2951, #10327, .T. ) ;
#23620 = ORIENTED_EDGE ( 'NONE', *, *, #10399, .T. ) ;
#23621 = CARTESIAN_POINT ( 'NONE',  ( 10.69681779260000098, -97.83805864369999483, 16.80092975179999826 ) ) ;
#23622 = EDGE_CURVE ( 'NONE', #26675, #16955, #6189, .T. ) ;
#23623 = B_SPLINE_SURFACE_WITH_KNOTS ( 'NONE', 5, 5, ( 
 ( #4277, #28734, #6169, #13002, #4127, #19431 ),
 ( #21912, #24526, #3990, #13295, #22199, #28315 ),
 ( #2243, #20004, #8771, #1962, #74, #8350 ),
 ( #19716, #17251, #2110, #26291, #28603, #26144 ),
 ( #12849, #10660, #19575, #28461, #8498, #17398 ),
 ( #6316, #15324, #13152, #22062, #10944, #27456 ),
 ( #22945, #24971, #20605, #26868, #4865, #24827 ),
 ( #18564, #15922, #7505, #15771, #5158, #14039 ),
 ( #11845, #18418, #27307, #17976, #13747, #9368 ) ),
 .UNSPECIFIED., .F., .F., .F.,
 ( 6, 3, 6 ),
 ( 6, 6 ),
 ( 3.884102134650000319E-15, 2.251105814029999763, 5.576980695509999642 ),
 ( 0.000000000000000000, 1.000000000000000000 ),
 .UNSPECIFIED. ) ;
#23624 = CARTESIAN_POINT ( 'NONE',  ( -15.08595480590000015, -92.80303298520000510, -23.69775107969999794 ) ) ;
#23625 = CARTESIAN_POINT ( 'NONE',  ( -8.119791933969999320, -99.97545561319999763, 14.82168165659999914 ) ) ;
#23626 = ORIENTED_EDGE ( 'NONE', *, *, #16219, .T. ) ;
#23627 = CARTESIAN_POINT ( 'NONE',  ( 0.05992568041179999888, -93.49005502529999490, 26.18698436240000049 ) ) ;
#23628 = CARTESIAN_POINT ( 'NONE',  ( 9.720255118479999012, -72.82938648530000592, -26.98670296669999757 ) ) ;
#23629 = CARTESIAN_POINT ( 'NONE',  ( 11.76103934369071702, -98.56104011604492143, -15.97798918033824656 ) ) ;
#23630 = ORIENTED_EDGE ( 'NONE', *, *, #21202, .T. ) ;
#23631 = AXIS2_PLACEMENT_3D ( 'NONE', #96, #8368, #11868 ) ;
#23632 = CARTESIAN_POINT ( 'NONE',  ( 13.64952044873572312, -100.3796496172744668, -10.12948479266517232 ) ) ;
#23633 = CARTESIAN_POINT ( 'NONE',  ( -22.25450259269999975, -94.89197151650000706, -8.089821617090001027 ) ) ;
#23634 = CARTESIAN_POINT ( 'NONE',  ( 10.27467259300000002, -95.70830610299999819, -20.00247075010000231 ) ) ;
#23635 = EDGE_LOOP ( 'NONE', ( #18867, #550, #8210, #1170 ) ) ;
#23636 = DIRECTION ( 'NONE',  ( 1.000000000000000000, 0.000000000000000000, 0.000000000000000000 ) ) ;
#23637 = CARTESIAN_POINT ( 'NONE',  ( -14.14106740610000124, -74.03779068149999887, 36.36621500920000472 ) ) ;
#23638 = CARTESIAN_POINT ( 'NONE',  ( -18.19849796460000135, -94.71480814230000078, 16.19177224499999923 ) ) ;
#23639 = CARTESIAN_POINT ( 'NONE',  ( -16.77460173512971053, -92.92035260009522801, 25.47427353929137439 ) ) ;
#23640 = EDGE_LOOP ( 'NONE', ( #28145, #4437, #16985, #18550 ) ) ;
#23641 = CARTESIAN_POINT ( 'NONE',  ( -0.5663699853978287901, -74.35139840166131364, 47.23114592678867041 ) ) ;
#23642 = TOROIDAL_SURFACE ( 'NONE', #4074, 15.50000000000000000, 0.5000000000000000000 ) ;
#23643 = CARTESIAN_POINT ( 'NONE',  ( -0.08783699053769999932, -101.6484611540000031, -16.00001271889999899 ) ) ;
#23644 = LINE ( 'NONE', #25702, #27278 ) ;
#23645 = CARTESIAN_POINT ( 'NONE',  ( 15.58784579500000156, -100.8733988930000010, 2.070706579690000382 ) ) ;
#23646 = DIRECTION ( 'NONE',  ( 1.000000000000000000, 0.000000000000000000, 0.000000000000000000 ) ) ;
#23647 = CARTESIAN_POINT ( 'NONE',  ( 47.25000000000000000, -74.00000000000000000, 0.000000000000000000 ) ) ;
#23648 = ORIENTED_EDGE ( 'NONE', *, *, #3385, .F. ) ;
#23649 = CARTESIAN_POINT ( 'NONE',  ( 6.321364180049999781, -100.1512121650000040, 15.39199192900000135 ) ) ;
#23650 = CARTESIAN_POINT ( 'NONE',  ( 15.66067906339999816, -101.4829589650000088, 3.855162640470000124 ) ) ;
#23651 = EDGE_CURVE ( 'NONE', #11243, #24004, #8419, .T. ) ;
#23652 = CIRCLE ( 'NONE', #19005, 53.35000000000000142 ) ;
#23653 = AXIS2_PLACEMENT_3D ( 'NONE', #21909, #4273, #10804 ) ;
#23654 = CARTESIAN_POINT ( 'NONE',  ( -32.83566817730000054, -74.50000000000000000, -22.22906645950000026 ) ) ;
#23655 = FACE_OUTER_BOUND ( 'NONE', #16002, .T. ) ;
#23656 = CIRCLE ( 'NONE', #17137, 5.000000000000000888 ) ;
#23657 = DIRECTION ( 'NONE',  ( -1.000000000000000000, 0.000000000000000000, 0.000000000000000000 ) ) ;
#23658 = CARTESIAN_POINT ( 'NONE',  ( 8.985924787889999266, -94.36515553530000489, -23.15004553760000050 ) ) ;
#23659 = EDGE_CURVE ( 'NONE', #22021, #2012, #6680, .T. ) ;
#23660 = CARTESIAN_POINT ( 'NONE',  ( -15.92623219940000112, -93.13202907839999511, -20.96831028749999959 ) ) ;
#23661 = DIRECTION ( 'NONE',  ( 0.000000000000000000, 1.000000000000000000, 0.000000000000000000 ) ) ;
#23662 = VERTEX_POINT ( 'NONE', #18039 ) ;
#23663 = DIRECTION ( 'NONE',  ( 0.000000000000000000, -1.000000000000000000, 0.000000000000000000 ) ) ;
#23664 = B_SPLINE_CURVE_WITH_KNOTS ( 'NONE', 3,
 ( #27424, #22468, #3104, #18532, #339, #13859, #16182, #26987, #9041, #20271 ),
 .UNSPECIFIED., .F., .F.,
 ( 4, 2, 2, 2, 4 ),
 ( 0.000000000000000000, 0.2500000000000000000, 0.5000000000000000000, 0.7500000000000000000, 1.000000000000000000 ),
 .UNSPECIFIED. ) ;
#23665 = CYLINDRICAL_SURFACE ( 'NONE', #14550, 39.24999999999998579 ) ;
#23666 = ORIENTED_EDGE ( 'NONE', *, *, #17192, .T. ) ;
#23667 = CARTESIAN_POINT ( 'NONE',  ( 11.64589452461991037, -93.86980009079697140, -22.69836348088650979 ) ) ;
#23668 = CARTESIAN_POINT ( 'NONE',  ( -7.296770820709999938, -74.06388275500000873, 39.69120874740000460 ) ) ;
#23669 = DIRECTION ( 'NONE',  ( 0.8775825618903722036, 0.000000000000000000, -0.4794255386042041156 ) ) ;
#23670 = DIRECTION ( 'NONE',  ( 1.000000000000000000, 0.000000000000000000, 0.000000000000000000 ) ) ;
#23671 = CIRCLE ( 'NONE', #22758, 9.499999999999998224 ) ;
#23672 = CARTESIAN_POINT ( 'NONE',  ( 0.000000000000000000, -17.30000000000000071, 0.000000000000000000 ) ) ;
#23673 = AXIS2_PLACEMENT_3D ( 'NONE', #10379, #19017, #27897 ) ;
#23674 = CARTESIAN_POINT ( 'NONE',  ( 11.63343413870000020, -100.9405348700000076, -10.90407401050000047 ) ) ;
#23675 = CARTESIAN_POINT ( 'NONE',  ( -12.15457518680000071, -65.52795386159999680, -22.48391257200000126 ) ) ;
#23676 = CARTESIAN_POINT ( 'NONE',  ( 7.217842745160000462, -35.78513210170000036, -21.44331575660000055 ) ) ;
#23677 = DIRECTION ( 'NONE',  ( 1.000000000000000000, 0.000000000000000000, 0.000000000000000000 ) ) ;
#23678 = ORIENTED_EDGE ( 'NONE', *, *, #28239, .T. ) ;
#23679 = ORIENTED_EDGE ( 'NONE', *, *, #19693, .F. ) ;
#23680 = ADVANCED_FACE ( 'NONE', ( #15546 ), #6850, .T. ) ;
#23681 = DIRECTION ( 'NONE',  ( 0.4794255386042036715, 0.000000000000000000, 0.8775825618903724257 ) ) ;
#23682 = ADVANCED_FACE ( 'NONE', ( #19775 ), #28656, .F. ) ;
#23683 = CARTESIAN_POINT ( 'NONE',  ( -2.485331911600000332, -61.52579421249999569, -25.06050290059999952 ) ) ;
#23684 = TOROIDAL_SURFACE ( 'NONE', #4618, 12.00000000000000000, 1.000000000000000000 ) ;
#23685 = CARTESIAN_POINT ( 'NONE',  ( 9.322992499379999742, -37.99098076110000477, -22.72991278869999832 ) ) ;
#23686 = CARTESIAN_POINT ( 'NONE',  ( -29.29520252239999678, -92.62399497440000573, 4.740789425840000071 ) ) ;
#23687 = CARTESIAN_POINT ( 'NONE',  ( 9.370945656724327222, -94.71481465630654384, -22.48432281284479117 ) ) ;
#23688 = AXIS2_PLACEMENT_3D ( 'NONE', #7214, #27176, #244 ) ;
#23689 = AXIS2_PLACEMENT_3D ( 'NONE', #15245, #6537, #6833 ) ;
#23690 = AXIS2_PLACEMENT_3D ( 'NONE', #18028, #20065, #28793 ) ;
#23691 = AXIS2_PLACEMENT_3D ( 'NONE', #2802, #24648, #11656 ) ;
#23692 = VERTEX_POINT ( 'NONE', #13218 ) ;
#23693 = PLANE ( 'NONE',  #27484 ) ;
#23694 = ORIENTED_EDGE ( 'NONE', *, *, #15300, .T. ) ;
#23695 = CARTESIAN_POINT ( 'NONE',  ( 7.691701944196837282, -37.38596123215534561, -21.51611381909645715 ) ) ;
#23696 = ORIENTED_EDGE ( 'NONE', *, *, #8477, .T. ) ;
#23697 = CARTESIAN_POINT ( 'NONE',  ( -14.01337416149999981, -80.34292142019999972, 36.66316733609999545 ) ) ;
#23698 = CARTESIAN_POINT ( 'NONE',  ( -22.16250285911532814, -74.14342904296044878, -32.55991892830125778 ) ) ;
#23699 = CARTESIAN_POINT ( 'NONE',  ( 22.02359273509999937, -18.62181730670000235, 9.222605046309999111 ) ) ;
#23700 = CARTESIAN_POINT ( 'NONE',  ( -13.15133833870000046, -100.9197081840000010, -8.436152112259998503 ) ) ;
#23701 = CARTESIAN_POINT ( 'NONE',  ( -40.16286586133305292, -63.35496135697056275, 2.175426268797550744 ) ) ;
#23702 = EDGE_CURVE ( 'NONE', #5567, #24058, #4937, .T. ) ;
#23703 = ORIENTED_EDGE ( 'NONE', *, *, #7512, .T. ) ;
#23704 = CARTESIAN_POINT ( 'NONE',  ( -9.356041104380000917, -84.00000000000000000, 37.60355029590000697 ) ) ;
#23705 = CARTESIAN_POINT ( 'NONE',  ( -12.43113460380000035, -101.2902355740000075, -9.959137603120000293 ) ) ;
#23706 = CARTESIAN_POINT ( 'NONE',  ( -0.5590517731190000061, -18.50000000000000000, -21.02688049580000040 ) ) ;
#23707 = CARTESIAN_POINT ( 'NONE',  ( -7.459817445499475674, -101.2637735886632129, 14.49077341668773578 ) ) ;
#23708 = ORIENTED_EDGE ( 'NONE', *, *, #19178, .T. ) ;
#23709 = AXIS2_PLACEMENT_3D ( 'NONE', #23552, #25604, #27787 ) ;
#23710 = AXIS2_PLACEMENT_3D ( 'NONE', #23556, #14518, #19046 ) ;
#23711 = CARTESIAN_POINT ( 'NONE',  ( -41.50091764415566331, -65.12549727761340534, -2.878985763018412136 ) ) ;
#23712 = CARTESIAN_POINT ( 'NONE',  ( -41.76385502083800105, -65.70026997502756672, -1.401764440866061667 ) ) ;
#23713 = CARTESIAN_POINT ( 'NONE',  ( 36.67694313739999501, -80.46520755129999714, -13.97975614370000130 ) ) ;
#23714 = EDGE_LOOP ( 'NONE', ( #25259, #1217, #22691, #6832 ) ) ;
#23715 = EDGE_CURVE ( 'NONE', #14159, #5527, #3257, .T. ) ;
#23716 = EDGE_CURVE ( 'NONE', #7833, #26140, #2890, .T. ) ;
#23717 = DIRECTION ( 'NONE',  ( 0.4794255386042036715, 0.000000000000000000, 0.8775825618903724257 ) ) ;
#23718 = CARTESIAN_POINT ( 'NONE',  ( 6.947152782944919558, -100.1994045928328774, 15.67154092987886216 ) ) ;
#23719 = CARTESIAN_POINT ( 'NONE',  ( -7.215414233289999757, -77.00000000000000000, -40.70731707320000226 ) ) ;
#23720 = ORIENTED_EDGE ( 'NONE', *, *, #673, .T. ) ;
#23721 = DIRECTION ( 'NONE',  ( 0.000000000000000000, 1.000000000000000000, 0.000000000000000000 ) ) ;
#23722 = CARTESIAN_POINT ( 'NONE',  ( 47.16762437949999764, -74.53411049070001582, -1.089894286769999887 ) ) ;
#23723 = ORIENTED_EDGE ( 'NONE', *, *, #17670, .T. ) ;
#23724 = CARTESIAN_POINT ( 'NONE',  ( 23.11751862730000084, -56.19735282230000450, 10.36524394209999933 ) ) ;
#23725 = CARTESIAN_POINT ( 'NONE',  ( 20.82957722363834918, -36.00000000010000178, -9.510883242529262205 ) ) ;
#23726 = CARTESIAN_POINT ( 'NONE',  ( -7.135467526410000261, -73.65707963269998970, -38.71641004229999794 ) ) ;
#23727 = ORIENTED_EDGE ( 'NONE', *, *, #17302, .T. ) ;
#23728 = CARTESIAN_POINT ( 'NONE',  ( 13.88148934900000064, -99.91102932019998661, -9.687780287520000755 ) ) ;
#23729 = DIRECTION ( 'NONE',  ( 0.000000000000000000, -1.000000000000000000, 0.000000000000000000 ) ) ;
#23730 = AXIS2_PLACEMENT_3D ( 'NONE', #24709, #22377, #4450 ) ;
#23731 = CIRCLE ( 'NONE', #14875, 12.25068835559999947 ) ;
#23732 = FACE_OUTER_BOUND ( 'NONE', #28272, .T. ) ;
#23733 = CARTESIAN_POINT ( 'NONE',  ( -2.557399843751114954, -79.91561779696330348, 47.03678055220303378 ) ) ;
#23734 = VERTEX_POINT ( 'NONE', #7571 ) ;
#23735 = CARTESIAN_POINT ( 'NONE',  ( 25.12979114312568285, -65.01951069083045809, 0.1513711869631185758 ) ) ;
#23736 = CARTESIAN_POINT ( 'NONE',  ( 12.38736960600000003, -101.0403179300000005, -9.267121510750001789 ) ) ;
#23737 = DIRECTION ( 'NONE',  ( -0.7071067811865474617, 0.000000000000000000, -0.7071067811865474617 ) ) ;
#23738 = EDGE_CURVE ( 'NONE', #790, #19618, #25192, .T. ) ;
#23739 = CARTESIAN_POINT ( 'NONE',  ( 24.53124433849999875, -92.68289710869998999, -13.70463660470000100 ) ) ;
#23740 = VERTEX_POINT ( 'NONE', #14107 ) ;
#23741 = B_SPLINE_CURVE_WITH_KNOTS ( 'NONE', 3,
 ( #22669, #27189, #16093, #12422 ),
 .UNSPECIFIED., .F., .F.,
 ( 4, 4 ),
 ( 0.000000000000000000, 1.000000000000000000 ),
 .UNSPECIFIED. ) ;
#23742 = CARTESIAN_POINT ( 'NONE',  ( 29.71005176673471482, -92.93978723898561611, 6.896596330736053382 ) ) ;
#23743 = CARTESIAN_POINT ( 'NONE',  ( -18.28907245470000120, -18.50000000000000000, 14.67141105099999976 ) ) ;
#23744 = ORIENTED_EDGE ( 'NONE', *, *, #574, .T. ) ;
#23745 = DIRECTION ( 'NONE',  ( 0.000000000000000000, 1.000000000000000000, 0.000000000000000000 ) ) ;
#23746 = DIRECTION ( 'NONE',  ( 0.4794255386042042266, 0.000000000000000000, 0.8775825618903720926 ) ) ;
#23747 = CARTESIAN_POINT ( 'NONE',  ( 29.11677867130000052, -93.00000000000000000, 6.880015861159999524 ) ) ;
#23748 = CARTESIAN_POINT ( 'NONE',  ( 21.63858029419999696, -18.50000000000000000, 8.493246274499998805 ) ) ;
#23749 = ADVANCED_FACE ( 'NONE', ( #27525 ), #9435, .F. ) ;
#23750 = CARTESIAN_POINT ( 'NONE',  ( 26.61374759190000105, -73.81001964159999318, -28.89513312169999892 ) ) ;
#23751 = AXIS2_PLACEMENT_3D ( 'NONE', #14902, #8772, #12715 ) ;
#23752 = AXIS2_PLACEMENT_3D ( 'NONE', #16785, #14184, #1353 ) ;
#23753 = AXIS2_PLACEMENT_3D ( 'NONE', #26921, #11144, #24735 ) ;
#23754 = ADVANCED_BREP_SHAPE_REPRESENTATION ( '', ( #16071, #26433 ), #5492 ) ;
#23755 =( NAMED_UNIT ( * ) SI_UNIT ( $, .STERADIAN. ) SOLID_ANGLE_UNIT ( ) );
#23756 = ORIENTED_EDGE ( 'NONE', *, *, #993, .F. ) ;
#23757 = CARTESIAN_POINT ( 'NONE',  ( -39.83391879159715643, -73.87273571728266575, -7.248098695806580949 ) ) ;
#23758 = ORIENTED_EDGE ( 'NONE', *, *, #9646, .F. ) ;
#23759 = CARTESIAN_POINT ( 'NONE',  ( 20.97515210950000153, -36.16091267649999708, -8.638070979520000137 ) ) ;
#23760 = CARTESIAN_POINT ( 'NONE',  ( 9.151216319970000512, -35.87888623290000112, -19.56023227720000079 ) ) ;
#23761 = EDGE_LOOP ( 'NONE', ( #10582, #22908, #7707, #4098 ) ) ;
#23762 = CARTESIAN_POINT ( 'NONE',  ( 13.61159746509999913, -96.44392658620000702, 17.13483077990000325 ) ) ;
#23763 = FACE_BOUND ( 'NONE', #27597, .T. ) ;
#23764 = CARTESIAN_POINT ( 'NONE',  ( -7.887657129469999973, -99.88067631459999518, 15.44459931949999998 ) ) ;
#23765 = CARTESIAN_POINT ( 'NONE',  ( -3.215500290640000536, -94.59276479679999738, 23.57860595660000058 ) ) ;
#23766 = CARTESIAN_POINT ( 'NONE',  ( 7.992697997670000554, -57.47158989559999753, -22.16162922080000186 ) ) ;
#23767 = CIRCLE ( 'NONE', #22386, 5.500000000000000000 ) ;
#23768 = ORIENTED_EDGE ( 'NONE', *, *, #4464, .F. ) ;
#23769 = AXIS2_PLACEMENT_3D ( 'NONE', #8131, #22251, #11148 ) ;
#23770 = DIRECTION ( 'NONE',  ( -0.8775825618903722036, 0.000000000000000000, 0.4794255386042041156 ) ) ;
#23771 = TOROIDAL_SURFACE ( 'NONE', #13534, 10.50000000000000000, 0.5000000000000000000 ) ;
#23772 = CARTESIAN_POINT ( 'NONE',  ( 22.38048301969999798, -27.06679042429999882, 0.1658473372300000026 ) ) ;
#23773 = DIRECTION ( 'NONE',  ( 1.000000000000000000, 0.000000000000000000, 0.000000000000000000 ) ) ;
#23774 = ORIENTED_EDGE ( 'NONE', *, *, #5385, .T. ) ;
#23775 = CARTESIAN_POINT ( 'NONE',  ( 19.35192606849999919, -18.86754463369999968, -8.857879772089999548 ) ) ;
#23776 = CIRCLE ( 'NONE', #11190, 53.75557630320000868 ) ;
#23777 = EDGE_CURVE ( 'NONE', #3830, #10282, #25301, .T. ) ;
#23778 = CARTESIAN_POINT ( 'NONE',  ( -14.40064467200000209, -74.16918790970001396, 36.61749309489999860 ) ) ;
#23779 = CARTESIAN_POINT ( 'NONE',  ( -17.45201720579999716, -93.65993419859999847, 18.14866333539999843 ) ) ;
#23780 = LINE ( 'NONE', #26261, #23796 ) ;
#23781 = ORIENTED_EDGE ( 'NONE', *, *, #24472, .T. ) ;
#23782 = EDGE_CURVE ( 'NONE', #6426, #17770, #11299, .T. ) ;
#23783 = FACE_OUTER_BOUND ( 'NONE', #1536, .T. ) ;
#23784 = B_SPLINE_CURVE_WITH_KNOTS ( 'NONE', 5,
 ( #12931, #10885, #15116, #1898, #19650, #21565, #19795, #14981, #15257 ),
 .UNSPECIFIED., .F., .F.,
 ( 6, 3, 6 ),
 ( 0.000000000000000000, 1.237573681330000008, 1.566718891470000097 ),
 .UNSPECIFIED. ) ;
#23785 = CARTESIAN_POINT ( 'NONE',  ( 26.77683864449999973, -33.79999999999999716, 49.01467436490000296 ) ) ;
#23786 = CARTESIAN_POINT ( 'NONE',  ( 7.999569604760000452, -65.05903923030000158, -23.83793848660000236 ) ) ;
#23787 = CARTESIAN_POINT ( 'NONE',  ( -13.18623751009999978, -69.39685719070000403, -23.69831535020000146 ) ) ;
#23788 = EDGE_CURVE ( 'NONE', #15502, #25637, #9719, .T. ) ;
#23789 = CARTESIAN_POINT ( 'NONE',  ( 23.14416773940000027, -57.40875670289999988, 10.37855713959999981 ) ) ;
#23790 = CARTESIAN_POINT ( 'NONE',  ( -10.84622327880000014, -27.00851495050000040, -21.73428641559999974 ) ) ;
#23791 = ORIENTED_EDGE ( 'NONE', *, *, #27656, .F. ) ;
#23792 = ADVANCED_FACE ( 'NONE', ( #24894 ), #12190, .F. ) ;
#23793 = CARTESIAN_POINT ( 'NONE',  ( 6.355965434729999863, -99.91102932029998840, 15.68918534660000041 ) ) ;
#23794 = CARTESIAN_POINT ( 'NONE',  ( 15.61571272419999978, -101.4908759489999994, 3.625172433619999968 ) ) ;
#23795 = CARTESIAN_POINT ( 'NONE',  ( 7.286238495500000134, -101.2500498790000023, 13.33737010350000141 ) ) ;
#23796 = VECTOR ( 'NONE', #28284, 1000.000000000000000 ) ;
#23797 = CIRCLE ( 'NONE', #27054, 9.500000000000001776 ) ;
#23798 = AXIS2_PLACEMENT_3D ( 'NONE', #4612, #18164, #20202 ) ;
#23799 = CARTESIAN_POINT ( 'NONE',  ( 8.963581071920001975, -35.44265712969999527, -20.01429396089999813 ) ) ;
#23800 = CARTESIAN_POINT ( 'NONE',  ( 21.09786747150000252, -18.50000000000000000, 0.1832040240040000156 ) ) ;
#23801 = CARTESIAN_POINT ( 'NONE',  ( -7.371671982299999648, -98.73889367950000917, 17.11857524030000022 ) ) ;
#23802 = ORIENTED_EDGE ( 'NONE', *, *, #8790, .T. ) ;
#23803 = CARTESIAN_POINT ( 'NONE',  ( 8.558247864140000161, -94.18458606759999441, -22.78405818970000141 ) ) ;
#23804 = CARTESIAN_POINT ( 'NONE',  ( 0.000000000000000000, -91.50000000000000000, 0.000000000000000000 ) ) ;
#23805 = CARTESIAN_POINT ( 'NONE',  ( -6.871575534529999807, -101.3138676899999950, 14.35405997169999814 ) ) ;
#23806 = ORIENTED_EDGE ( 'NONE', *, *, #20137, .F. ) ;
#23807 = CARTESIAN_POINT ( 'NONE',  ( -29.86363316589999783, -101.1889999979999999, 0.3450520983969999622 ) ) ;
#23808 = ORIENTED_EDGE ( 'NONE', *, *, #297, .F. ) ;
#23809 = CARTESIAN_POINT ( 'NONE',  ( -1.604079331969999966, -100.9197086960000007, -15.54198441969999855 ) ) ;
#23810 = CARTESIAN_POINT ( 'NONE',  ( -38.71640881029999548, -73.50000064450000536, -7.135467304789999687 ) ) ;
#23811 = CARTESIAN_POINT ( 'NONE',  ( 36.62466543095905536, -74.65121096129686862, -14.68734462481934600 ) ) ;
#23812 = FACE_OUTER_BOUND ( 'NONE', #2907, .T. ) ;
#23813 = CIRCLE ( 'NONE', #14497, 16.00000000000000000 ) ;
#23814 = CARTESIAN_POINT ( 'NONE',  ( 16.19996591404212793, -94.70212264478905695, 17.23798455394816287 ) ) ;
#23815 = ADVANCED_FACE ( 'NONE', ( #18338 ), #19215, .F. ) ;
#23816 = DIRECTION ( 'NONE',  ( 0.000000000000000000, 1.000000000000000000, 0.000000000000000000 ) ) ;
#23817 = CARTESIAN_POINT ( 'NONE',  ( 46.25000000000000000, -75.00000000000000000, -13.75000000000000000 ) ) ;
#23818 = CARTESIAN_POINT ( 'NONE',  ( -18.68796107978499776, -19.47636826820795264, 13.44054024894182042 ) ) ;
#23819 = CARTESIAN_POINT ( 'NONE',  ( -10.50797418640000025, -18.50000000000000000, 18.24753908359999954 ) ) ;
#23820 = VERTEX_POINT ( 'NONE', #22710 ) ;
#23821 = ADVANCED_FACE ( 'NONE', ( #2752 ), #7267, .F. ) ;
#23822 = CARTESIAN_POINT ( 'NONE',  ( 8.522376746440000872, -19.16582662329999920, -20.19515292700000231 ) ) ;
#23823 = ORIENTED_EDGE ( 'NONE', *, *, #26072, .T. ) ;
#23824 = CARTESIAN_POINT ( 'NONE',  ( -40.00000000000000000, -74.50000000000000000, 2.464695114669999848E-15 ) ) ;
#23825 = EDGE_LOOP ( 'NONE', ( #8065, #28096, #3373, #25969 ) ) ;
#23826 = CARTESIAN_POINT ( 'NONE',  ( 6.948750312308070498, -36.56992522833583337, -21.53806854013285133 ) ) ;
#23827 = B_SPLINE_CURVE_WITH_KNOTS ( 'NONE', 3,
 ( #18832, #18538, #11518, #20425 ),
 .UNSPECIFIED., .F., .F.,
 ( 4, 4 ),
 ( 0.000000000000000000, 1.000000000000000000 ),
 .UNSPECIFIED. ) ;
#23828 = DIRECTION ( 'NONE',  ( 1.000000000000000000, 0.000000000000000000, 1.110223024629999160E-15 ) ) ;
#23829 = AXIS2_PLACEMENT_3D ( 'NONE', #22219, #9093, #9235 ) ;
#23830 = DIRECTION ( 'NONE',  ( 1.000000000000000000, 0.000000000000000000, 0.000000000000000000 ) ) ;
#23831 = CARTESIAN_POINT ( 'NONE',  ( 15.63315392260000003, -100.5027207520000019, 4.441352150160000178 ) ) ;
#23832 = ORIENTED_EDGE ( 'NONE', *, *, #9403, .F. ) ;
#23833 = CARTESIAN_POINT ( 'NONE',  ( 21.49951961919999732, -36.15937190469999507, -7.044630138860000557 ) ) ;
#23834 = VERTEX_POINT ( 'NONE', #15174 ) ;
#23835 = DIRECTION ( 'NONE',  ( 0.8775825618903722036, 0.000000000000000000, -0.4794255386042041156 ) ) ;
#23836 = CARTESIAN_POINT ( 'NONE',  ( -14.25825325729999982, -80.34252531600000680, 36.56956972409999906 ) ) ;
#23837 = CARTESIAN_POINT ( 'NONE',  ( -7.550578184249999047, -94.89197151660000884, -22.44319203070000057 ) ) ;
#23838 = ADVANCED_FACE ( 'NONE', ( #13147 ), #28730, .T. ) ;
#23839 = CARTESIAN_POINT ( 'NONE',  ( -14.99618466630000135, -101.1411470330000100, 3.458522314510000140 ) ) ;
#23840 = CARTESIAN_POINT ( 'NONE',  ( -32.79293189096514283, -74.34878806649766148, -22.21871444800659035 ) ) ;
#23841 = CARTESIAN_POINT ( 'NONE',  ( -20.56018215729999810, -57.40875686090000585, 14.85415973970000003 ) ) ;
#23842 = VERTEX_POINT ( 'NONE', #27933 ) ;
#23843 = AXIS2_PLACEMENT_3D ( 'NONE', #19761, #9385, #24986 ) ;
#23844 = CIRCLE ( 'NONE', #28058, 39.25000000000000000 ) ;
#23845 = CARTESIAN_POINT ( 'NONE',  ( 16.94740002120616396, -100.7167551730822908, 1.805771684632079488 ) ) ;
#23846 = CARTESIAN_POINT ( 'NONE',  ( -12.51867210719999868, -101.6311724339999927, -9.986052846930000726 ) ) ;
#23847 = CIRCLE ( 'NONE', #21094, 4.999999999999997335 ) ;
#23848 = CARTESIAN_POINT ( 'NONE',  ( 26.37318901919999803, -93.00000450890000536, 13.16123549989999830 ) ) ;
#23849 = CARTESIAN_POINT ( 'NONE',  ( -7.902774248908001731, -100.3796496173660131, 15.04865541543737351 ) ) ;
#23850 = ORIENTED_EDGE ( 'NONE', *, *, #12962, .F. ) ;
#23851 = ADVANCED_FACE ( 'NONE', ( #8768 ), #12457, .T. ) ;
#23852 = CARTESIAN_POINT ( 'NONE',  ( -0.7205257401540000606, -101.6484611540000031, -15.98376809950000066 ) ) ;
#23853 = CARTESIAN_POINT ( 'NONE',  ( -32.08679448059999828, -74.00994675159999758, -21.96941954280000076 ) ) ;
#23854 = CARTESIAN_POINT ( 'NONE',  ( 36.29172732829999859, -79.24889011169999264, -14.94947765220000058 ) ) ;
#23855 = ORIENTED_EDGE ( 'NONE', *, *, #26895, .F. ) ;
#23856 = B_SPLINE_SURFACE_WITH_KNOTS ( 'NONE', 5, 5, ( 
 ( #1465, #14964, #12778, #6237, #21827, #1883 ),
 ( #10721, #19635, #14698, #17463, #26349, #15241 ),
 ( #24160, #4194, #1325, #10167, #19086, #23591 ),
 ( #8009, #3635, #9286, #22265, #2313, #11166 ),
 ( #24452, #21978, #19777, #11321, #8690, #15844 ),
 ( #20369, #13362, #20080, #27083, #24305, #20225 ) ),
 .UNSPECIFIED., .F., .F., .F.,
 ( 6, 6 ),
 ( 6, 6 ),
 ( 2.709627234730000112, 3.225498864409999999 ),
 ( 0.000000000000000000, 2.000000000000000000 ),
 .UNSPECIFIED. ) ;
#23857 = AXIS2_PLACEMENT_3D ( 'NONE', #18834, #28125, #27723 ) ;
#23858 = CARTESIAN_POINT ( 'NONE',  ( 36.70830968599999977, -79.00000000000000000, -14.75000000000000000 ) ) ;
#23859 = CARTESIAN_POINT ( 'NONE',  ( 7.003224168222498491, -100.1240332945425564, 15.71316356361139910 ) ) ;
#23860 = CARTESIAN_POINT ( 'NONE',  ( -3.306822307565103536, -80.49999980012920275, 46.45859196424991211 ) ) ;
#23861 = ORIENTED_EDGE ( 'NONE', *, *, #17570, .F. ) ;
#23862 = ADVANCED_FACE ( 'NONE', ( #15318 ), #27631, .T. ) ;
#23863 = DIRECTION ( 'NONE',  ( 0.000000000000000000, -1.000000000000000000, 0.000000000000000000 ) ) ;
#23864 = CARTESIAN_POINT ( 'NONE',  ( 46.60312383370383316, -73.73419539363156616, -2.997193309239198467 ) ) ;
#23865 = VERTEX_POINT ( 'NONE', #19847 ) ;
#23866 = AXIS2_PLACEMENT_3D ( 'NONE', #27793, #3325, #8108 ) ;
#23867 = CARTESIAN_POINT ( 'NONE',  ( 28.45101619980000152, -92.62399496609999971, 8.439409298800001125 ) ) ;
#23868 = CARTESIAN_POINT ( 'NONE',  ( 47.25000000000000000, -75.00000000000000000, -7.375000000000000000 ) ) ;
#23869 = CARTESIAN_POINT ( 'NONE',  ( -35.50000000000000000, -63.00000000000000000, 0.000000000000000000 ) ) ;
#23870 = ORIENTED_EDGE ( 'NONE', *, *, #25528, .F. ) ;
#23871 = AXIS2_PLACEMENT_3D ( 'NONE', #21866, #4084, #12953 ) ;
#23872 = FACE_BOUND ( 'NONE', #16787, .T. ) ;
#23873 = CARTESIAN_POINT ( 'NONE',  ( 6.015370493379999656E-15, -69.00000000000000000, -40.00000000000000000 ) ) ;
#23874 = ORIENTED_EDGE ( 'NONE', *, *, #15531, .T. ) ;
#23875 = DIRECTION ( 'NONE',  ( 0.000000000000000000, -1.000000000000000000, 0.000000000000000000 ) ) ;
#23876 = CARTESIAN_POINT ( 'NONE',  ( -42.52792552673321325, -63.24690319806013150, 0.5612274588118402185 ) ) ;
#23877 = CARTESIAN_POINT ( 'NONE',  ( -22.01409729879999944, -92.76004107139999633, -20.03404935359999683 ) ) ;
#23878 = DIRECTION ( 'NONE',  ( 1.000000000000000000, 0.000000000000000000, 0.000000000000000000 ) ) ;
#23879 = ORIENTED_EDGE ( 'NONE', *, *, #1489, .T. ) ;
#23880 = CARTESIAN_POINT ( 'NONE',  ( -40.00000000000000000, -66.00000000000000000, 0.000000000000000000 ) ) ;
#23881 = ADVANCED_FACE ( 'NONE', ( #26425 ), #2439, .T. ) ;
#23882 = CARTESIAN_POINT ( 'NONE',  ( 12.73439086970000034, -101.3878691800000098, -9.855841448820001460 ) ) ;
#23883 = DIRECTION ( 'NONE',  ( 0.000000000000000000, 1.000000000000000000, 0.000000000000000000 ) ) ;
#23884 = CARTESIAN_POINT ( 'NONE',  ( 24.71445532999999983, -93.30149055180000062, -11.27282922470000237 ) ) ;
#23885 = CARTESIAN_POINT ( 'NONE',  ( -0.5350069560319999917, -53.84434310269999457, -23.22809113779999990 ) ) ;
#23886 = AXIS2_PLACEMENT_3D ( 'NONE', #3714, #28318, #7948 ) ;
#23887 = CARTESIAN_POINT ( 'NONE',  ( 10.27942207598835012, -72.70273852363769151, -26.82731210389089327 ) ) ;
#23888 = DIRECTION ( 'NONE',  ( 0.000000000000000000, 1.000000000000000000, 0.000000000000000000 ) ) ;
#23889 = ORIENTED_EDGE ( 'NONE', *, *, #5502, .T. ) ;
#23890 = CARTESIAN_POINT ( 'NONE',  ( 2.042810365310000056E-12, -74.50000000000000000, -2.458477865729999957E-12 ) ) ;
#23891 = CARTESIAN_POINT ( 'NONE',  ( -19.11827583450000034, -19.41837863929999841, 14.08667248819999962 ) ) ;
#23892 = CARTESIAN_POINT ( 'NONE',  ( 23.58466923419999972, -94.98812477769999418, -2.405350023570000051 ) ) ;
#23893 = CARTESIAN_POINT ( 'NONE',  ( 22.43858155039999858, -18.50000000000000000, 8.750340092050000962 ) ) ;
#23894 = CARTESIAN_POINT ( 'NONE',  ( -39.18882116139999994, -65.49083508809999898, 2.489060262989999828 ) ) ;
#23895 = VECTOR ( 'NONE', #2726, 1000.000000000000114 ) ;
#23896 = VERTEX_POINT ( 'NONE', #28007 ) ;
#23897 = CIRCLE ( 'NONE', #25391, 3.750000000000000000 ) ;
#23898 = EDGE_CURVE ( 'NONE', #87, #11019, #12682, .T. ) ;
#23899 = CARTESIAN_POINT ( 'NONE',  ( -11.85289063449999958, -94.98812477599999227, -21.44324726029999795 ) ) ;
#23900 = ORIENTED_EDGE ( 'NONE', *, *, #1043, .T. ) ;
#23901 = CIRCLE ( 'NONE', #207, 0.3500000000000003664 ) ;
#23902 = CARTESIAN_POINT ( 'NONE',  ( 19.85335301099999938, -35.79755265089999483, -9.067520686860000012 ) ) ;
#23903 = CARTESIAN_POINT ( 'NONE',  ( 9.212446728010000641, -35.92148816550000134, -19.60212694180000170 ) ) ;
#23904 = ORIENTED_EDGE ( 'NONE', *, *, #2488, .F. ) ;
#23905 = CARTESIAN_POINT ( 'NONE',  ( 10.64217894839999978, -97.74063293919999751, 16.82202129059999862 ) ) ;
#23906 = CARTESIAN_POINT ( 'NONE',  ( -16.08644287450000121, -92.54349754189999544, -23.90073121629999875 ) ) ;
#23907 = CARTESIAN_POINT ( 'NONE',  ( -8.247318090510001198, -99.72202992580000114, 15.06295020069999957 ) ) ;
#23908 = CARTESIAN_POINT ( 'NONE',  ( -1.709235988930000172, -93.75379239749999272, 24.88396779469999842 ) ) ;
#23909 = CARTESIAN_POINT ( 'NONE',  ( 20.36793921129758900, -34.63244748723148092, -8.805019764629991030 ) ) ;
#23910 = TOROIDAL_SURFACE ( 'NONE', #9505, 5.500000000000000000, 0.5000000000000000000 ) ;
#23911 = CARTESIAN_POINT ( 'NONE',  ( -34.11790219230000076, -80.00000000000000000, -24.21840725559999896 ) ) ;
#23912 = CARTESIAN_POINT ( 'NONE',  ( -18.88944331909999974, -111.0000000000000000, -23.13319212550000259 ) ) ;
#23913 = ORIENTED_EDGE ( 'NONE', *, *, #9345, .T. ) ;
#23914 = CARTESIAN_POINT ( 'NONE',  ( 12.77542149835405638, -101.4728631013604456, -9.856360518087987188 ) ) ;
#23915 = CARTESIAN_POINT ( 'NONE',  ( 23.99279226960000244, -42.23583340129999897, 1.251023842240000183 ) ) ;
#23916 = CARTESIAN_POINT ( 'NONE',  ( 23.67408170059999861, -68.20869413019998717, 12.08289283440000084 ) ) ;
#23917 = CARTESIAN_POINT ( 'NONE',  ( 9.108768065319999607, -94.52419709919999491, -22.22443129089999658 ) ) ;
#23918 = VERTEX_POINT ( 'NONE', #3124 ) ;
#23919 = DIRECTION ( 'NONE',  ( 1.000000000000000000, 0.000000000000000000, 0.000000000000000000 ) ) ;
#23920 = APPLICATION_CONTEXT ( 'automotive_design' ) ;
#23921 = DIRECTION ( 'NONE',  ( 0.000000000000000000, -1.000000000000000000, 0.000000000000000000 ) ) ;
#23922 = DIRECTION ( 'NONE',  ( 0.000000000000000000, 1.000000000000000000, 0.000000000000000000 ) ) ;
#23923 = CARTESIAN_POINT ( 'NONE',  ( -20.53694319417668268, -92.95475433444754287, 17.43128291165811916 ) ) ;
#23924 = ORIENTED_EDGE ( 'NONE', *, *, #23500, .T. ) ;
#23925 = CARTESIAN_POINT ( 'NONE',  ( 28.60859787209999894, -72.37489962920000153, 2.608048168490000318 ) ) ;
#23926 = AXIS2_PLACEMENT_3D ( 'NONE', #2062, #13252, #26526 ) ;
#23927 = DIRECTION ( 'NONE',  ( 1.000000000000000000, 0.000000000000000000, 0.000000000000000000 ) ) ;
#23928 = CARTESIAN_POINT ( 'NONE',  ( 8.613456916169999644, -58.97932910050000288, -22.38225487870000308 ) ) ;
#23929 = CARTESIAN_POINT ( 'NONE',  ( -12.23046582149999928, -69.33507195810000212, -24.60464239079999871 ) ) ;
#23930 = CARTESIAN_POINT ( 'NONE',  ( 22.73387075099999777, -60.10032509980000270, 10.25825663050000003 ) ) ;
#23931 = CARTESIAN_POINT ( 'NONE',  ( -11.11926074269999987, -19.46548176030000121, -19.02542913479999953 ) ) ;
#23932 = EDGE_LOOP ( 'NONE', ( #4280, #3260 ) ) ;
#23933 = CARTESIAN_POINT ( 'NONE',  ( 6.038481244350000665, -100.8023006570000035, 14.57509264930000015 ) ) ;
#23934 = CARTESIAN_POINT ( 'NONE',  ( 15.61329055410000066, -101.5216621940000152, 3.544188506249999815 ) ) ;
#23935 = AXIS2_PLACEMENT_3D ( 'NONE', #4876, #13165, #2403 ) ;
#23936 = CARTESIAN_POINT ( 'NONE',  ( 3.907985046679999924E-15, -73.50000000000000000, -40.00000000000000000 ) ) ;
#23937 = CARTESIAN_POINT ( 'NONE',  ( -40.00000000000000000, -79.00000000000000000, 0.000000000000000000 ) ) ;
#23938 = TOROIDAL_SURFACE ( 'NONE', #27693, 6.750000000000000000, 0.5000000000000000000 ) ;
#23939 = DIRECTION ( 'NONE',  ( 0.000000000000000000, -1.000000000000000000, 0.000000000000000000 ) ) ;
#23940 = ORIENTED_EDGE ( 'NONE', *, *, #13008, .T. ) ;
#23941 = CARTESIAN_POINT ( 'NONE',  ( 4.528887711649999481, -92.66001714109999909, -27.65183955359999857 ) ) ;
#23942 = ADVANCED_FACE ( 'NONE', ( #14035 ), #25739, .F. ) ;
#23943 = B_SPLINE_CURVE_WITH_KNOTS ( 'NONE', 5,
 ( #25312, #2724, #7544, #22539, #2584, #20487 ),
 .UNSPECIFIED., .F., .F.,
 ( 6, 6 ),
 ( 0.000000000000000000, 1.000000000000000000 ),
 .UNSPECIFIED. ) ;
#23944 = DIRECTION ( 'NONE',  ( 1.000000000000000000, 0.000000000000000000, 0.000000000000000000 ) ) ;
#23945 = CARTESIAN_POINT ( 'NONE',  ( -6.668573295719999905, -101.1716782170000073, 14.25075804799999979 ) ) ;
#23946 = ORIENTED_EDGE ( 'NONE', *, *, #8641, .T. ) ;
#23947 = CIRCLE ( 'NONE', #11867, 0.9999999999999996669 ) ;
#23948 = DIRECTION ( 'NONE',  ( 1.000000000000000000, 0.000000000000000000, 7.486357007659991815E-17 ) ) ;
#23949 = CARTESIAN_POINT ( 'NONE',  ( -5.873418876839999747, -101.3150700380000018, 15.15334698740000086 ) ) ;
#23950 = ORIENTED_EDGE ( 'NONE', *, *, #7161, .F. ) ;
#23951 = EDGE_CURVE ( 'NONE', #23472, #23865, #170, .T. ) ;
#23952 = CARTESIAN_POINT ( 'NONE',  ( 27.07580689300000287, -92.50000460620000808, -12.39707951610000158 ) ) ;
#23953 = ADVANCED_FACE ( 'NONE', ( #7908 ), #811, .T. ) ;
#23954 = ORIENTED_EDGE ( 'NONE', *, *, #6592, .T. ) ;
#23955 = CARTESIAN_POINT ( 'NONE',  ( -0.7191277762650000183, -101.4254868729999970, -15.95275638909999749 ) ) ;
#23956 = CARTESIAN_POINT ( 'NONE',  ( -3.252988965690000178, -72.00000000000000000, -30.32986301179999700 ) ) ;
#23957 = DIRECTION ( 'NONE',  ( 0.000000000000000000, -1.000000000000000000, 0.000000000000000000 ) ) ;
#23958 = CARTESIAN_POINT ( 'NONE',  ( 12.83908560070000071, -94.89197151660000884, -19.89638108760000179 ) ) ;
#23959 = CARTESIAN_POINT ( 'NONE',  ( 15.99636488046209060, -94.79936261290481525, 17.25621003525883168 ) ) ;
#23960 = DIRECTION ( 'NONE',  ( -0.3388747807339287932, -0.000000000000000000, -0.9408314849018032389 ) ) ;
#23961 = CIRCLE ( 'NONE', #2117, 34.89999999999999858 ) ;
#23962 = CARTESIAN_POINT ( 'NONE',  ( 13.81100091409999919, -99.92967571559999840, -10.51865105429999936 ) ) ;
#23963 = DIRECTION ( 'NONE',  ( 0.000000000000000000, -1.000000000000000000, 0.000000000000000000 ) ) ;
#23964 = CARTESIAN_POINT ( 'NONE',  ( 7.351926511809999454, -36.21205854349999953, -21.46601197540000072 ) ) ;
#23965 = DIRECTION ( 'NONE',  ( 1.000000000000000000, 0.000000000000000000, 0.000000000000000000 ) ) ;
#23966 = ORIENTED_EDGE ( 'NONE', *, *, #20297, .T. ) ;
#23967 = CARTESIAN_POINT ( 'NONE',  ( 8.815784351519999618, -19.48264119070000078, -19.82501765289999796 ) ) ;
#23968 = CARTESIAN_POINT ( 'NONE',  ( -13.85848666890000125, -57.40875702409999803, 21.24403892489999990 ) ) ;
#23969 = CARTESIAN_POINT ( 'NONE',  ( -2.790536552329999864, -64.24504439390000243, -26.36014980279999875 ) ) ;
#23970 = CARTESIAN_POINT ( 'NONE',  ( 10.68317386900000088, -36.00000000000000000, -21.62249396890000241 ) ) ;
#23971 = CARTESIAN_POINT ( 'NONE',  ( -25.74949179000000044, -93.99830544879999650, -2.429629024850000096 ) ) ;
#23972 = CARTESIAN_POINT ( 'NONE',  ( -19.84037407199999947, -55.01779585689999408, 14.17763065249999954 ) ) ;
#23973 = EDGE_CURVE ( 'NONE', #11658, #14011, #25753, .T. ) ;
#23974 = VECTOR ( 'NONE', #13521, 1000.000000000000000 ) ;
#23975 = VERTEX_POINT ( 'NONE', #14461 ) ;
#23976 = CARTESIAN_POINT ( 'NONE',  ( -18.06114732863891348, -97.34036579259480959, -10.09119009767709407 ) ) ;
#23977 = CARTESIAN_POINT ( 'NONE',  ( 19.97576656849999921, -35.50000000000000000, -19.97576656849999921 ) ) ;
#23978 = ORIENTED_EDGE ( 'NONE', *, *, #22206, .T. ) ;
#23979 = EDGE_CURVE ( 'NONE', #6426, #5907, #11840, .T. ) ;
#23980 = DIRECTION ( 'NONE',  ( 1.000000000000000000, 0.000000000000000000, 0.000000000000000000 ) ) ;
#23981 = EDGE_CURVE ( 'NONE', #23613, #12242, #11767, .T. ) ;
#23982 = CARTESIAN_POINT ( 'NONE',  ( 5.329070518200000398E-15, -74.50000000000000000, 0.000000000000000000 ) ) ;
#23983 = CIRCLE ( 'NONE', #11413, 22.61111346610000084 ) ;
#23984 = CARTESIAN_POINT ( 'NONE',  ( -22.18442533826599217, -74.19997306779613666, -32.65038183209173184 ) ) ;
#23985 = CARTESIAN_POINT ( 'NONE',  ( 22.19631186670000034, -18.86932112550000085, 9.599616484340000255 ) ) ;
#23986 = CARTESIAN_POINT ( 'NONE',  ( -32.75544218747561587, -74.29667472474076817, -22.20975189080888867 ) ) ;
#23987 = CARTESIAN_POINT ( 'NONE',  ( 11.14159932559999966, -101.1364147039999892, -10.55279472049999967 ) ) ;
#23988 = VERTEX_POINT ( 'NONE', #25685 ) ;
#23989 = SPHERICAL_SURFACE ( 'NONE', #26462, 2.000000000000000000 ) ;
#23990 = CARTESIAN_POINT ( 'NONE',  ( -11.82347332360000003, -101.2358105800000061, -9.579693020240000578 ) ) ;
#23991 = DIRECTION ( 'NONE',  ( 0.000000000000000000, -1.000000000000000000, 0.000000000000000000 ) ) ;
#23992 = CARTESIAN_POINT ( 'NONE',  ( -7.312065474886813909, -101.4085864806282160, 14.43964435962598358 ) ) ;
#23993 = EDGE_LOOP ( 'NONE', ( #14867, #28192, #12226, #17384 ) ) ;
#23994 = B_SPLINE_CURVE_WITH_KNOTS ( 'NONE', 5,
 ( #2185, #13381, #24324, #13088, #26814, #6550 ),
 .UNSPECIFIED., .F., .F.,
 ( 6, 6 ),
 ( 0.000000000000000000, 1.000000000000000000 ),
 .UNSPECIFIED. ) ;
#23995 = CARTESIAN_POINT ( 'NONE',  ( -25.98617420859999783, -79.50000000000000000, -36.59277592640000165 ) ) ;
#23996 = CARTESIAN_POINT ( 'NONE',  ( 37.14872973290000147, -79.99999989399999833, -13.69566407600000169 ) ) ;
#23997 = ORIENTED_EDGE ( 'NONE', *, *, #17203, .F. ) ;
#23998 = EDGE_CURVE ( 'NONE', #5681, #26675, #14111, .T. ) ;
#23999 = FACE_OUTER_BOUND ( 'NONE', #4449, .T. ) ;
#24000 = CIRCLE ( 'NONE', #3103, 39.25000000000000000 ) ;
#24001 = FACE_OUTER_BOUND ( 'NONE', #7802, .T. ) ;
#24002 = ORIENTED_EDGE ( 'NONE', *, *, #1884, .F. ) ;
#24003 = EDGE_CURVE ( 'NONE', #24292, #22471, #14593, .T. ) ;
#24004 = VERTEX_POINT ( 'NONE', #27452 ) ;
#24005 = CARTESIAN_POINT ( 'NONE',  ( 21.60392450109999984, -56.24740423709999249, 10.18205705279999940 ) ) ;
#24006 = CARTESIAN_POINT ( 'NONE',  ( -15.36947826900000003, -101.0685828069999985, 4.769131590209999771 ) ) ;
#24007 = CARTESIAN_POINT ( 'NONE',  ( 10.52519477159999894, -92.53453854219999641, 27.02797911619999738 ) ) ;
#24008 = ORIENTED_EDGE ( 'NONE', *, *, #27228, .F. ) ;
#24009 = ADVANCED_FACE ( 'NONE', ( #9934 ), #14320, .F. ) ;
#24010 = CARTESIAN_POINT ( 'NONE',  ( -42.10639864760541684, -65.69467928435254578, 0.8217321237320240890 ) ) ;
#24011 = CARTESIAN_POINT ( 'NONE',  ( 3.459338121946999694E-15, -74.00000000000000000, -32.25000000000000000 ) ) ;
#24012 = ADVANCED_FACE ( 'NONE', ( #25271 ), #22442, .T. ) ;
#24013 = ORIENTED_EDGE ( 'NONE', *, *, #13655, .T. ) ;
#24014 = CARTESIAN_POINT ( 'NONE',  ( -21.70609662629999903, -80.13404657770000483, -32.70204620079999813 ) ) ;
#24015 = CARTESIAN_POINT ( 'NONE',  ( -16.50842902520000166, -93.39359504729999628, -21.60523500349999892 ) ) ;
#24016 = CARTESIAN_POINT ( 'NONE',  ( 26.13974465595868679, -69.66091081680940533, 10.83115750005767097 ) ) ;
#24017 = ORIENTED_EDGE ( 'NONE', *, *, #2629, .T. ) ;
#24018 = DIRECTION ( 'NONE',  ( 0.000000000000000000, 1.000000000000000000, 0.000000000000000000 ) ) ;
#24019 = CARTESIAN_POINT ( 'NONE',  ( 13.66933441149999950, -100.1459902240000019, -10.03108682719999933 ) ) ;
#24020 = CARTESIAN_POINT ( 'NONE',  ( -37.75000000000000000, -63.30468293320000583, -0.7216878364849999006 ) ) ;
#24021 = CARTESIAN_POINT ( 'NONE',  ( -2.578307999469999778, -52.56313962730000355, -25.11373953509999879 ) ) ;
#24022 = B_SPLINE_CURVE_WITH_KNOTS ( 'NONE', 5,
 ( #22665, #9390, #13766, #9676, #25145, #20179, #2709, #26892, #9539, #20319, #543, #389 ),
 .UNSPECIFIED., .F., .F.,
 ( 6, 3, 3, 6 ),
 ( -25.08217526889999860, -18.82033206645258616, -10.56888224947905819, -7.186327137053730496 ),
 .UNSPECIFIED. ) ;
#24023 = CARTESIAN_POINT ( 'NONE',  ( 11.37934278408159194, -72.27101671311534403, -27.01370042787952030 ) ) ;
#24024 = CARTESIAN_POINT ( 'NONE',  ( -19.73459501870000210, -19.50000008899999671, 14.41863475499999936 ) ) ;
#24025 = ORIENTED_EDGE ( 'NONE', *, *, #12765, .T. ) ;
#24026 = LINE ( 'NONE', #10735, #22528 ) ;
#24027 = DIRECTION ( 'NONE',  ( 0.000000000000000000, 1.000000000000000000, 0.000000000000000000 ) ) ;
#24028 = CARTESIAN_POINT ( 'NONE',  ( 0.000000000000000000, -17.50000000000000000, 0.000000000000000000 ) ) ;
#24029 = CARTESIAN_POINT ( 'NONE',  ( -0.6731250195771717459, -92.54938211485213628, -30.49269871153447298 ) ) ;
#24030 = DIRECTION ( 'NONE',  ( 1.000000000000000000, 0.000000000000000000, 0.000000000000000000 ) ) ;
#24031 = CARTESIAN_POINT ( 'NONE',  ( -11.69653606700000026, -94.52419709919999491, -20.97822790150000216 ) ) ;
#24032 = ORIENTED_EDGE ( 'NONE', *, *, #4475, .T. ) ;
#24033 = ADVANCED_FACE ( 'NONE', ( #25956 ), #12529, .T. ) ;
#24034 = CARTESIAN_POINT ( 'NONE',  ( 20.76627821419999975, -96.95622423369999865, -2.346863933399999880 ) ) ;
#24035 = ORIENTED_EDGE ( 'NONE', *, *, #16821, .T. ) ;
#24036 = CARTESIAN_POINT ( 'NONE',  ( 21.55284568440000115, -37.11646645979999448, -8.225667895000000840 ) ) ;
#24037 = CARTESIAN_POINT ( 'NONE',  ( 9.056984553609998656, -35.76308213440000117, -19.54972227260000039 ) ) ;
#24038 = ORIENTED_EDGE ( 'NONE', *, *, #17123, .T. ) ;
#24039 = EDGE_CURVE ( 'NONE', #22913, #23692, #20952, .T. ) ;
#24040 = CARTESIAN_POINT ( 'NONE',  ( -12.96744186819999989, -101.1042759770000004, -9.004950000140000910 ) ) ;
#24041 = CARTESIAN_POINT ( 'NONE',  ( 3.355978770230000130, -91.50000000000000000, 6.143077933229999843 ) ) ;
#24042 = CARTESIAN_POINT ( 'NONE',  ( -3.281858763419757352, -67.67702679679626954, -27.44020346820908074 ) ) ;
#24043 = CARTESIAN_POINT ( 'NONE',  ( -8.190587505059999884, -99.74726900420000675, 15.07401393059999961 ) ) ;
#24044 = DIRECTION ( 'NONE',  ( 0.4794255386042040601, 0.000000000000000000, 0.8775825618903720926 ) ) ;
#24045 = DIRECTION ( 'NONE',  ( 0.4794255386042041711, 0.000000000000000000, 0.8775825618903720926 ) ) ;
#24046 = CARTESIAN_POINT ( 'NONE',  ( 7.914382952159999540, -49.10861551380000378, -21.88571563610000226 ) ) ;
#24047 = CARTESIAN_POINT ( 'NONE',  ( -11.17631027600000060, -19.46429362099999949, -18.99082252140000193 ) ) ;
#24048 = ORIENTED_EDGE ( 'NONE', *, *, #8300, .F. ) ;
#24049 = CARTESIAN_POINT ( 'NONE',  ( 13.65853266997999071, -100.3617719036068081, -10.14140713304427877 ) ) ;
#24050 = CARTESIAN_POINT ( 'NONE',  ( 24.63152983679999863, -42.21394486829999693, 1.405087790390000091 ) ) ;
#24051 = CARTESIAN_POINT ( 'NONE',  ( 24.74138143300000081, -65.80499425489999510, 10.85530572179999886 ) ) ;
#24052 = DIRECTION ( 'NONE',  ( -1.836909530729999990E-16, 0.000000000000000000, 1.000000000000000000 ) ) ;
#24053 = EDGE_LOOP ( 'NONE', ( #17578, #3955, #8583, #24569, #21124, #11282, #14596, #16831, #9177, #10790 ) ) ;
#24054 = CARTESIAN_POINT ( 'NONE',  ( -38.65569705749999940, -74.00000000000000000, 7.472970580910000216 ) ) ;
#24055 = CARTESIAN_POINT ( 'NONE',  ( -20.49364000779999984, -54.17834560379999687, 14.81079386229999884 ) ) ;
#24056 = CARTESIAN_POINT ( 'NONE',  ( -15.93508487770000137, -92.93255488879999859, 23.98294276400000058 ) ) ;
#24057 = CARTESIAN_POINT ( 'NONE',  ( -20.55830956777789709, -92.99223971643057496, 17.22324199352144092 ) ) ;
#24058 = VERTEX_POINT ( 'NONE', #8450 ) ;
#24059 =( GEOMETRIC_REPRESENTATION_CONTEXT ( 3 ) GLOBAL_UNCERTAINTY_ASSIGNED_CONTEXT ( ( #14413 ) ) GLOBAL_UNIT_ASSIGNED_CONTEXT ( ( #1808, #21623, #5882 ) ) REPRESENTATION_CONTEXT ( 'NONE', 'WORKASPACE' ) );
#24060 = CARTESIAN_POINT ( 'NONE',  ( 26.64667737100000267, -68.06111685179999427, 1.045328632849999995 ) ) ;
#24061 = EDGE_CURVE ( 'NONE', #28564, #27146, #20152, .T. ) ;
#24062 = CARTESIAN_POINT ( 'NONE',  ( 0.6375376905170000441, -100.5229262450000078, -16.86993779310000008 ) ) ;
#24063 = CARTESIAN_POINT ( 'NONE',  ( 7.555863278439999497, -62.13670074319999515, -22.76391182080000064 ) ) ;
#24064 = CARTESIAN_POINT ( 'NONE',  ( 15.53498458480000011, -101.1499348409999897, 2.599897626340000212 ) ) ;
#24065 = CARTESIAN_POINT ( 'NONE',  ( 26.60903970598167589, -23.00000000000000000, 48.70752046822583736 ) ) ;
#24066 = DIRECTION ( 'NONE',  ( 1.000000000000000000, 0.000000000000000000, 0.000000000000000000 ) ) ;
#24067 = ORIENTED_EDGE ( 'NONE', *, *, #6681, .F. ) ;
#24068 = CARTESIAN_POINT ( 'NONE',  ( 6.656205481639999810, -101.1976625110000043, 14.93341658319999965 ) ) ;
#24069 = CARTESIAN_POINT ( 'NONE',  ( 15.00803725019999924, -101.1284992150000051, 3.477295974860000083 ) ) ;
#24070 = TOROIDAL_SURFACE ( 'NONE', #18971, 7.750000000000000000, 0.5000000000000000000 ) ;
#24071 = ORIENTED_EDGE ( 'NONE', *, *, #8694, .F. ) ;
#24072 = EDGE_CURVE ( 'NONE', #258, #11126, #26206, .T. ) ;
#24073 = CARTESIAN_POINT ( 'NONE',  ( 8.366907574789999913, -35.47960661259999426, -21.01624086869999886 ) ) ;
#24074 = CARTESIAN_POINT ( 'NONE',  ( 23.75187361598589675, -62.52448827938915343, 10.63125306484759847 ) ) ;
#24075 = CARTESIAN_POINT ( 'NONE',  ( 2.842170943039999687E-14, -72.00000000000000000, 1.776356839399999804E-15 ) ) ;
#24076 = ORIENTED_EDGE ( 'NONE', *, *, #196, .F. ) ;
#24077 = CARTESIAN_POINT ( 'NONE',  ( 4.580264318640000276, -92.68289710869998999, -27.72400028910000458 ) ) ;
#24078 = CIRCLE ( 'NONE', #6899, 38.75000000000000000 ) ;
#24079 = CARTESIAN_POINT ( 'NONE',  ( 6.738397544221694346, -101.4241070619504796, 14.70285685720373792 ) ) ;
#24080 = FACE_OUTER_BOUND ( 'NONE', #4832, .T. ) ;
#24081 = ORIENTED_EDGE ( 'NONE', *, *, #17203, .T. ) ;
#24082 = EDGE_CURVE ( 'NONE', #13829, #19768, #7630, .T. ) ;
#24083 = CARTESIAN_POINT ( 'NONE',  ( -38.08875739639999836, -82.25000000000000000, -9.476764215410000247 ) ) ;
#24084 = DIRECTION ( 'NONE',  ( 1.000000000000000000, 0.000000000000000000, 0.000000000000000000 ) ) ;
#24085 = VERTEX_POINT ( 'NONE', #23628 ) ;
#24086 = CARTESIAN_POINT ( 'NONE',  ( 7.403496485329999821, -36.74765514679999967, -21.48174179600000144 ) ) ;
#24087 = CARTESIAN_POINT ( 'NONE',  ( 26.91890708249999875, -92.56168957700000988, -12.40459431399999879 ) ) ;
#24088 = CARTESIAN_POINT ( 'NONE',  ( -1.229530056899999835, -101.0685849509999912, -16.04536266459999894 ) ) ;
#24089 = DIRECTION ( 'NONE',  ( 0.8775825618903723147, 0.000000000000000000, 0.4794255386042037825 ) ) ;
#24090 = CARTESIAN_POINT ( 'NONE',  ( -38.24483487620000233, -65.84529946160000691, 0.9588510772079998912 ) ) ;
#24091 = CARTESIAN_POINT ( 'NONE',  ( 13.03263341399999931, -94.63960343439998724, -19.83860458410000049 ) ) ;
#24092 = TOROIDAL_SURFACE ( 'NONE', #19434, 6.750000000000000000, 0.5000000000000000000 ) ;
#24093 = ORIENTED_EDGE ( 'NONE', *, *, #1428, .T. ) ;
#24094 = CARTESIAN_POINT ( 'NONE',  ( -14.83395525729999775, -101.1411475039999885, 4.096596759159999657 ) ) ;
#24095 = CARTESIAN_POINT ( 'NONE',  ( 0.000000000000000000, -2.000000000000000000, 0.000000000000000000 ) ) ;
#24096 = CARTESIAN_POINT ( 'NONE',  ( -36.70269827918048122, -65.09619745167545091, -0.03908829155573841085 ) ) ;
#24097 = PRODUCT_DEFINITION_SHAPE ( 'NONE', 'NONE',  #28808 ) ;
#24098 = ADVANCED_FACE ( 'NONE', ( #17498 ), #13584, .T. ) ;
#24099 = B_SPLINE_CURVE_WITH_KNOTS ( 'NONE', 3,
 ( #4375, #322, #26824, #20402 ),
 .UNSPECIFIED., .F., .F.,
 ( 4, 4 ),
 ( 0.000000000000000000, 1.000000000000000000 ),
 .UNSPECIFIED. ) ;
#24100 = CARTESIAN_POINT ( 'NONE',  ( 36.51232682552267050, -75.00000020506665521, -14.77966825339260382 ) ) ;
#24101 = CARTESIAN_POINT ( 'NONE',  ( -18.49652135632734584, -19.46608320370290102, 12.36970486431163074 ) ) ;
#24102 = DIRECTION ( 'NONE',  ( -0.4151946956541399669, 0.5000000000001689759, -0.7600087925152558821 ) ) ;
#24103 = CARTESIAN_POINT ( 'NONE',  ( 24.19803400451018760, -94.16483583547625358, -8.868831527973414453 ) ) ;
#24104 = CARTESIAN_POINT ( 'NONE',  ( 19.43643804750000115, -34.66800313659999944, -8.988996126470000902 ) ) ;
#24105 = EDGE_LOOP ( 'NONE', ( #6954, #15407, #12441, #12053 ) ) ;
#24106 = DIRECTION ( 'NONE',  ( -0.1516076670439319707, -0.9486832980505756074, -0.2775159730418759185 ) ) ;
#24107 = VECTOR ( 'NONE', #20633, 1000.000000000000000 ) ;
#24108 = AXIS2_PLACEMENT_3D ( 'NONE', #12502, #18823, #7880 ) ;
#24109 = CARTESIAN_POINT ( 'NONE',  ( 21.22142466270000227, -36.00000000000000000, -10.41046144799999951 ) ) ;
#24110 = EDGE_CURVE ( 'NONE', #23575, #26844, #16895, .T. ) ;
#24111 = CARTESIAN_POINT ( 'NONE',  ( -2.343981719409999886, -60.15167146970000545, -24.54744736600000010 ) ) ;
#24112 = ORIENTED_EDGE ( 'NONE', *, *, #20468, .T. ) ;
#24113 = CARTESIAN_POINT ( 'NONE',  ( 9.649489330299999779, -36.18102153040000246, -21.30683186290000108 ) ) ;
#24114 = CARTESIAN_POINT ( 'NONE',  ( -25.20910175530000075, -93.61368346379998684, -2.138151043640000193 ) ) ;
#24115 = CARTESIAN_POINT ( 'NONE',  ( -19.65423707410000276, -57.45864773929999814, 13.63538719409999977 ) ) ;
#24116 = FACE_OUTER_BOUND ( 'NONE', #22896, .T. ) ;
#24117 = ORIENTED_EDGE ( 'NONE', *, *, #21910, .T. ) ;
#24118 = CARTESIAN_POINT ( 'NONE',  ( 21.28939746550000223, -35.22612253230000334, -7.745600858799999600 ) ) ;
#24119 = CARTESIAN_POINT ( 'NONE',  ( 7.260235792919999653, -73.97913911329999337, -40.03809227349999844 ) ) ;
#24120 = ORIENTED_EDGE ( 'NONE', *, *, #14425, .F. ) ;
#24121 = CARTESIAN_POINT ( 'NONE',  ( 7.923880834827633279, -37.75688408617100578, -21.55540859128345232 ) ) ;
#24122 = AXIS2_PLACEMENT_3D ( 'NONE', #16556, #10253, #5619 ) ;
#24123 = AXIS2_PLACEMENT_3D ( 'NONE', #16578, #18779, #4928 ) ;
#24124 = AXIS2_PLACEMENT_3D ( 'NONE', #25913, #23585, #25264 ) ;
#24125 = CARTESIAN_POINT ( 'NONE',  ( -9.493551874750000508, -18.50000000000000000, -20.00161470729999991 ) ) ;
#24126 = CARTESIAN_POINT ( 'NONE',  ( -40.00000000000000000, -63.50000000000000000, 0.000000000000000000 ) ) ;
#24127 = DIRECTION ( 'NONE',  ( 0.000000000000000000, 1.000000000000000000, 0.000000000000000000 ) ) ;
#24128 = CARTESIAN_POINT ( 'NONE',  ( -32.61798281429999946, -80.00000000000000000, -22.71848787769999944 ) ) ;
#24129 = CARTESIAN_POINT ( 'NONE',  ( -13.41619584950000110, -101.2306315440000049, -9.103915625870000028 ) ) ;
#24130 = ORIENTED_EDGE ( 'NONE', *, *, #9937, .F. ) ;
#24131 = CARTESIAN_POINT ( 'NONE',  ( 30.45033996220000105, -72.00000000000000000, 1.805359716810000181 ) ) ;
#24132 = CARTESIAN_POINT ( 'NONE',  ( -12.12074076350000063, -101.1180794200000008, -9.692271323269999073 ) ) ;
#24133 = EDGE_CURVE ( 'NONE', #20283, #17502, #22968, .T. ) ;
#24134 = DIRECTION ( 'NONE',  ( 1.000000000000000000, 0.000000000000000000, 0.000000000000000000 ) ) ;
#24135 = CARTESIAN_POINT ( 'NONE',  ( -7.422674037662165603, -101.3038909012893924, 14.47466155340364757 ) ) ;
#24136 = ORIENTED_EDGE ( 'NONE', *, *, #24442, .T. ) ;
#24137 = ADVANCED_FACE ( 'NONE', ( #22161 ), #6865, .F. ) ;
#24138 = B_SPLINE_CURVE_WITH_KNOTS ( 'NONE', 5,
 ( #3929, #4364, #26510, #23893, #15413, #23748, #13236, #21846, #12793, #13087, #26364, #6393, #25938, #21701, #17187, #8288, #10738, #5962 ),
 .UNSPECIFIED., .F., .F.,
 ( 6, 3, 3, 3, 3, 6 ),
 ( 0.000000000000000000, 1.124498255640000055, 2.252774941560000244, 3.380756636310000118, 4.508382774220000222, 5.576981603820000188 ),
 .UNSPECIFIED. ) ;
#24139 = VECTOR ( 'NONE', #28203, 1000.000000000000000 ) ;
#24140 = FACE_OUTER_BOUND ( 'NONE', #3199, .T. ) ;
#24141 = CARTESIAN_POINT ( 'NONE',  ( -32.08195032130000612, -74.00665451570000641, -21.91676683800000092 ) ) ;
#24142 = CARTESIAN_POINT ( 'NONE',  ( 36.88485589580000124, -80.18584060519999923, -13.59838148100000055 ) ) ;
#24143 = ORIENTED_EDGE ( 'NONE', *, *, #22380, .T. ) ;
#24144 = EDGE_CURVE ( 'NONE', #15756, #7849, #13642, .T. ) ;
#24145 = EDGE_CURVE ( 'NONE', #18220, #4271, #17362, .T. ) ;
#24146 = VECTOR ( 'NONE', #17990, 1000.000000000000000 ) ;
#24147 = CONICAL_SURFACE ( 'NONE', #11575, 1.732050807582486307, 1.047197551199999799 ) ;
#24148 = AXIS2_PLACEMENT_3D ( 'NONE', #1396, #16830, #25719 ) ;
#24149 = CARTESIAN_POINT ( 'NONE',  ( 27.89292634430000106, -72.00000000000000000, 12.34776042340000046 ) ) ;
#24150 = CARTESIAN_POINT ( 'NONE',  ( -18.26810397560000254, -94.98812477769999418, 16.32728546869999775 ) ) ;
#24151 = ORIENTED_EDGE ( 'NONE', *, *, #26367, .T. ) ;
#24152 = CARTESIAN_POINT ( 'NONE',  ( -20.25756709850169557, -95.19002702548807804, 10.95028088663572774 ) ) ;
#24153 = EDGE_LOOP ( 'NONE', ( #10418, #26625, #18236 ) ) ;
#24154 = CARTESIAN_POINT ( 'NONE',  ( 22.14531096509999841, -93.99830645880000191, 13.36130718660000127 ) ) ;
#24155 = DIRECTION ( 'NONE',  ( 1.000000000000000000, 0.000000000000000000, 1.225073682349999956E-16 ) ) ;
#24156 = ORIENTED_EDGE ( 'NONE', *, *, #8275, .F. ) ;
#24157 = PLANE ( 'NONE',  #28498 ) ;
#24158 = CARTESIAN_POINT ( 'NONE',  ( 20.49657866619999780, -57.47855601759999900, 11.20866246179999948 ) ) ;
#24159 = AXIS2_PLACEMENT_3D ( 'NONE', #25836, #23922, #10625 ) ;
#24160 = CARTESIAN_POINT ( 'NONE',  ( 9.726843560609999884, -36.00000000000000000, -20.21912206349999863 ) ) ;
#24161 = CARTESIAN_POINT ( 'NONE',  ( -20.49992799259999998, -92.87863185410000710, -20.70054720279999927 ) ) ;
#24162 = CARTESIAN_POINT ( 'NONE',  ( -3.190509958379999844, -18.50000000000000000, -22.41471204839999842 ) ) ;
#24163 = ORIENTED_EDGE ( 'NONE', *, *, #18134, .T. ) ;
#24164 = CIRCLE ( 'NONE', #19514, 57.75000000000000000 ) ;
#24165 = AXIS2_PLACEMENT_3D ( 'NONE', #14704, #10725, #28384 ) ;
#24166 = DIRECTION ( 'NONE',  ( 0.000000000000000000, 1.000000000000000000, 0.000000000000000000 ) ) ;
#24167 = CARTESIAN_POINT ( 'NONE',  ( 13.52017591309999922, -100.2511768809999921, -9.777168233029998490 ) ) ;
#24168 = DIRECTION ( 'NONE',  ( 1.000000000000000000, 0.000000000000000000, 0.000000000000000000 ) ) ;
#24169 = CARTESIAN_POINT ( 'NONE',  ( -11.69298166125931004, -94.57749869814954025, -21.18608910009514901 ) ) ;
#24170 = DIRECTION ( 'NONE',  ( 0.000000000000000000, 1.000000000000000000, 0.000000000000000000 ) ) ;
#24171 = CARTESIAN_POINT ( 'NONE',  ( 29.95046995577899196, -92.50630337894793342, 5.765085911501825144 ) ) ;
#24172 = DIRECTION ( 'NONE',  ( 0.000000000000000000, 0.000000000000000000, -1.000000000000000000 ) ) ;
#24173 = ORIENTED_EDGE ( 'NONE', *, *, #11591, .T. ) ;
#24174 = EDGE_CURVE ( 'NONE', #3921, #19835, #12249, .T. ) ;
#24175 = DIRECTION ( 'NONE',  ( 0.9601004944592521628, 0.000000000000000000, -0.2796552172570708761 ) ) ;
#24176 = CARTESIAN_POINT ( 'NONE',  ( -38.08919256720000135, -63.35440207070000440, 1.043878858160000034 ) ) ;
#24177 = CARTESIAN_POINT ( 'NONE',  ( 22.35420107259999867, -19.50000000000000000, 9.881343484100000296 ) ) ;
#24178 = DIRECTION ( 'NONE',  ( 0.000000000000000000, 1.000000000000000000, 0.000000000000000000 ) ) ;
#24179 = CARTESIAN_POINT ( 'NONE',  ( -0.1055951870944554088, -92.72722989461847476, -30.49981915221950146 ) ) ;
#24180 = EDGE_CURVE ( 'NONE', #4878, #11981, #24642, .T. ) ;
#24181 = CARTESIAN_POINT ( 'NONE',  ( 0.000000000000000000, 0.000000000000000000, 0.000000000000000000 ) ) ;
#24182 = DIRECTION ( 'NONE',  ( 6.123031769109993025E-17, 0.000000000000000000, -1.000000000000000000 ) ) ;
#24183 = TOROIDAL_SURFACE ( 'NONE', #4659, 55.85192378860000417, 0.3499999999999999778 ) ;
#24184 = TOROIDAL_SURFACE ( 'NONE', #19515, 53.85000000000000142, 0.5000000000000000000 ) ;
#24185 = VERTEX_POINT ( 'NONE', #30 ) ;
#24186 = DIRECTION ( 'NONE',  ( 0.000000000000000000, 1.000000000000000000, 0.000000000000000000 ) ) ;
#24187 = CARTESIAN_POINT ( 'NONE',  ( 22.49719386810000188, -95.90105812930001150, -4.302050608990000136 ) ) ;
#24188 = EDGE_LOOP ( 'NONE', ( #6789, #8096, #1540, #5051 ) ) ;
#24189 = CARTESIAN_POINT ( 'NONE',  ( 21.56715281920000038, -37.71255813250000699, -7.938702241180000563 ) ) ;
#24190 = CARTESIAN_POINT ( 'NONE',  ( -42.40756524499999358, -65.56519245710001087, -0.6307174998540000521 ) ) ;
#24191 = EDGE_LOOP ( 'NONE', ( #23179, #10463, #5967, #14412, #25760, #7158, #1807 ) ) ;
#24192 = CARTESIAN_POINT ( 'NONE',  ( 16.49889766720000139, -94.79581468469999095, 16.97757898100000062 ) ) ;
#24193 = B_SPLINE_CURVE_WITH_KNOTS ( 'NONE', 5,
 ( #1205, #27421, #10039, #5685, #784, #7881, #20570, #7312, #18954, #926, #18824, #27837 ),
 .UNSPECIFIED., .F., .F.,
 ( 6, 3, 3, 6 ),
 ( 0.000000000000000000, 0.4964111757593314134, 0.7833083924331026848, 1.000000000000000000 ),
 .UNSPECIFIED. ) ;
#24194 = CARTESIAN_POINT ( 'NONE',  ( -16.09760936190000180, -92.53016485179999506, -24.04852265159999902 ) ) ;
#24195 = DIRECTION ( 'NONE',  ( 0.000000000000000000, 1.000000000000000000, 0.000000000000000000 ) ) ;
#24196 = ORIENTED_EDGE ( 'NONE', *, *, #5972, .T. ) ;
#24197 = CARTESIAN_POINT ( 'NONE',  ( -6.571450035919999877, -97.39505561490000218, -20.10197936720000200 ) ) ;
#24198 = CARTESIAN_POINT ( 'NONE',  ( -29.03051485019999944, -92.50425969839999141, 5.507518881380000231 ) ) ;
#24199 = CARTESIAN_POINT ( 'NONE',  ( 8.600016955360000992, -57.45905992459999823, -22.33353630010000046 ) ) ;
#24200 = CARTESIAN_POINT ( 'NONE',  ( -29.53621923517769332, -92.52640451558471568, 7.606711608869601626 ) ) ;
#24201 = CARTESIAN_POINT ( 'NONE',  ( 11.97834023485886235, -100.7167551706393738, -12.12413065688971692 ) ) ;
#24202 = EDGE_LOOP ( 'NONE', ( #20820, #23356, #22820, #20956 ) ) ;
#24203 = DIRECTION ( 'NONE',  ( 0.4794255386042040046, 0.000000000000000000, 0.8775825618903722036 ) ) ;
#24204 = CARTESIAN_POINT ( 'NONE',  ( 25.02058468999999974, -57.41946978100000365, 1.375913977570000002 ) ) ;
#24205 = DIRECTION ( 'NONE',  ( 0.000000000000000000, 1.000000000000000000, 0.000000000000000000 ) ) ;
#24206 = CARTESIAN_POINT ( 'NONE',  ( 39.22862632788639559, -73.58711170886084574, 7.208933142618684897 ) ) ;
#24207 = ORIENTED_EDGE ( 'NONE', *, *, #18163, .F. ) ;
#24208 = LINE ( 'NONE', #2211, #26228 ) ;
#24209 = CARTESIAN_POINT ( 'NONE',  ( -13.35883408399999972, -92.54627707209999699, 27.01063094439999901 ) ) ;
#24210 = CARTESIAN_POINT ( 'NONE',  ( 27.07127034026193968, -92.49999918154685474, -10.05443361004321723 ) ) ;
#24211 = ORIENTED_EDGE ( 'NONE', *, *, #1381, .F. ) ;
#24212 = AXIS2_PLACEMENT_3D ( 'NONE', #2193, #24631, #15578 ) ;
#24213 = EDGE_CURVE ( 'NONE', #1763, #10539, #9784, .T. ) ;
#24214 = CARTESIAN_POINT ( 'NONE',  ( -40.00000000000000000, -73.50000000000000000, 3.397282455350000038E-15 ) ) ;
#24215 = AXIS2_PLACEMENT_3D ( 'NONE', #3685, #19548, #21887 ) ;
#24216 = CARTESIAN_POINT ( 'NONE',  ( 0.5403162009290000123, -100.8772072149999985, -15.79149104430000250 ) ) ;
#24217 = DIRECTION ( 'NONE',  ( 1.000000000000000000, 0.000000000000000000, 0.000000000000000000 ) ) ;
#24218 = CARTESIAN_POINT ( 'NONE',  ( 15.48147096319999960, -101.1716782170000073, 2.806783133030000155 ) ) ;
#24219 = CARTESIAN_POINT ( 'NONE',  ( 23.50166587800000073, -64.58097839929999395, 10.73601817129999958 ) ) ;
#24220 = CARTESIAN_POINT ( 'NONE',  ( 22.74072897519999970, -62.08051493450000180, -8.166369310169999451 ) ) ;
#24221 = ORIENTED_EDGE ( 'NONE', *, *, #27357, .T. ) ;
#24222 = DIRECTION ( 'NONE',  ( 1.000000000000000000, 0.000000000000000000, 0.000000000000000000 ) ) ;
#24223 = ORIENTED_EDGE ( 'NONE', *, *, #14726, .F. ) ;
#24224 = CARTESIAN_POINT ( 'NONE',  ( -17.53169073309999959, -94.47975186520000079, 16.30735973009999995 ) ) ;
#24225 = CARTESIAN_POINT ( 'NONE',  ( 23.57414836690000115, -18.50000000000000000, 2.476549100839999795 ) ) ;
#24226 = DIRECTION ( 'NONE',  ( 1.000000000000000000, 0.000000000000000000, 0.000000000000000000 ) ) ;
#24227 = ORIENTED_EDGE ( 'NONE', *, *, #21916, .T. ) ;
#24228 = CIRCLE ( 'NONE', #13035, 10.49999999999999822 ) ;
#24229 = CARTESIAN_POINT ( 'NONE',  ( -17.00715350810000004, -99.92967601899998442, 3.484608414699999823 ) ) ;
#24230 = CIRCLE ( 'NONE', #1453, 4.750000000000000888 ) ;
#24231 = VECTOR ( 'NONE', #21274, 1000.000000000000000 ) ;
#24232 = EDGE_CURVE ( 'NONE', #7043, #19169, #21599, .T. ) ;
#24233 = CARTESIAN_POINT ( 'NONE',  ( 0.000000000000000000, -17.50000000000000000, 0.000000000000000000 ) ) ;
#24234 = CARTESIAN_POINT ( 'NONE',  ( -6.572142520109999886, -101.1292389600000092, 14.04468523589999940 ) ) ;
#24235 = ORIENTED_EDGE ( 'NONE', *, *, #18904, .F. ) ;
#24236 = CARTESIAN_POINT ( 'NONE',  ( -13.11204875850966012, -100.1406256088236830, -11.11584611941340839 ) ) ;
#24237 = ORIENTED_EDGE ( 'NONE', *, *, #3971, .F. ) ;
#24238 = CARTESIAN_POINT ( 'NONE',  ( 8.862965437350000641, -35.80913068480000305, -20.41714882420000166 ) ) ;
#24239 = CARTESIAN_POINT ( 'NONE',  ( 25.53753465840000203, -93.24058218609999926, -5.819240763660000759 ) ) ;
#24240 = CARTESIAN_POINT ( 'NONE',  ( -1.044714352840000027, -101.1042759770000004, -15.75284879089999812 ) ) ;
#24241 = CARTESIAN_POINT ( 'NONE',  ( -23.77081188420000046, -93.00000000000000000, -19.11016751280000037 ) ) ;
#24242 = CARTESIAN_POINT ( 'NONE',  ( -43.20000000000000284, -63.07912966450000880, 0.1732050807559999961 ) ) ;
#24243 = CARTESIAN_POINT ( 'NONE',  ( -21.10288026827540264, -92.92035259892315935, -22.02258658995163287 ) ) ;
#24244 = ORIENTED_EDGE ( 'NONE', *, *, #1331, .F. ) ;
#24245 = CARTESIAN_POINT ( 'NONE',  ( -15.30640947800000085, -101.3256025499999993, 4.329700326000000210 ) ) ;
#24246 = CARTESIAN_POINT ( 'NONE',  ( -13.65271896930000040, -18.62222160940000037, 19.81146398099999928 ) ) ;
#24247 = DIRECTION ( 'NONE',  ( 0.000000000000000000, 1.000000000000000000, 0.000000000000000000 ) ) ;
#24248 = ADVANCED_FACE ( 'NONE', ( #18522 ), #7150, .F. ) ;
#24249 = CARTESIAN_POINT ( 'NONE',  ( -38.55000000000000426, -63.07912966450000880, -2.857883832489999776 ) ) ;
#24250 = CARTESIAN_POINT ( 'NONE',  ( -15.46523628789999982, -74.50000000000000000, 38.98408025979999536 ) ) ;
#24251 = CARTESIAN_POINT ( 'NONE',  ( 25.66698395754550077, -60.96609256304353153, 1.396244422503700955 ) ) ;
#24252 = CARTESIAN_POINT ( 'NONE',  ( 7.456866166569999343, -35.46743057900000196, -21.37275087869999624 ) ) ;
#24253 = CARTESIAN_POINT ( 'NONE',  ( 27.00388527187511656, -93.12686943497722325, 10.05985568221045767 ) ) ;
#24254 = AXIS2_PLACEMENT_3D ( 'NONE', #13118, #12822, #10917 ) ;
#24255 = VERTEX_POINT ( 'NONE', #9902 ) ;
#24256 = AXIS2_PLACEMENT_3D ( 'NONE', #2571, #26896, #6933 ) ;
#24257 = FACE_OUTER_BOUND ( 'NONE', #10197, .T. ) ;
#24258 = AXIS2_PLACEMENT_3D ( 'NONE', #20864, #1203, #27836 ) ;
#24259 = CARTESIAN_POINT ( 'NONE',  ( 21.60058908400000277, -36.18196428190000091, -9.926413990670001297 ) ) ;
#24260 = CARTESIAN_POINT ( 'NONE',  ( -11.47801891529999985, -59.03823354080000740, 20.41172223289999721 ) ) ;
#24261 = CARTESIAN_POINT ( 'NONE',  ( -24.12299397890000208, -94.89419905519999077, -4.133205798090000549 ) ) ;
#24262 = CARTESIAN_POINT ( 'NONE',  ( -19.68646692119999742, -57.47571038090000428, 12.70082239459999940 ) ) ;
#24263 = ADVANCED_FACE ( 'NONE', ( #25378 ), #11791, .T. ) ;
#24264 = ORIENTED_EDGE ( 'NONE', *, *, #24373, .T. ) ;
#24265 = CARTESIAN_POINT ( 'NONE',  ( -17.97303742817231509, -97.38870237790561646, -10.12129934261613151 ) ) ;
#24266 = DIRECTION ( 'NONE',  ( 0.5000000000001882938, 0.000000000000000000, -0.8660254037843299058 ) ) ;
#24267 = EDGE_LOOP ( 'NONE', ( #10408, #28643, #28403, #5065 ) ) ;
#24268 = AXIS2_PLACEMENT_3D ( 'NONE', #3106, #11958, #10179 ) ;
#24269 = DIRECTION ( 'NONE',  ( 0.000000000000000000, -1.000000000000000000, 0.000000000000000000 ) ) ;
#24270 = AXIS2_PLACEMENT_3D ( 'NONE', #16772, #5694, #1752 ) ;
#24271 = CARTESIAN_POINT ( 'NONE',  ( 0.7331063123750001242, -99.53431386179998697, -17.39857302659999760 ) ) ;
#24272 = CARTESIAN_POINT ( 'NONE',  ( 7.010390260919999428E-15, -69.00000000000000000, 36.25000000000000000 ) ) ;
#24273 = CARTESIAN_POINT ( 'NONE',  ( -39.50000000000000000, -65.63577453799999262, 2.309401076760000393 ) ) ;
#24274 = CARTESIAN_POINT ( 'NONE',  ( -13.82310862920000005, -74.00000000000000000, 36.20061004779999791 ) ) ;
#24275 = CARTESIAN_POINT ( 'NONE',  ( -32.81624540183023697, -79.75525706503896117, -22.27658736101337666 ) ) ;
#24276 = CYLINDRICAL_SURFACE ( 'NONE', #26930, 0.5000000000000004441 ) ;
#24277 = B_SPLINE_SURFACE_WITH_KNOTS ( 'NONE', 4, 5, ( 
 ( #24021, #14566, #25798, #12921, #21837, #1891, #8280, #5954, #12505 ),
 ( #1333, #10176, #23599, #14973, #10728, #19094, #27838, #12786, #23885 ),
 ( #8017, #14837, #16907, #25656, #5686, #21557, #21416, #1474, #10315 ),
 ( #17180, #2034, #11014, #17763, #8850, #20088, #13077, #24315, #26503 ),
 ( #21986, #4645, #26649, #24607, #11330, #6837, #6693, #15701, #10875 ) ),
 .UNSPECIFIED., .F., .F., .F.,
 ( 5, 5 ),
 ( 6, 3, 6 ),
 ( 4.938368304360000033E-16, 6.855861996819999860 ),
 ( 0.000000000000000000, 1.000000000000000000, 2.000000000000000000 ),
 .UNSPECIFIED. ) ;
#24278 = ORIENTED_EDGE ( 'NONE', *, *, #16719, .F. ) ;
#24279 = DIRECTION ( 'NONE',  ( 0.000000000000000000, 1.000000000000000000, 0.000000000000000000 ) ) ;
#24280 = DIRECTION ( 'NONE',  ( 0.4794255386042033384, 0.000000000000000000, 0.8775825618903726477 ) ) ;
#24281 = CARTESIAN_POINT ( 'NONE',  ( -12.32330071950000061, -101.1617736559999940, -9.795274802109998902 ) ) ;
#24282 = FILL_AREA_STYLE_COLOUR ( '', #7192 ) ;
#24283 = CARTESIAN_POINT ( 'NONE',  ( -37.48121085046030743, -63.24880261862786313, 0.5665023486436212563 ) ) ;
#24284 = ORIENTED_EDGE ( 'NONE', *, *, #26651, .T. ) ;
#24285 = CIRCLE ( 'NONE', #18250, 6.000000000000000000 ) ;
#24286 = CARTESIAN_POINT ( 'NONE',  ( 0.000000000000000000, -26.29689110869999880, 0.000000000000000000 ) ) ;
#24287 = CARTESIAN_POINT ( 'NONE',  ( -22.51794828416004890, -79.95513383975661270, -32.71047865149532896 ) ) ;
#24288 = ORIENTED_EDGE ( 'NONE', *, *, #6843, .T. ) ;
#24289 = CIRCLE ( 'NONE', #5700, 4.750000000000000000 ) ;
#24290 = CYLINDRICAL_SURFACE ( 'NONE', #18602, 18.64285714289999163 ) ;
#24291 = CARTESIAN_POINT ( 'NONE',  ( -18.19849796459701707, -94.71480814228209510, 16.19177224503937751 ) ) ;
#24292 = VERTEX_POINT ( 'NONE', #16753 ) ;
#24293 = EDGE_CURVE ( 'NONE', #26855, #18774, #5254, .T. ) ;
#24294 = CARTESIAN_POINT ( 'NONE',  ( -20.39102396179032084, -94.78512952904711142, 11.78310433714105976 ) ) ;
#24295 = ORIENTED_EDGE ( 'NONE', *, *, #734, .F. ) ;
#24296 = FACE_OUTER_BOUND ( 'NONE', #12773, .T. ) ;
#24297 = CARTESIAN_POINT ( 'NONE',  ( 46.45339896309999261, -74.00000000000000000, -4.166463576890000020 ) ) ;
#24298 = ORIENTED_EDGE ( 'NONE', *, *, #607, .T. ) ;
#24299 = CARTESIAN_POINT ( 'NONE',  ( 11.74592569580000045, -11.00000000000000000, 21.50077276629999901 ) ) ;
#24300 = CARTESIAN_POINT ( 'NONE',  ( -22.21938216790000098, -80.01919940119999808, -32.54924996240000468 ) ) ;
#24301 = EDGE_CURVE ( 'NONE', #11029, #18513, #5762, .T. ) ;
#24302 = B_SPLINE_CURVE_WITH_KNOTS ( 'NONE', 3,
 ( #14528, #6056, #10280, #23840, #3471, #23986, #7979, #19188, #15077, #17436, #12882, #14671, #1576, #17287, #12336, #10416, #14936, #12608, #4020, #21798, #10138, #23565, #1854, #10695, #21244, #8245, #3883, #28209, #16869, #1295, #21660 ),
 .UNSPECIFIED., .F., .F.,
 ( 4, 2, 2, 1, 1, 2, 2, 2, 1, 1, 2, 2, 2, 1, 1, 1, 2, 2, 4 ),
 ( 0.000000000000000000, 0.1250000000000730527, 0.1875000000001095790, 0.2187500000001328382, 0.2343750000001279810, 0.2421875000001261768, 0.2500000000001244005, 0.3750000000000689448, 0.4375000000000421330, 0.4687500000000286993, 0.4843750000000281442, 0.5000000000000276446, 0.6249999999998725464, 0.6874999999997949418, 0.7187499999997526423, 0.7343749999997410960, 0.7421874999997390976, 0.7499999999997370992, 1.000000000000000000 ),
 .UNSPECIFIED. ) ;
#24303 = VECTOR ( 'NONE', #4307, 1000.000000000000000 ) ;
#24304 = CIRCLE ( 'NONE', #2001, 16.00000000000000000 ) ;
#24305 = CARTESIAN_POINT ( 'NONE',  ( 8.479934984299998035, -37.33301741529999873, -21.77931235099999796 ) ) ;
#24306 = EDGE_CURVE ( 'NONE', #26673, #9115, #19705, .T. ) ;
#24307 = CARTESIAN_POINT ( 'NONE',  ( -23.28637498790000038, -92.50000947299999154, -18.90060859649999969 ) ) ;
#24308 = AXIS2_PLACEMENT_3D ( 'NONE', #17712, #21936, #28624 ) ;
#24309 = DIRECTION ( 'NONE',  ( 0.000000000000000000, -1.000000000000000000, 0.000000000000000000 ) ) ;
#24310 = VERTEX_POINT ( 'NONE', #14558 ) ;
#24311 = EDGE_CURVE ( 'NONE', #21723, #7597, #16393, .T. ) ;
#24312 = CARTESIAN_POINT ( 'NONE',  ( 36.36428601960000151, -73.99923028089999377, -13.97901162650000018 ) ) ;
#24313 = CARTESIAN_POINT ( 'NONE',  ( 12.81378706179999938, -101.0640712160000021, -9.747090585469999624 ) ) ;
#24314 = DIRECTION ( 'NONE',  ( 0.4794255386042040601, 0.000000000000000000, 0.8775825618903720926 ) ) ;
#24315 = CARTESIAN_POINT ( 'NONE',  ( -0.8467854781579999823, -56.26681992150000156, -23.30550165100000015 ) ) ;
#24316 = DIRECTION ( 'NONE',  ( 1.000000000000000000, 0.000000000000000000, 0.000000000000000000 ) ) ;
#24317 = CARTESIAN_POINT ( 'NONE',  ( 11.16657025251494417, -72.37633449930413576, -26.91772825060574803 ) ) ;
#24318 = CARTESIAN_POINT ( 'NONE',  ( 12.39757656149999931, -101.6484611540000031, -10.11435096289999969 ) ) ;
#24319 = VERTEX_POINT ( 'NONE', #16475 ) ;
#24320 = FACE_OUTER_BOUND ( 'NONE', #2940, .T. ) ;
#24321 = CARTESIAN_POINT ( 'NONE',  ( 20.31287103041500330, -73.22909343996219889, -31.37144790015285167 ) ) ;
#24322 = CARTESIAN_POINT ( 'NONE',  ( 7.615531154710000195, -93.65023553240000354, -24.05380218500000211 ) ) ;
#24323 = CARTESIAN_POINT ( 'NONE',  ( 7.619628858569999608, -36.43422328860000192, -21.46039065680000135 ) ) ;
#24324 = CARTESIAN_POINT ( 'NONE',  ( 21.33284145582814517, -96.53847999911016586, 1.142362698555328793 ) ) ;
#24325 = CARTESIAN_POINT ( 'NONE',  ( -25.37284092810000047, -93.00000000000000000, 2.543411731580000001 ) ) ;
#24326 = DIRECTION ( 'NONE',  ( 0.9183650514339934956, 0.000000000000000000, -0.3957342950827467121 ) ) ;
#24327 = B_SPLINE_CURVE_WITH_KNOTS ( 'NONE', 3,
 ( #13228, #26219, #6387, #4205, #8281, #22139, #19504, #28668, #10583, #23887, #10878, #19643, #21559, #10452, #26068, #28388, #1614, #6098, #19931, #28535, #8570, #24317, #13080, #2178, #21988, #2037, #17181, #24023, #17474, #26652, #5, #17327, #8852 ),
 .UNSPECIFIED., .F., .F.,
 ( 4, 2, 2, 1, 2, 2, 2, 2, 1, 2, 2, 2, 2, 1, 1, 1, 2, 2, 4 ),
 ( 0.000000000000000000, 0.1250000000000635048, 0.1875000000000947020, 0.2187500000001103007, 0.2343750000001184330, 0.2500000000001265654, 0.3750000000001944556, 0.4375000000002257083, 0.4687500000002383094, 0.4843750000002446376, 0.5000000000002509104, 0.6250000000003361755, 0.6875000000003781420, 0.7187500000003974598, 0.7343750000004078959, 0.7421875000004114487, 0.7460937500004124479, 0.7500000000004134471, 1.000000000000000000 ),
 .UNSPECIFIED. ) ;
#24328 = AXIS2_PLACEMENT_3D ( 'NONE', #26, #26674, #4824 ) ;
#24329 = VECTOR ( 'NONE', #16510, 1000.000000000000000 ) ;
#24330 = PLANE ( 'NONE',  #25146 ) ;
#24331 = ORIENTED_EDGE ( 'NONE', *, *, #5451, .F. ) ;
#24332 = CARTESIAN_POINT ( 'NONE',  ( 15.77847595849999784, -100.9405345029999950, 2.296807716130000010 ) ) ;
#24333 = ORIENTED_EDGE ( 'NONE', *, *, #18924, .T. ) ;
#24334 = CARTESIAN_POINT ( 'NONE',  ( -13.56438818361382914, -18.97801334097803760, 20.36277990756491718 ) ) ;
#24335 = CARTESIAN_POINT ( 'NONE',  ( 9.364228581315421351, -35.99000303267523293, -19.78658063234450992 ) ) ;
#24336 = VERTEX_POINT ( 'NONE', #5406 ) ;
#24337 = CARTESIAN_POINT ( 'NONE',  ( 8.855030637886567746, -36.23917065938484683, -21.13310776212970055 ) ) ;
#24338 = ADVANCED_FACE ( 'NONE', ( #12362 ), #15493, .T. ) ;
#24339 = PRODUCT_DEFINITION_SHAPE ( 'NONE', 'NONE',  #121 ) ;
#24340 = ORIENTED_EDGE ( 'NONE', *, *, #5013, .F. ) ;
#24341 = CARTESIAN_POINT ( 'NONE',  ( -4.663136541669999247, -98.35430138709999426, -18.48787719950000152 ) ) ;
#24342 = AXIS2_PLACEMENT_3D ( 'NONE', #7036, #11520, #27288 ) ;
#24343 = DIRECTION ( 'NONE',  ( 1.000000000000000000, 0.000000000000000000, 0.000000000000000000 ) ) ;
#24344 = DIRECTION ( 'NONE',  ( 0.000000000000000000, 1.000000000000000000, 0.000000000000000000 ) ) ;
#24345 = CARTESIAN_POINT ( 'NONE',  ( -10.95392404250000062, -19.15751145089999952, -19.17041938750000085 ) ) ;
#24346 = CARTESIAN_POINT ( 'NONE',  ( 11.60004717582089739, -98.07566646012705291, -16.86827489351441045 ) ) ;
#24347 = ORIENTED_EDGE ( 'NONE', *, *, #23007, .F. ) ;
#24348 = ADVANCED_FACE ( 'NONE', ( #14289 ), #12089, .F. ) ;
#24349 = CARTESIAN_POINT ( 'NONE',  ( 20.78260698670000295, -56.78056608349999834, 38.04230691420000454 ) ) ;
#24350 = CARTESIAN_POINT ( 'NONE',  ( -13.34153245340000105, -111.0000000000000000, 27.42724032409999779 ) ) ;
#24351 = CARTESIAN_POINT ( 'NONE',  ( 25.15895431540000260, -70.69114014129999646, 11.62372445859999814 ) ) ;
#24352 = CARTESIAN_POINT ( 'NONE',  ( -32.72159597179999935, -74.32000120609998817, -21.62349002899999917 ) ) ;
#24353 = ORIENTED_EDGE ( 'NONE', *, *, #10084, .F. ) ;
#24354 = AXIS2_PLACEMENT_3D ( 'NONE', #7465, #2943, #11806 ) ;
#24355 = LINE ( 'NONE', #22171, #18802 ) ;
#24356 = CARTESIAN_POINT ( 'NONE',  ( -17.75840719219999997, -93.65013249519999761, 19.45109209530000172 ) ) ;
#24357 = DIRECTION ( 'NONE',  ( 0.000000000000000000, -1.000000000000000000, 0.000000000000000000 ) ) ;
#24358 = VERTEX_POINT ( 'NONE', #777 ) ;
#24359 = CARTESIAN_POINT ( 'NONE',  ( 27.79603073779999889, -69.50480368919998853, 2.066568264030000268 ) ) ;
#24360 = CARTESIAN_POINT ( 'NONE',  ( 0.2077369398249999943, -101.1402801299999936, -15.33898559480000046 ) ) ;
#24361 = CARTESIAN_POINT ( 'NONE',  ( 24.20036131582700634, -74.16719602402496037, -30.74030054472169837 ) ) ;
#24362 = CARTESIAN_POINT ( 'NONE',  ( 15.74335372269999844, -101.6484611540000031, 2.854262349889999939 ) ) ;
#24363 = CARTESIAN_POINT ( 'NONE',  ( 24.55403954519999843, -64.36570418790000758, -9.970356804210000590 ) ) ;
#24364 = ORIENTED_EDGE ( 'NONE', *, *, #12887, .T. ) ;
#24365 = CARTESIAN_POINT ( 'NONE',  ( -18.34989813179999985, -101.1889999979999999, 23.56346505449999995 ) ) ;
#24366 = AXIS2_PLACEMENT_3D ( 'NONE', #25128, #22505, #11696 ) ;
#24367 = ORIENTED_EDGE ( 'NONE', *, *, #25496, .F. ) ;
#24368 = CARTESIAN_POINT ( 'NONE',  ( -39.65151520464630153, -65.69483747912252625, -2.234885500246811763 ) ) ;
#24369 = DIRECTION ( 'NONE',  ( 1.000000000000000000, 0.000000000000000000, 0.000000000000000000 ) ) ;
#24370 = CARTESIAN_POINT ( 'NONE',  ( 7.479537002301369419, -74.09468416706585003, 39.31219897218797144 ) ) ;
#24371 = ORIENTED_EDGE ( 'NONE', *, *, #22135, .F. ) ;
#24372 = CARTESIAN_POINT ( 'NONE',  ( 22.61295488650000252, -92.68419354099999907, 15.80596811629999721 ) ) ;
#24373 = EDGE_CURVE ( 'NONE', #9035, #6367, #13187, .T. ) ;
#24374 = DIRECTION ( 'NONE',  ( 0.000000000000000000, -1.000000000000000000, 0.000000000000000000 ) ) ;
#24375 = VERTEX_POINT ( 'NONE', #14150 ) ;
#24376 = DIRECTION ( 'NONE',  ( 1.000000000000000000, 0.000000000000000000, 0.000000000000000000 ) ) ;
#24377 = CARTESIAN_POINT ( 'NONE',  ( -12.57246511061115157, -100.9510322836001137, -10.75256427542645099 ) ) ;
#24378 = DIRECTION ( 'NONE',  ( -1.000000000000000000, 0.000000000000000000, 0.000000000000000000 ) ) ;
#24379 = DIRECTION ( 'NONE',  ( 0.000000000000000000, -1.000000000000000000, 0.000000000000000000 ) ) ;
#24380 = ORIENTED_EDGE ( 'NONE', *, *, #607, .F. ) ;
#24381 = EDGE_CURVE ( 'NONE', #28257, #7849, #25320, .T. ) ;
#24382 = CARTESIAN_POINT ( 'NONE',  ( 9.220169834260000030, -98.40144667389999711, 16.53004056780000042 ) ) ;
#24383 = AXIS2_PLACEMENT_3D ( 'NONE', #20910, #22659, #27174 ) ;
#24384 = DIRECTION ( 'NONE',  ( 0.7520801565632392327, -0.3326668106484357845, 0.5689536283360986380 ) ) ;
#24385 = CARTESIAN_POINT ( 'NONE',  ( -5.660850080320000366, -95.85308664740000495, -21.77572594749999979 ) ) ;
#24386 = AXIS2_PLACEMENT_3D ( 'NONE', #25007, #7689, #16554 ) ;
#24387 = CARTESIAN_POINT ( 'NONE',  ( -20.12052720778319426, -92.59033770634258076, -22.92234717996245408 ) ) ;
#24388 = ORIENTED_EDGE ( 'NONE', *, *, #2849, .F. ) ;
#24389 = CARTESIAN_POINT ( 'NONE',  ( 11.80818982729999966, -101.2459394079999981, -10.72877140129999951 ) ) ;
#24390 = CARTESIAN_POINT ( 'NONE',  ( 28.24050769817818107, -69.80859171892026893, 2.425102034864300649 ) ) ;
#24391 = CARTESIAN_POINT ( 'NONE',  ( -15.95377854864229050, -19.50000000000000000, 21.99697738415282799 ) ) ;
#24392 = CARTESIAN_POINT ( 'NONE',  ( -36.71069433210978872, -65.10053925468626801, -0.06637106436662004727 ) ) ;
#24393 = B_SPLINE_CURVE_WITH_KNOTS ( 'NONE', 5,
 ( #15879, #22011, #8873, #15724, #13250, #28686 ),
 .UNSPECIFIED., .F., .F.,
 ( 6, 6 ),
 ( 0.000000000000000000, 1.000000000000000000 ),
 .UNSPECIFIED. ) ;
#24394 = B_SPLINE_CURVE_WITH_KNOTS ( 'NONE', 5,
 ( #28076, #19332, #8242, #28492, #23837, #21240 ),
 .UNSPECIFIED., .F., .F.,
 ( 6, 6 ),
 ( 0.000000000000000000, 1.000000000000000000 ),
 .UNSPECIFIED. ) ;
#24395 = CARTESIAN_POINT ( 'NONE',  ( -41.91080743279999865, -63.35440207070000440, -1.043878858150000033 ) ) ;
#24396 = CARTESIAN_POINT ( 'NONE',  ( -12.07617952120000027, -66.61054971539999769, -23.44199634219999950 ) ) ;
#24397 = AXIS2_PLACEMENT_3D ( 'NONE', #18429, #22957, #13901 ) ;
#24398 = CARTESIAN_POINT ( 'NONE',  ( 24.68647381493572723, -93.48480241409957614, -11.77680583462976216 ) ) ;
#24399 = CARTESIAN_POINT ( 'NONE',  ( 22.55799654273938160, -93.99439547208534407, 13.13363697907470851 ) ) ;
#24400 = VERTEX_POINT ( 'NONE', #27971 ) ;
#24401 = CARTESIAN_POINT ( 'NONE',  ( 2.756696846970000170, -109.2500000000000000, 5.046099730869999966 ) ) ;
#24402 = AXIS2_PLACEMENT_3D ( 'NONE', #15644, #13463, #22369 ) ;
#24403 = CARTESIAN_POINT ( 'NONE',  ( -14.06310087329999803, -61.59908875819999707, 21.57936076700000072 ) ) ;
#24404 = EDGE_LOOP ( 'NONE', ( #11278, #15342, #17021, #18885, #27999, #17959, #16756 ) ) ;
#24405 = CARTESIAN_POINT ( 'NONE',  ( -13.51150976399999948, -58.88293941810000121, 20.78295126999999809 ) ) ;
#24406 = DIRECTION ( 'NONE',  ( 0.3687499999999814260, 0.000000000000000000, -0.9295286103719527793 ) ) ;
#24407 = AXIS2_PLACEMENT_3D ( 'NONE', #25824, #21440, #1768 ) ;
#24408 = DIRECTION ( 'NONE',  ( 1.000000000000000000, 0.000000000000000000, 0.000000000000000000 ) ) ;
#24409 = CARTESIAN_POINT ( 'NONE',  ( -19.96385611919999903, -52.58489974430000302, 14.40794232450000045 ) ) ;
#24410 = CARTESIAN_POINT ( 'NONE',  ( -14.99091303862281777, -98.53908159007769996, -11.25711904965173460 ) ) ;
#24411 = ADVANCED_FACE ( 'NONE', ( #19492 ), #12264, .T. ) ;
#24412 = EDGE_LOOP ( 'NONE', ( #19732, #26827, #20586, #3638 ) ) ;
#24413 = DIRECTION ( 'NONE',  ( 0.4794255386042000078, 0.000000000000000000, 0.8775825618903743131 ) ) ;
#24414 = CARTESIAN_POINT ( 'NONE',  ( -13.16239939709999796, -100.8816831189999874, -8.729909459909999114 ) ) ;
#24415 = ORIENTED_EDGE ( 'NONE', *, *, #12515, .F. ) ;
#24416 = EDGE_CURVE ( 'NONE', #7866, #10585, #25073, .T. ) ;
#24417 = CARTESIAN_POINT ( 'NONE',  ( 8.036636119666090039, -92.56492639278413037, 29.42229982729625704 ) ) ;
#24418 = DIRECTION ( 'NONE',  ( 0.4794255386042040601, 0.000000000000000000, 0.8775825618903720926 ) ) ;
#24419 = TOROIDAL_SURFACE ( 'NONE', #10901, 52.20000000000000284, 5.000000000000000000 ) ;
#24420 = CARTESIAN_POINT ( 'NONE',  ( 19.76472763569999813, -19.46501104069999855, 9.931837840570000964 ) ) ;
#24421 = FACE_OUTER_BOUND ( 'NONE', #1276, .T. ) ;
#24422 = CARTESIAN_POINT ( 'NONE',  ( 24.54513662149999931, -93.07154530310000951, -11.24897352390000016 ) ) ;
#24423 = CARTESIAN_POINT ( 'NONE',  ( 8.852567479250000204, -98.72068567929999006, 16.20451607640000091 ) ) ;
#24424 = CARTESIAN_POINT ( 'NONE',  ( 11.38850808709999995, -70.45799658879998617, -26.88027528670000166 ) ) ;
#24425 = CARTESIAN_POINT ( 'NONE',  ( 13.88364982429999905, -99.64579499010000063, -10.35699147140000065 ) ) ;
#24426 = VERTEX_POINT ( 'NONE', #17031 ) ;
#24427 = TOROIDAL_SURFACE ( 'NONE', #22102, 7.750000000000000000, 0.5000000000000000000 ) ;
#24428 = CARTESIAN_POINT ( 'NONE',  ( -38.55000000000000426, -63.07912966450000880, 2.857883832489999776 ) ) ;
#24429 = CARTESIAN_POINT ( 'NONE',  ( -9.597487326430000465, -80.50000000000000000, 38.57396449699999863 ) ) ;
#24430 = CARTESIAN_POINT ( 'NONE',  ( -12.90060417029999940, -99.77922884479998800, -11.29212820419999908 ) ) ;
#24431 = CARTESIAN_POINT ( 'NONE',  ( 21.63872345726285928, -19.48618186048361522, 9.527059235570996876 ) ) ;
#24432 = DIRECTION ( 'NONE',  ( 1.000000000000000000, 0.000000000000000000, 0.000000000000000000 ) ) ;
#24433 = EDGE_LOOP ( 'NONE', ( #7734, #13424, #3778, #20947 ) ) ;
#24434 = EDGE_CURVE ( 'NONE', #28363, #22004, #12544, .T. ) ;
#24435 = CARTESIAN_POINT ( 'NONE',  ( 0.000000000000000000, -108.5000000000000000, 6.000000000000000000 ) ) ;
#24436 = VERTEX_POINT ( 'NONE', #12914 ) ;
#24437 = DIRECTION ( 'NONE',  ( 0.000000000000000000, -1.000000000000000000, 0.000000000000000000 ) ) ;
#24438 = DIRECTION ( 'NONE',  ( 1.000000000000000000, 0.000000000000000000, 0.000000000000000000 ) ) ;
#24439 = CARTESIAN_POINT ( 'NONE',  ( 12.04737265749960784, -101.5555610555548469, -10.52904611307853777 ) ) ;
#24440 = ORIENTED_EDGE ( 'NONE', *, *, #5792, .F. ) ;
#24441 = ADVANCED_FACE ( 'NONE', ( #19220 ), #23451, .F. ) ;
#24442 = EDGE_CURVE ( 'NONE', #12207, #8283, #22649, .T. ) ;
#24443 = LINE ( 'NONE', #18032, #5194 ) ;
#24444 = CARTESIAN_POINT ( 'NONE',  ( -19.13290590728680129, -97.24060876560415068, 7.010995730810996029 ) ) ;
#24445 = VERTEX_POINT ( 'NONE', #25789 ) ;
#24446 = CARTESIAN_POINT ( 'NONE',  ( -24.46593625966632501, -94.79128788238732284, -3.807804778192843020 ) ) ;
#24447 = CARTESIAN_POINT ( 'NONE',  ( 22.17077749659999952, -94.09272483339999837, 13.34913124499999881 ) ) ;
#24448 = CARTESIAN_POINT ( 'NONE',  ( 46.63086251900000434, -74.05159139319999895, -3.730496185299999823 ) ) ;
#24449 = EDGE_LOOP ( 'NONE', ( #11827, #2315, #27162, #6434 ) ) ;
#24450 = CARTESIAN_POINT ( 'NONE',  ( -42.25000000000000000, -65.63577453799999262, 0.7216878364880000563 ) ) ;
#24451 = CARTESIAN_POINT ( 'NONE',  ( -22.29173994399999970, -79.81702446639999948, -32.80950025890000177 ) ) ;
#24452 = CARTESIAN_POINT ( 'NONE',  ( 9.561259125210000320, -36.00000000000000000, -20.11250876450000291 ) ) ;
#24453 = CARTESIAN_POINT ( 'NONE',  ( -42.10477055614926911, -63.33487562142746441, -0.8055360949872770737 ) ) ;
#24454 = CARTESIAN_POINT ( 'NONE',  ( -0.5590517731190000061, -18.50000000000000000, -21.02688049580000040 ) ) ;
#24455 = VERTEX_POINT ( 'NONE', #12634 ) ;
#24456 = CARTESIAN_POINT ( 'NONE',  ( -1.381305061119999955, -100.8816835080000089, -15.73378738089999729 ) ) ;
#24457 = CARTESIAN_POINT ( 'NONE',  ( -17.12548609519999943, -99.53431381699999747, 3.156820590889999778 ) ) ;
#24458 = CARTESIAN_POINT ( 'NONE',  ( -21.65925653600000444, -74.22385006870000268, -32.64405417670000276 ) ) ;
#24459 = DIRECTION ( 'NONE',  ( 0.000000000000000000, 1.000000000000000000, 0.000000000000000000 ) ) ;
#24460 = AXIS2_PLACEMENT_3D ( 'NONE', #26527, #6568, #25377 ) ;
#24461 = DIRECTION ( 'NONE',  ( 0.000000000000000000, -1.000000000000000000, 0.000000000000000000 ) ) ;
#24462 = CARTESIAN_POINT ( 'NONE',  ( -7.344253762436438571, -73.99970746456109794, 39.37955618711904293 ) ) ;
#24463 = CARTESIAN_POINT ( 'NONE',  ( 7.250043397162129644, -74.39270540171456503, -40.35498444578576738 ) ) ;
#24464 = ORIENTED_EDGE ( 'NONE', *, *, #1716, .T. ) ;
#24465 = LINE ( 'NONE', #8, #2052 ) ;
#24466 = EDGE_CURVE ( 'NONE', #17507, #11243, #8028, .T. ) ;
#24467 = CARTESIAN_POINT ( 'NONE',  ( 9.564509902230000193, -57.40875702419999982, -23.52622212079999997 ) ) ;
#24468 = DIRECTION ( 'NONE',  ( 1.000000000000000000, 0.000000000000000000, 0.000000000000000000 ) ) ;
#24469 = DIRECTION ( 'NONE',  ( 0.09756097560976997873, 0.000000000000000000, -0.9952295494196653491 ) ) ;
#24470 = DIRECTION ( 'NONE',  ( 0.000000000000000000, 1.000000000000000000, 0.000000000000000000 ) ) ;
#24471 = AXIS2_PLACEMENT_3D ( 'NONE', #18897, #27779, #18464 ) ;
#24472 = EDGE_CURVE ( 'NONE', #5884, #15706, #6205, .T. ) ;
#24473 = APPLICATION_PROTOCOL_DEFINITION ( 'draft international standard', 'automotive_design', 1998, #10323 ) ;
#24474 = ADVANCED_FACE ( 'NONE', ( #26059 ), #23856, .F. ) ;
#24475 = LINE ( 'NONE', #28678, #8363 ) ;
#24476 = ORIENTED_EDGE ( 'NONE', *, *, #12736, .T. ) ;
#24477 = B_SPLINE_CURVE_WITH_KNOTS ( 'NONE', 3,
 ( #16881, #21255, #5798, #12210 ),
 .UNSPECIFIED., .F., .F.,
 ( 4, 4 ),
 ( 1.645588054440000114, 2.780179228649999779 ),
 .UNSPECIFIED. ) ;
#24478 = FACE_OUTER_BOUND ( 'NONE', #14897, .T. ) ;
#24479 = CARTESIAN_POINT ( 'NONE',  ( 17.94519931069999785, -99.91547912500000450, 1.181841864839999756 ) ) ;
#24480 = ORIENTED_EDGE ( 'NONE', *, *, #11404, .F. ) ;
#24481 = CARTESIAN_POINT ( 'NONE',  ( -11.74919335509999918, -57.47571039350000177, 20.26880008290000035 ) ) ;
#24482 = FACE_OUTER_BOUND ( 'NONE', #18183, .T. ) ;
#24483 = VERTEX_POINT ( 'NONE', #22572 ) ;
#24484 = CARTESIAN_POINT ( 'NONE',  ( -6.903469049429999949, -74.00000000000000000, 46.75000000000000000 ) ) ;
#24485 = ORIENTED_EDGE ( 'NONE', *, *, #9159, .F. ) ;
#24486 = CARTESIAN_POINT ( 'NONE',  ( 22.55816085667000692, -34.67040743918621359, -0.5428485797609520214 ) ) ;
#24487 = CARTESIAN_POINT ( 'NONE',  ( 9.510880446319999848, -36.06003250090000023, -20.82958080039999871 ) ) ;
#24488 = DIRECTION ( 'NONE',  ( 0.000000000000000000, 1.000000000000000000, 0.000000000000000000 ) ) ;
#24489 = CARTESIAN_POINT ( 'NONE',  ( -11.16934527530000132, -19.15747282889999781, -18.98222458509999910 ) ) ;
#24490 = CARTESIAN_POINT ( 'NONE',  ( 22.66044434279999820, -66.11532834579999474, 11.96275783630000156 ) ) ;
#24491 = ORIENTED_EDGE ( 'NONE', *, *, #13361, .F. ) ;
#24492 = CARTESIAN_POINT ( 'NONE',  ( 12.21423488090000120, -93.96464232169999775, -21.69898374830000165 ) ) ;
#24493 = CARTESIAN_POINT ( 'NONE',  ( -20.38120117614986171, -61.35278060542812284, 12.44166777117195544 ) ) ;
#24494 = DIRECTION ( 'NONE',  ( 0.000000000000000000, 1.000000000000000000, 0.000000000000000000 ) ) ;
#24495 = CARTESIAN_POINT ( 'NONE',  ( -32.08195032130000612, -74.00665451570000641, -21.91676683800000092 ) ) ;
#24496 = ORIENTED_EDGE ( 'NONE', *, *, #13517, .F. ) ;
#24497 = DIRECTION ( 'NONE',  ( 0.000000000000000000, 1.000000000000000000, 0.000000000000000000 ) ) ;
#24498 = CARTESIAN_POINT ( 'NONE',  ( -15.81949116929999910, -92.71181266049998726, 23.89725124530000144 ) ) ;
#24499 = CARTESIAN_POINT ( 'NONE',  ( -14.48711453910000024, -79.93770852559998730, 37.01826959139999929 ) ) ;
#24500 = VERTEX_POINT ( 'NONE', #18042 ) ;
#24501 = CARTESIAN_POINT ( 'NONE',  ( 28.08445624330000001, -69.30631424429999754, 2.280942866869999808 ) ) ;
#24502 = CARTESIAN_POINT ( 'NONE',  ( 0.4062216120019999654, -101.0147083550000104, -15.54305921829999981 ) ) ;
#24503 = CARTESIAN_POINT ( 'NONE',  ( 27.75394116159999669, -74.50000000000000000, -27.75394116159999669 ) ) ;
#24504 = CARTESIAN_POINT ( 'NONE',  ( -19.65424240801501199, -57.45864753664992008, 13.63538986705772160 ) ) ;
#24505 = EDGE_CURVE ( 'NONE', #4023, #17027, #6682, .T. ) ;
#24506 = CARTESIAN_POINT ( 'NONE',  ( 23.33235093769999935, -63.43007729560000740, -8.903997769090000958 ) ) ;
#24507 = ADVANCED_FACE ( 'NONE', ( #15693 ), #12702, .F. ) ;
#24508 = CARTESIAN_POINT ( 'NONE',  ( 0.000000000000000000, -15.14308496720000008, 0.000000000000000000 ) ) ;
#24509 = EDGE_CURVE ( 'NONE', #20007, #21750, #22986, .T. ) ;
#24510 = EDGE_CURVE ( 'NONE', #723, #16270, #144, .T. ) ;
#24511 = CARTESIAN_POINT ( 'NONE',  ( 28.44836026452301070, -92.82668962668340384, 10.99730886889462056 ) ) ;
#24512 = CARTESIAN_POINT ( 'NONE',  ( 7.894724219650000485, -99.51557806589998734, 16.06685178089999866 ) ) ;
#24513 = B_SPLINE_CURVE_WITH_KNOTS ( 'NONE', 5,
 ( #14782, #23826, #3868, #12865, #1695, #10531 ),
 .UNSPECIFIED., .F., .F.,
 ( 6, 6 ),
 ( 0.000000000000000000, 1.000000000000000000 ),
 .UNSPECIFIED. ) ;
#24514 = CARTESIAN_POINT ( 'NONE',  ( 17.44131645659999919, -95.98460699740000734, 14.95162584959999919 ) ) ;
#24515 = DIRECTION ( 'NONE',  ( 0.000000000000000000, -1.000000000000000000, 0.000000000000000000 ) ) ;
#24516 = CARTESIAN_POINT ( 'NONE',  ( -47.25000000000000000, -82.25000000000000000, -8.214972755869998945E-15 ) ) ;
#24517 = B_SPLINE_SURFACE_WITH_KNOTS ( 'NONE', 5, 5, ( 
 ( #24729, #413, #4764, #564, #4904, #9409 ),
 ( #9263, #22836, #16110, #711, #13639, #20493 ),
 ( #2731, #7393, #18462, #11887, #20653, #22983 ),
 ( #20940, #2881, #13784, #22686, #13935, #18317 ),
 ( #9563, #11738, #16257, #25167, #18162, #20344 ),
 ( #25011, #2591, #27061, #853, #11585, #25317 ) ),
 .UNSPECIFIED., .F., .F., .F.,
 ( 6, 6 ),
 ( 6, 6 ),
 ( 16.61710410409999739, 20.91501685549999934 ),
 ( 0.000000000000000000, 2.000000000000000000 ),
 .UNSPECIFIED. ) ;
#24518 = CARTESIAN_POINT ( 'NONE',  ( 22.86947465604172436, -19.47453829777655443, 1.128719766882153364 ) ) ;
#24519 = CARTESIAN_POINT ( 'NONE',  ( -7.009104771800000577, -101.4908759489999994, 14.41751744779999989 ) ) ;
#24520 = ORIENTED_EDGE ( 'NONE', *, *, #24509, .F. ) ;
#24521 = CARTESIAN_POINT ( 'NONE',  ( 26.81678742717032193, -72.67627779146050671, -10.37109992809414827 ) ) ;
#24522 = CARTESIAN_POINT ( 'NONE',  ( 9.175366638180001644, -35.90614572970000040, -19.93301557890000097 ) ) ;
#24523 = CARTESIAN_POINT ( 'NONE',  ( -36.83844719860000083, -65.17124718639999514, -0.1954025812290000053 ) ) ;
#24524 = ORIENTED_EDGE ( 'NONE', *, *, #15198, .T. ) ;
#24525 = CARTESIAN_POINT ( 'NONE',  ( 9.279094190520000396, -98.48918237500001283, 16.48187022329999962 ) ) ;
#24526 = CARTESIAN_POINT ( 'NONE',  ( 21.34453858160000195, -18.50000000000000000, -0.07199018194310001506 ) ) ;
#24527 = CARTESIAN_POINT ( 'NONE',  ( -0.8449272815640000989, -98.83667233820000320, -18.63222145299999966 ) ) ;
#24528 = CARTESIAN_POINT ( 'NONE',  ( -19.92928515724098659, -92.55017404142323301, -23.08838732444159092 ) ) ;
#24529 = CARTESIAN_POINT ( 'NONE',  ( -15.50938067939999954, -101.3150705480000084, 4.855933298290000089 ) ) ;
#24530 = CIRCLE ( 'NONE', #17559, 55.67692378859999991 ) ;
#24531 = CARTESIAN_POINT ( 'NONE',  ( 12.90275855517485049, -96.31541554714243603, 17.28766916121755770 ) ) ;
#24532 = DIRECTION ( 'NONE',  ( 0.4794255386042032829, 0.000000000000000000, 0.8775825618903726477 ) ) ;
#24534 = EDGE_CURVE ( 'NONE', #8919, #13409, #28075, .T. ) ;
#24533 = LINE ( 'NONE', #22069, #18128 ) ;
#24535 = CARTESIAN_POINT ( 'NONE',  ( 7.215414233289999757, -82.25000000000000000, -40.70731707320000226 ) ) ;
#24536 = DIRECTION ( 'NONE',  ( 0.000000000000000000, 1.000000000000000000, 0.000000000000000000 ) ) ;
#24537 = CARTESIAN_POINT ( 'NONE',  ( 24.70175895849127912, -93.12686943433988063, -14.84027023513776200 ) ) ;
#24538 = CARTESIAN_POINT ( 'NONE',  ( 24.27624741938561570, -93.55106866556637613, 12.16912909751702720 ) ) ;
#24539 = ORIENTED_EDGE ( 'NONE', *, *, #1831, .T. ) ;
#24540 = EDGE_CURVE ( 'NONE', #28390, #27862, #15548, .T. ) ;
#24541 = CARTESIAN_POINT ( 'NONE',  ( 0.000000000000000000, -15.00000000000000000, 0.000000000000000000 ) ) ;
#24542 = CARTESIAN_POINT ( 'NONE',  ( 8.071148094770000725, -100.8816835939999947, 13.57632622700000091 ) ) ;
#24543 = CONICAL_SURFACE ( 'NONE', #22216, 5.999999999999999112, 0.7853981633970000820 ) ;
#24544 = ADVANCED_FACE ( 'NONE', ( #8993 ), #8039, .T. ) ;
#24545 = COLOUR_RGB ( '', 0.40784314, 0.44705882, 0.49803922) ;
#24546 = EDGE_LOOP ( 'NONE', ( #1491, #23281, #27742 ) ) ;
#24547 = CARTESIAN_POINT ( 'NONE',  ( -12.69597419230000135, -65.01950817790000769, 21.68734838749999838 ) ) ;
#24548 = CARTESIAN_POINT ( 'NONE',  ( -13.88246128279999958, -63.14781701039999717, 21.47252710969999967 ) ) ;
#24549 = CARTESIAN_POINT ( 'NONE',  ( 7.102042752109999135, -111.0000000000000000, 14.33739825589999839 ) ) ;
#24550 = CARTESIAN_POINT ( 'NONE',  ( -24.07227057460000097, -94.80026553589999594, -4.144178597490000726 ) ) ;
#24551 = CARTESIAN_POINT ( 'NONE',  ( -20.25037018340000117, -54.99674360790000094, 14.65440538810000071 ) ) ;
#24552 = CARTESIAN_POINT ( 'NONE',  ( -11.13193851743714191, -32.10667435364714350, -22.10121990970652561 ) ) ;
#24553 = ORIENTED_EDGE ( 'NONE', *, *, #21490, .T. ) ;
#24554 = CARTESIAN_POINT ( 'NONE',  ( -40.00000000000000000, -94.00000000000000000, 0.000000000000000000 ) ) ;
#24555 = CARTESIAN_POINT ( 'NONE',  ( 30.16735348728591504, -74.23014832817669628, -24.98698552860614797 ) ) ;
#24556 = TOROIDAL_SURFACE ( 'NONE', #10122, 7.750000000000000000, 0.5000000000000000000 ) ;
#24557 = CARTESIAN_POINT ( 'NONE',  ( 7.332363419890000067, -74.23956954040001222, -39.85902549529999561 ) ) ;
#24558 = ORIENTED_EDGE ( 'NONE', *, *, #27939, .F. ) ;
#24559 = CARTESIAN_POINT ( 'NONE',  ( 7.312846564840000063, -92.50000000000000000, 29.61034067890000188 ) ) ;
#24560 = FACE_OUTER_BOUND ( 'NONE', #12266, .T. ) ;
#24561 = DIRECTION ( 'NONE',  ( 0.000000000000000000, 1.000000000000000000, 0.000000000000000000 ) ) ;
#24562 = CARTESIAN_POINT ( 'NONE',  ( 19.94281239099999681, -26.09793778660000285, 10.08502759879999999 ) ) ;
#24563 = DIRECTION ( 'NONE',  ( 0.000000000000000000, -1.000000000000000000, 0.000000000000000000 ) ) ;
#24564 = CARTESIAN_POINT ( 'NONE',  ( 24.44279401320000034, -92.66001714109999909, -13.69981297090000005 ) ) ;
#24565 = AXIS2_PLACEMENT_3D ( 'NONE', #14062, #18297, #22815 ) ;
#24566 = CARTESIAN_POINT ( 'NONE',  ( 20.22035593609999893, -19.15979404320000157, 9.591164680889999516 ) ) ;
#24567 = CARTESIAN_POINT ( 'NONE',  ( 8.386163660559999400, -68.18701866809999501, -25.21061429379999907 ) ) ;
#24568 = CARTESIAN_POINT ( 'NONE',  ( -17.43464046073879814, -96.56053630746443162, 12.16311153714526050 ) ) ;
#24569 = ORIENTED_EDGE ( 'NONE', *, *, #15788, .T. ) ;
#24570 = AXIS2_PLACEMENT_3D ( 'NONE', #9910, #16759, #23056 ) ;
#24571 = CARTESIAN_POINT ( 'NONE',  ( -14.67079199201519657, -67.87586507525224988, 22.52608771271433596 ) ) ;
#24572 = CARTESIAN_POINT ( 'NONE',  ( 27.25648091989999955, -93.00000000000000000, -13.26500883389999963 ) ) ;
#24573 = CARTESIAN_POINT ( 'NONE',  ( -11.94559458280000008, -100.4792519539999915, -10.93369168340000108 ) ) ;
#24574 = DIRECTION ( 'NONE',  ( 0.4794255386042041156, 0.000000000000000000, 0.8775825618903722036 ) ) ;
#24575 = CARTESIAN_POINT ( 'NONE',  ( -39.96405813100000159, -74.08838618849999591, -7.268564243729999319 ) ) ;
#24576 = EDGE_LOOP ( 'NONE', ( #23626, #12157, #21305, #8394, #24093, #8266, #4339 ) ) ;
#24577 = EDGE_CURVE ( 'NONE', #3729, #10287, #2837, .T. ) ;
#24578 = B_SPLINE_CURVE_WITH_KNOTS ( 'NONE', 5,
 ( #22302, #22159, #588, #8727, #25036, #22863, #9432, #5070, #735 ),
 .UNSPECIFIED., .F., .F.,
 ( 6, 3, 6 ),
 ( 0.000000000000000000, 0.5000000000000000000, 1.000000000000000000 ),
 .UNSPECIFIED. ) ;
#24579 = CARTESIAN_POINT ( 'NONE',  ( 26.34682155151427096, -92.82044061126494228, -15.36538583964133053 ) ) ;
#24580 = PRODUCT_DEFINITION_FORMATION_WITH_SPECIFIED_SOURCE ( 'ANY', '', #26194, .NOT_KNOWN. ) ;
#24581 = VERTEX_POINT ( 'NONE', #5077 ) ;
#24582 = ADVANCED_FACE ( 'NONE', ( #4642 ), #7643, .F. ) ;
#24583 = B_SPLINE_SURFACE_WITH_KNOTS ( 'NONE', 5, 5, ( 
 ( #24457, #443, #11171, #4933, #303, #9440, #26944, #6986, #149 ),
 ( #27090, #9001, #596, #11617, #20527, #24903, #7131, #15850, #24759 ),
 ( #13672, #22577, #14670, #23290, #18639, #16442, #5649, #19057, #14115 ),
 ( #1167, #3470, #14259, #27535, #14527, #7978, #7423, #27800, #16724 ),
 ( #2909, #18920, #16868, #5511, #27942, #3333, #12197, #12335, #25757 ),
 ( #25201, #5230, #21112, #7716, #25477, #11919, #23014, #9872, #11771 ),
 ( #5785, #14398, #20971, #10006, #20822, #12055, #18786, #7842, #25620 ),
 ( #3064, #9726, #23152, #23434, #21243, #884, #7578, #25346, #3197 ),
 ( #1034, #1294, #10137, #20683, #5376, #16290, #744, #27678, #9589 ),
 ( #16583, #18489, #27380, #12462, #19187, #8667, #14935, #17139, #17575 ),
 ( #8244, #17435, #23839, #3882, #12747, #10279, #26029, #23564, #21375 ),
 ( #6055, #21659, #6500, #19748, #1707, #28636, #8113, #3602, #6208 ) ),
 .UNSPECIFIED., .F., .F., .F.,
 ( 6, 3, 3, 6 ),
 ( 6, 3, 6 ),
 ( 3.365447998909999683, 5.319894352600000431, 6.690827956829999756, 7.896981424030000696 ),
 ( 0.000000000000000000, 0.2500000000000000000, 0.5000000000000000000 ),
 .UNSPECIFIED. ) ;
#24584 = CARTESIAN_POINT ( 'NONE',  ( 0.000000000000000000, -57.47855601759999900, 0.000000000000000000 ) ) ;
#24585 = PLANE ( 'NONE',  #28790 ) ;
#24586 = CARTESIAN_POINT ( 'NONE',  ( 12.79650330539999992, -92.63554657719998886, 27.41785451570000021 ) ) ;
#24587 = ORIENTED_EDGE ( 'NONE', *, *, #7215, .F. ) ;
#24588 = VECTOR ( 'NONE', #26806, 1000.000000000000000 ) ;
#24589 = AXIS2_PLACEMENT_3D ( 'NONE', #6453, #13149, #26141 ) ;
#24590 = CARTESIAN_POINT ( 'NONE',  ( 0.000000000000000000, -83.75000000000000000, 0.000000000000000000 ) ) ;
#24591 = ORIENTED_EDGE ( 'NONE', *, *, #6428, .F. ) ;
#24592 = CARTESIAN_POINT ( 'NONE',  ( -40.50000000000000000, -12.50000000000000000, 4.500000000000000000 ) ) ;
#24593 = CARTESIAN_POINT ( 'NONE',  ( -13.16183723299999997, -70.12921532840000793, -24.09258145020000086 ) ) ;
#24594 = CARTESIAN_POINT ( 'NONE',  ( 27.68682485439999752, -13.40000000000000036, 50.68039294919999804 ) ) ;
#24595 = ORIENTED_EDGE ( 'NONE', *, *, #25740, .T. ) ;
#24596 = DIRECTION ( 'NONE',  ( 0.000000000000000000, 1.000000000000000000, 0.000000000000000000 ) ) ;
#24597 = CARTESIAN_POINT ( 'NONE',  ( -22.19845100579999908, -79.83484740680000868, -32.70622245319999877 ) ) ;
#24598 = ADVANCED_FACE ( 'NONE', ( #20232 ), #7273, .F. ) ;
#24599 = DIRECTION ( 'NONE',  ( 0.7678754814159398645, 0.000000000000000000, -0.6405991297529514128 ) ) ;
#24600 = CARTESIAN_POINT ( 'NONE',  ( -13.34720188679999886, -94.24983875549999368, -21.61594323940000351 ) ) ;
#24601 = LINE ( 'NONE', #28660, #19404 ) ;
#24602 = ORIENTED_EDGE ( 'NONE', *, *, #28003, .T. ) ;
#24603 = CYLINDRICAL_SURFACE ( 'NONE', #17643, 57.74999999999999289 ) ;
#24604 = CARTESIAN_POINT ( 'NONE',  ( -2.644509777640000170, -62.27955658970000030, -25.79865804869999835 ) ) ;
#24605 = CARTESIAN_POINT ( 'NONE',  ( -39.64142120219999299, -73.82497517469998627, 7.260602597430000138 ) ) ;
#24606 = CARTESIAN_POINT ( 'NONE',  ( -21.92609131280000057, -74.01492597349999869, -32.13963591329999758 ) ) ;
#24607 = CARTESIAN_POINT ( 'NONE',  ( -2.353367408570000041, -57.44036991819999827, -24.34032937810000163 ) ) ;
#24608 = CARTESIAN_POINT ( 'NONE',  ( -12.35307240344411994, -101.1962283502562059, -8.971858293833401277 ) ) ;
#24609 = CARTESIAN_POINT ( 'NONE',  ( 21.02965361369999897, -18.50000000000000000, -0.4426258060200000122 ) ) ;
#24610 = CARTESIAN_POINT ( 'NONE',  ( 28.66244647610000129, -91.50000000000000000, 10.42660836539999991 ) ) ;
#24611 = CARTESIAN_POINT ( 'NONE',  ( -18.04642050529999864, -18.61786835250000038, 12.22684699669999908 ) ) ;
#24612 = VERTEX_POINT ( 'NONE', #13367 ) ;
#24613 = CIRCLE ( 'NONE', #6002, 10.49999999999999822 ) ;
#24614 = AXIS2_PLACEMENT_3D ( 'NONE', #8969, #6955, #17875 ) ;
#24615 = ADVANCED_FACE ( 'NONE', ( #20374 ), #24583, .T. ) ;
#24617 = ADVANCED_FACE ( 'NONE', ( #10694 ), #10373, .F. ) ;
#24616 = CARTESIAN_POINT ( 'NONE',  ( -10.69999465949999973, -93.40479992090000394, -23.45152081580000214 ) ) ;
#24618 = AXIS2_PLACEMENT_3D ( 'NONE', #17064, #1771, #21584 ) ;
#24619 = DIRECTION ( 'NONE',  ( 1.000000000000000000, 0.000000000000000000, 0.000000000000000000 ) ) ;
#24620 = CARTESIAN_POINT ( 'NONE',  ( -24.48306397703444048, -92.50630337894787658, -18.18918482052484720 ) ) ;
#24621 = CARTESIAN_POINT ( 'NONE',  ( 40.65853658540000026, -84.00000000000000000, -6.717799458580000049 ) ) ;
#24622 = CARTESIAN_POINT ( 'NONE',  ( 45.99664575370000108, -80.06168502749999050, -4.396813293179999249 ) ) ;
#24623 = EDGE_CURVE ( 'NONE', #6901, #19131, #17849, .T. ) ;
#24624 = B_SPLINE_CURVE_WITH_KNOTS ( 'NONE', 3,
 ( #24128, #11132, #20198, #15515, #26912, #22098, #24726, #20051, #18013, #24275, #271, #6349 ),
 .UNSPECIFIED., .F., .F.,
 ( 4, 2, 2, 2, 2, 4 ),
 ( 0.000000000000000000, 0.2499999999999988898, 0.3749999999999893974, 0.4374999999999802935, 0.4999999999999711897, 1.000000000000000000 ),
 .UNSPECIFIED. ) ;
#24625 = DIRECTION ( 'NONE',  ( 0.7071067811865475727, 0.000000000000000000, -0.7071067811865475727 ) ) ;
#24626 = ORIENTED_EDGE ( 'NONE', *, *, #23788, .F. ) ;
#24627 = CYLINDRICAL_SURFACE ( 'NONE', #7547, 2.999999999999996447 ) ;
#24628 = CARTESIAN_POINT ( 'NONE',  ( 24.39713799250000292, -19.50000027030000282, 1.459766484860000046 ) ) ;
#24630 = ORIENTED_EDGE ( 'NONE', *, *, #16236, .T. ) ;
#24629 = CIRCLE ( 'NONE', #22774, 22.03370205219999889 ) ;
#24631 = DIRECTION ( 'NONE',  ( 0.000000000000000000, -1.000000000000000000, 0.000000000000000000 ) ) ;
#24632 = ORIENTED_EDGE ( 'NONE', *, *, #3531, .F. ) ;
#24633 = DIRECTION ( 'NONE',  ( 0.000000000000000000, 1.000000000000000000, 0.000000000000000000 ) ) ;
#24634 = VECTOR ( 'NONE', #9175, 1000.000000000000000 ) ;
#24635 = AXIS2_PLACEMENT_3D ( 'NONE', #7470, #1202, #27273 ) ;
#24636 = AXIS2_PLACEMENT_3D ( 'NONE', #9257, #19889, #20046 ) ;
#24637 = ADVANCED_FACE ( 'NONE', ( #28077 ), #15725, .T. ) ;
#24638 = B_SPLINE_CURVE_WITH_KNOTS ( 'NONE', 5,
 ( #27333, #7803, #7678, #14356, #13920, #25577, #23250, #3294, #9547 ),
 .UNSPECIFIED., .F., .F.,
 ( 6, 3, 6 ),
 ( 0.000000000000000000, 0.3290135944274085733, 1.000000000000000000 ),
 .UNSPECIFIED. ) ;
#24639 = EDGE_CURVE ( 'NONE', #20422, #1013, #17728, .T. ) ;
#24640 = CARTESIAN_POINT ( 'NONE',  ( 8.040406065020551551, -94.10917102489311503, -24.59531423993398036 ) ) ;
#24641 = DIRECTION ( 'NONE',  ( 1.000000000000000000, 0.000000000000000000, 0.000000000000000000 ) ) ;
#24642 = LINE ( 'NONE', #22305, #3426 ) ;
#24643 = CARTESIAN_POINT ( 'NONE',  ( -10.66538705860000036, -19.49268907760000147, -21.54408461599999924 ) ) ;
#24644 = CARTESIAN_POINT ( 'NONE',  ( 21.56055435100278928, -37.66855076750636755, -7.904811894883319923 ) ) ;
#24645 = ORIENTED_EDGE ( 'NONE', *, *, #21392, .F. ) ;
#24646 = DIRECTION ( 'NONE',  ( 1.000000000000000000, 0.000000000000000000, 0.000000000000000000 ) ) ;
#24647 = LINE ( 'NONE', #20568, #21448 ) ;
#24648 = DIRECTION ( 'NONE',  ( 0.000000000000000000, 1.000000000000000000, 0.000000000000000000 ) ) ;
#24649 = CARTESIAN_POINT ( 'NONE',  ( -32.53182592119999583, -74.14930846740000447, -21.71085396679999846 ) ) ;
#24650 = ORIENTED_EDGE ( 'NONE', *, *, #2210, .F. ) ;
#24651 = ADVANCED_FACE ( 'NONE', ( #24866 ), #28775, .F. ) ;
#24652 = CARTESIAN_POINT ( 'NONE',  ( 0.000000000000000000, -13.40000000000000036, 0.000000000000000000 ) ) ;
#24653 = CARTESIAN_POINT ( 'NONE',  ( -17.77445941079999869, -93.74388477669999986, 19.47957637960000099 ) ) ;
#24654 = CARTESIAN_POINT ( 'NONE',  ( 12.03978574509999966, -15.00000000000000000, 22.03867997850000293 ) ) ;
#24655 = CARTESIAN_POINT ( 'NONE',  ( -16.03899174369999869, -99.57125562240000249, 6.799714415290000424 ) ) ;
#24656 = CARTESIAN_POINT ( 'NONE',  ( 0.5505338958400000093, -101.0875971110000080, -15.39929819530000010 ) ) ;
#24657 = CARTESIAN_POINT ( 'NONE',  ( -3.215510237749999778, -94.59276292389999696, 23.57860181210000405 ) ) ;
#24658 = CARTESIAN_POINT ( 'NONE',  ( 22.06429904920000240, -36.00000000000000000, -11.19681729669999903 ) ) ;
#24659 = CARTESIAN_POINT ( 'NONE',  ( -10.76183065640000081, -34.65282384500000035, -20.56657588450000063 ) ) ;
#24660 = VECTOR ( 'NONE', #15025, 1000.000000000000114 ) ;
#24661 = CIRCLE ( 'NONE', #16265, 1.000000000000000888 ) ;
#24662 = CARTESIAN_POINT ( 'NONE',  ( 7.100891874899999401, -99.78393592979999482, 15.80033508019999822 ) ) ;
#24663 = FACE_OUTER_BOUND ( 'NONE', #21232, .T. ) ;
#24664 = VERTEX_POINT ( 'NONE', #15362 ) ;
#24665 = CARTESIAN_POINT ( 'NONE',  ( -13.52989530590000022, -92.50182112220001329, 26.44972089899999901 ) ) ;
#24666 = CARTESIAN_POINT ( 'NONE',  ( 12.61928293329999917, -98.69239344479998977, 15.21635193949999909 ) ) ;
#24667 = ORIENTED_EDGE ( 'NONE', *, *, #24174, .F. ) ;
#24668 = CARTESIAN_POINT ( 'NONE',  ( 7.260602597430000138, -73.82497517469998627, 39.64142120219999299 ) ) ;
#24669 = CARTESIAN_POINT ( 'NONE',  ( 22.54964778510000301, -92.87437365150000801, 15.59122118179999994 ) ) ;
#24670 = CARTESIAN_POINT ( 'NONE',  ( 20.72386479999999764, -35.83655893530000469, -8.803829908180000885 ) ) ;
#24671 = ORIENTED_EDGE ( 'NONE', *, *, #14848, .F. ) ;
#24672 = CARTESIAN_POINT ( 'NONE',  ( -3.562216332169999777, -80.49999996399999702, 46.31451619710000500 ) ) ;
#24673 = CYLINDRICAL_SURFACE ( 'NONE', #23239, 0.5000000000000004441 ) ;
#24674 = CARTESIAN_POINT ( 'NONE',  ( 8.236135946259999230, -37.13048524220000246, -21.55877352099999911 ) ) ;
#24675 = EDGE_CURVE ( 'NONE', #14159, #13154, #7007, .T. ) ;
#24676 = VECTOR ( 'NONE', #22837, 1000.000000000000000 ) ;
#24677 = CARTESIAN_POINT ( 'NONE',  ( 45.99664576247111114, -73.93831497102631545, -4.396813278696650507 ) ) ;
#24678 = ORIENTED_EDGE ( 'NONE', *, *, #18544, .T. ) ;
#24680 = EDGE_CURVE ( 'NONE', #15502, #19846, #27179, .T. ) ;
#24679 = AXIS2_PLACEMENT_3D ( 'NONE', #19112, #5293, #16924 ) ;
#24681 = CARTESIAN_POINT ( 'NONE',  ( -0.6842253571740000151, -101.2530993000000024, -15.17849927279999989 ) ) ;
#24682 = CARTESIAN_POINT ( 'NONE',  ( -29.63524900250000016, -92.56168957700000988, -0.5035227619879999450 ) ) ;
#24683 = CARTESIAN_POINT ( 'NONE',  ( -3.898844501749999747, -96.83679385029999764, -20.89542445309999863 ) ) ;
#24684 = CARTESIAN_POINT ( 'NONE',  ( -2.619606055569999814, -19.50000000000000000, -24.29997775220000023 ) ) ;
#24685 = ADVANCED_FACE ( 'NONE', ( #11581 ), #15483, .T. ) ;
#24686 = CARTESIAN_POINT ( 'NONE',  ( 11.86655925200000183, -101.3150705500000157, -11.10431217030000006 ) ) ;
#24687 = CARTESIAN_POINT ( 'NONE',  ( 14.95895049385062059, -95.29940929529944071, 17.31812158372859045 ) ) ;
#24688 = EDGE_CURVE ( 'NONE', #8180, #18987, #11318, .T. ) ;
#24689 = CARTESIAN_POINT ( 'NONE',  ( 25.57735248450000043, -37.08699221940000257, 46.81902967690000139 ) ) ;
#24690 = SHAPE_REPRESENTATION ( 'Housing Torx Attachment Screw', ( #26433 ), #5492 ) ;
#24691 = CARTESIAN_POINT ( 'NONE',  ( 25.70538116001676343, -61.18778281473014857, 1.399642238291860741 ) ) ;
#24692 = CARTESIAN_POINT ( 'NONE',  ( 29.08514934200000113, -10.00000000000000000, 53.24000875469999983 ) ) ;
#24693 = CARTESIAN_POINT ( 'NONE',  ( -14.33930122880000013, -18.50000000000000000, 19.87761826330000048 ) ) ;
#24694 = ORIENTED_EDGE ( 'NONE', *, *, #2561, .T. ) ;
#24695 = CARTESIAN_POINT ( 'NONE',  ( -29.76177017585215268, -92.96960399592616398, 6.669860268962034766 ) ) ;
#24696 = CARTESIAN_POINT ( 'NONE',  ( 8.188640737180000073, -100.9197086730000024, 13.30685945699999984 ) ) ;
#24697 = AXIS2_PLACEMENT_3D ( 'NONE', #27690, #18798, #16302 ) ;
#24698 = CIRCLE ( 'NONE', #20021, 19.50000000000000000 ) ;
#24699 = ORIENTED_EDGE ( 'NONE', *, *, #7396, .T. ) ;
#24700 = AXIS2_PLACEMENT_3D ( 'NONE', #24286, #26040, #13202 ) ;
#24701 = CARTESIAN_POINT ( 'NONE',  ( -14.70960788549999876, -64.89138858019998679, 22.30467294780000032 ) ) ;
#24702 = CARTESIAN_POINT ( 'NONE',  ( -12.03855289290000030, -63.62219628589998877, 21.32965301300000149 ) ) ;
#24703 = DIRECTION ( 'NONE',  ( 0.000000000000000000, -1.000000000000000000, 0.000000000000000000 ) ) ;
#24704 = B_SPLINE_CURVE_WITH_KNOTS ( 'NONE', 5,
 ( #23518, #5730, #12409, #1938, #8195, #10361 ),
 .UNSPECIFIED., .F., .F.,
 ( 6, 6 ),
 ( 0.000000000000000000, 1.000000000000000000 ),
 .UNSPECIFIED. ) ;
#24705 = CARTESIAN_POINT ( 'NONE',  ( 19.97576656849999921, -72.00000000000000000, -19.97576656849999921 ) ) ;
#24706 = CARTESIAN_POINT ( 'NONE',  ( -6.717799458580000049, -84.50000000000000000, 40.65853658540000026 ) ) ;
#24707 = CARTESIAN_POINT ( 'NONE',  ( 16.60616815699999904, -99.99711545080000974, 4.374379691520000613 ) ) ;
#24708 = ORIENTED_EDGE ( 'NONE', *, *, #11232, .F. ) ;
#24709 = CARTESIAN_POINT ( 'NONE',  ( 16.48132342839999964, -101.1889999979999999, 2.988055897779999803 ) ) ;
#24710 = SURFACE_STYLE_USAGE ( .BOTH. , #2131 ) ;
#24711 = CARTESIAN_POINT ( 'NONE',  ( -22.13586109129999713, -95.90105813160000992, -5.885152931789999542 ) ) ;
#24712 = ORIENTED_EDGE ( 'NONE', *, *, #20028, .F. ) ;
#24713 = CARTESIAN_POINT ( 'NONE',  ( 8.955369301398645732, -92.77481473455837602, 29.15572894638344792 ) ) ;
#24714 = ORIENTED_EDGE ( 'NONE', *, *, #938, .T. ) ;
#24715 = EDGE_CURVE ( 'NONE', #6398, #2162, #2511, .T. ) ;
#24716 = CARTESIAN_POINT ( 'NONE',  ( -3.883346862689999845, -2.000000000000000000, -7.108418751309999450 ) ) ;
#24717 = CARTESIAN_POINT ( 'NONE',  ( -38.17962778057142970, -63.35319846927643539, 1.206297397038823771 ) ) ;
#24718 = CARTESIAN_POINT ( 'NONE',  ( 21.88967610470000125, -26.05152176780000062, 9.642051993350001737 ) ) ;
#24719 = AXIS2_PLACEMENT_3D ( 'NONE', #15003, #12817, #24052 ) ;
#24720 = FACE_BOUND ( 'NONE', #22495, .T. ) ;
#24721 = CARTESIAN_POINT ( 'NONE',  ( -7.248307137522662202, -73.87844996482024840, -39.84323359139859377 ) ) ;
#24722 = AXIS2_PLACEMENT_3D ( 'NONE', #17553, #26011, #3866 ) ;
#24723 = EDGE_CURVE ( 'NONE', #17228, #17023, #13598, .T. ) ;
#24724 = AXIS2_PLACEMENT_3D ( 'NONE', #15938, #24845, #9233 ) ;
#24725 = CARTESIAN_POINT ( 'NONE',  ( 21.02834797730000105, -61.82803953129999996, 11.46254203570000030 ) ) ;
#24726 = CARTESIAN_POINT ( 'NONE',  ( -32.75213543914213687, -79.89792018864659440, -22.42386398948077186 ) ) ;
#24727 = CARTESIAN_POINT ( 'NONE',  ( -16.10740345911051108, -99.26499635306740288, 7.485719296024102576 ) ) ;
#24728 = ORIENTED_EDGE ( 'NONE', *, *, #21648, .F. ) ;
#24729 = CARTESIAN_POINT ( 'NONE',  ( -12.04650753100000138, -69.29982884310000202, -25.46956806070000212 ) ) ;
#24730 = CARTESIAN_POINT ( 'NONE',  ( 46.25000000000000000, -79.00000000000000000, -13.75000000000000000 ) ) ;
#24731 = CARTESIAN_POINT ( 'NONE',  ( -13.06366830770000043, -99.99711545080000974, -11.14632625079999961 ) ) ;
#24732 = CARTESIAN_POINT ( 'NONE',  ( 20.72577587939499466, -19.47314420526457468, 9.500409951011533849 ) ) ;
#24733 = CARTESIAN_POINT ( 'NONE',  ( -39.89376887310000086, -74.19145175629999756, -7.305188533560000863 ) ) ;
#24734 = ORIENTED_EDGE ( 'NONE', *, *, #22310, .F. ) ;
#24735 = DIRECTION ( 'NONE',  ( 1.000000000000000000, 0.000000000000000000, 0.000000000000000000 ) ) ;
#24736 = ORIENTED_EDGE ( 'NONE', *, *, #28680, .T. ) ;
#24737 = AXIS2_PLACEMENT_3D ( 'NONE', #27893, #3014, #21204 ) ;
#24738 = DIRECTION ( 'NONE',  ( 0.6285074900730004410, 0.000000000000000000, -0.7778035323410003032 ) ) ;
#24739 = CARTESIAN_POINT ( 'NONE',  ( -0.8151677527090001041, -95.98460638129999722, 22.95835728570000001 ) ) ;
#24740 = AXIS2_PLACEMENT_3D ( 'NONE', #17546, #4133, #13301 ) ;
#24741 = CARTESIAN_POINT ( 'NONE',  ( 5.626505627759999406, -93.46569726110000431, 26.69085374259999810 ) ) ;
#24742 = AXIS2_PLACEMENT_3D ( 'NONE', #6820, #15981, #13058 ) ;
#24743 = ORIENTED_EDGE ( 'NONE', *, *, #13150, .F. ) ;
#24744 = FACE_OUTER_BOUND ( 'NONE', #13844, .T. ) ;
#24745 = VERTEX_POINT ( 'NONE', #1780 ) ;
#24746 = CARTESIAN_POINT ( 'NONE',  ( -22.49369758140129960, -69.04718673991095557, 14.86230851755990123 ) ) ;
#24747 = CARTESIAN_POINT ( 'NONE',  ( 21.02256860540000005, -93.91547409650000588, 13.07290323880000038 ) ) ;
#24748 = CARTESIAN_POINT ( 'NONE',  ( 46.63164392270000036, -73.99951332550000416, -3.186587667189999529 ) ) ;
#24749 = ORIENTED_EDGE ( 'NONE', *, *, #12507, .F. ) ;
#24750 = DIRECTION ( 'NONE',  ( 0.000000000000000000, 1.000000000000000000, 0.000000000000000000 ) ) ;
#24751 = CARTESIAN_POINT ( 'NONE',  ( -21.91703890630000018, -80.37806415250000214, -32.56305777900000464 ) ) ;
#24752 = EDGE_CURVE ( 'NONE', #790, #9831, #14634, .T. ) ;
#24753 = CARTESIAN_POINT ( 'NONE',  ( 11.84128442000000092, -101.1848541609999899, -9.660509526330001151 ) ) ;
#24754 = CARTESIAN_POINT ( 'NONE',  ( -13.18688177930000016, -93.32822605769999313, -23.58441486170000090 ) ) ;
#24755 = CARTESIAN_POINT ( 'NONE',  ( -47.25000000000000000, -73.00000000000000000, 3.352534721190000231E-15 ) ) ;
#24756 = ORIENTED_EDGE ( 'NONE', *, *, #24577, .T. ) ;
#24757 = EDGE_CURVE ( 'NONE', #6342, #5907, #1440, .T. ) ;
#24758 = DIRECTION ( 'NONE',  ( 0.000000000000000000, 1.000000000000000000, 0.000000000000000000 ) ) ;
#24759 = CARTESIAN_POINT ( 'NONE',  ( -16.91430575710000284, -100.0771588430000065, 3.341621066080000091 ) ) ;
#24760 = CARTESIAN_POINT ( 'NONE',  ( -38.71641004229999794, -73.65707963269998970, 7.135467526410000261 ) ) ;
#24761 = CARTESIAN_POINT ( 'NONE',  ( -21.89190459030000113, -74.01117791779999777, -32.13651045809999829 ) ) ;
#24762 = CARTESIAN_POINT ( 'NONE',  ( -29.41275679339999982, -39.50000000000000000, -53.83969017199999740 ) ) ;
#24763 = LINE ( 'NONE', #17913, #24588 ) ;
#24764 = CIRCLE ( 'NONE', #16378, 9.500000000000000000 ) ;
#24765 = CARTESIAN_POINT ( 'NONE',  ( -7.485783351098411309, -73.99989201511671411, 38.96042338819187023 ) ) ;
#24766 = CARTESIAN_POINT ( 'NONE',  ( -18.55525302259999876, -19.15716910929999628, 11.86885460969999784 ) ) ;
#24767 = EDGE_LOOP ( 'NONE', ( #3022, #3185 ) ) ;
#24768 = DIRECTION ( 'NONE',  ( -1.000000000000000000, 0.000000000000000000, 0.000000000000000000 ) ) ;
#24769 = CARTESIAN_POINT ( 'NONE',  ( 10.33697414329999908, -72.00000000000000000, -28.69893982729999848 ) ) ;
#24770 = CARTESIAN_POINT ( 'NONE',  ( 7.936588789669999144, -35.30313509529999294, -21.23424077629999829 ) ) ;
#24771 = CARTESIAN_POINT ( 'NONE',  ( 15.69647852281674538, -101.4241070620424381, 3.898789967113180932 ) ) ;
#24772 = DIRECTION ( 'NONE',  ( 1.000000000000000000, 0.000000000000000000, 0.000000000000000000 ) ) ;
#24773 = CARTESIAN_POINT ( 'NONE',  ( 47.25045229320000573, -79.27360113529999808, -0.9350416584460000680 ) ) ;
#24774 = B_SPLINE_SURFACE_WITH_KNOTS ( 'NONE', 4, 5, ( 
 ( #5107, #1191, #9613, #7864, #24930, #18374, #13991, #22897, #11797 ),
 ( #20710, #768, #18514, #27407, #28371, #19210, #8264, #28099, #17309 ),
 ( #10715, #12770, #21540, #3767, #12353, #8138, #12487, #4041, #12906 ),
 ( #23724, #21822, #8403, #6229, #24005, #19482, #1872, #26202, #19355 ),
 ( #10159, #19079, #17161, #19630, #12628, #1596, #25782, #1728, #10569 ) ),
 .UNSPECIFIED., .F., .F., .F.,
 ( 5, 5 ),
 ( 6, 3, 6 ),
 ( 8.029182300089999980E-15, 6.855861996789999857 ),
 ( 0.000000000000000000, 1.000000000000000000, 2.000000000000000000 ),
 .UNSPECIFIED. ) ;
#24775 = CARTESIAN_POINT ( 'NONE',  ( 25.32712259480000228, -57.40875702469999453, 1.379782074460000230 ) ) ;
#24776 = CARTESIAN_POINT ( 'NONE',  ( 8.028473304129999377, -18.50000000000000000, -18.85230009969999898 ) ) ;
#24777 = CARTESIAN_POINT ( 'NONE',  ( 1.375225265779999928, -94.98812079580000045, 24.46248543800000164 ) ) ;
#24778 = ORIENTED_EDGE ( 'NONE', *, *, #5821, .F. ) ;
#24779 = AXIS2_PLACEMENT_3D ( 'NONE', #8595, #5612, #12014 ) ;
#24780 = CARTESIAN_POINT ( 'NONE',  ( 47.02585954350560371, -74.18642135858951292, -1.789303680145066355 ) ) ;
#24781 = ORIENTED_EDGE ( 'NONE', *, *, #8972, .T. ) ;
#24782 = CARTESIAN_POINT ( 'NONE',  ( -11.52020750800000037, -42.27108258110000349, 19.79605168710000029 ) ) ;
#24783 = DIRECTION ( 'NONE',  ( 0.000000000000000000, -1.000000000000000000, 0.000000000000000000 ) ) ;
#24784 = VERTEX_POINT ( 'NONE', #2360 ) ;
#24785 = CIRCLE ( 'NONE', #12636, 7.249999999999999112 ) ;
#24786 = CARTESIAN_POINT ( 'NONE',  ( 15.50925563669999896, -100.9197081840000010, 1.894558565230000102 ) ) ;
#24787 = ADVANCED_FACE ( 'NONE', ( #28699 ), #17656, .T. ) ;
#24788 = EDGE_CURVE ( 'NONE', #6516, #14582, #3446, .T. ) ;
#24789 = FACE_OUTER_BOUND ( 'NONE', #23714, .T. ) ;
#24790 = CARTESIAN_POINT ( 'NONE',  ( 8.797620038699999867, -37.04760834070000186, -21.76996719339999942 ) ) ;
#24791 = CARTESIAN_POINT ( 'NONE',  ( 0.000000000000000000, -108.5000000000000000, 0.000000000000000000 ) ) ;
#24792 = CARTESIAN_POINT ( 'NONE',  ( -10.39471473370000076, -19.47871561450000044, -20.73499808220000062 ) ) ;
#24793 = CARTESIAN_POINT ( 'NONE',  ( 22.90783306289999999, -66.63438074019998680, 12.00069599370000084 ) ) ;
#24794 = ORIENTED_EDGE ( 'NONE', *, *, #26724, .F. ) ;
#24795 = EDGE_CURVE ( 'NONE', #22, #21247, #24355, .T. ) ;
#24796 = DIRECTION ( 'NONE',  ( 0.000000000000000000, -1.000000000000000000, 0.000000000000000000 ) ) ;
#24797 = CARTESIAN_POINT ( 'NONE',  ( -38.22437212383332650, -65.70788121357088585, -1.362554289316070477 ) ) ;
#24798 = CARTESIAN_POINT ( 'NONE',  ( -32.17258283129999796, -74.02008960720000630, -21.87546129999999778 ) ) ;
#24799 = EDGE_LOOP ( 'NONE', ( #1553, #4370, #11071, #10718 ) ) ;
#24800 = CARTESIAN_POINT ( 'NONE',  ( 20.17385775081925914, -18.60284042207205601, -7.562753588496645918 ) ) ;
#24801 = CARTESIAN_POINT ( 'NONE',  ( 0.000000000000000000, -30.20000000000000284, 0.000000000000000000 ) ) ;
#24802 = CARTESIAN_POINT ( 'NONE',  ( -22.33897789299999914, -68.90459131420000460, 16.95310341020000067 ) ) ;
#24803 = EDGE_LOOP ( 'NONE', ( #20851, #16338, #10497 ) ) ;
#24804 = CARTESIAN_POINT ( 'NONE',  ( 37.17329344845187222, -80.00000002986575964, -13.70472019879660763 ) ) ;
#24805 = CIRCLE ( 'NONE', #22967, 0.9999999999999978906 ) ;
#24806 = CARTESIAN_POINT ( 'NONE',  ( -19.77751067240000182, -52.59522851920000619, 14.14810317800000128 ) ) ;
#24807 = DIRECTION ( 'NONE',  ( -0.9952295494196657932, 0.000000000000000000, -0.09756097560976527416 ) ) ;
#24808 = CARTESIAN_POINT ( 'NONE',  ( -0.6842253573819999657, -101.2530993000000024, -15.17849927279999989 ) ) ;
#24809 = CARTESIAN_POINT ( 'NONE',  ( -14.78607513363078318, -74.25103023226107268, 36.28681140252551529 ) ) ;
#24810 = EDGE_CURVE ( 'NONE', #22379, #9997, #22520, .T. ) ;
#24811 = DIRECTION ( 'NONE',  ( 0.000000000000000000, 1.000000000000000000, 0.000000000000000000 ) ) ;
#24812 = FACE_BOUND ( 'NONE', #747, .T. ) ;
#24813 = VERTEX_POINT ( 'NONE', #11054 ) ;
#24814 = CARTESIAN_POINT ( 'NONE',  ( -15.06840628259999981, -92.56711348129999806, 24.34572243330000063 ) ) ;
#24815 = AXIS2_PLACEMENT_3D ( 'NONE', #5168, #14050, #3000 ) ;
#24816 = CARTESIAN_POINT ( 'NONE',  ( 14.80687252510000107, -97.01506571140001256, 14.57555587629999927 ) ) ;
#24817 = ORIENTED_EDGE ( 'NONE', *, *, #19807, .F. ) ;
#24818 = CARTESIAN_POINT ( 'NONE',  ( 7.283536107469999799, -74.14144860030000928, 39.92836808239999868 ) ) ;
#24819 = CARTESIAN_POINT ( 'NONE',  ( 24.55398044940000446, -92.70565333729999224, 14.54119304790000022 ) ) ;
#24820 = CARTESIAN_POINT ( 'NONE',  ( 23.63066637245063362, -19.48669443993386352, 1.455896856190272537 ) ) ;
#24821 = CARTESIAN_POINT ( 'NONE',  ( 26.82037688552241406, -72.68639319731354931, -10.33655577607157561 ) ) ;
#24822 = CIRCLE ( 'NONE', #23427, 23.79684788999999867 ) ;
#24823 = CARTESIAN_POINT ( 'NONE',  ( 9.166432219540000759, -35.89879984470000096, -19.92145671899999826 ) ) ;
#24824 = AXIS2_PLACEMENT_3D ( 'NONE', #26833, #4671, #26979 ) ;
#24825 = CARTESIAN_POINT ( 'NONE',  ( 8.353998429006537663, -19.47332482891561511, -20.26327805068222432 ) ) ;
#24826 = CARTESIAN_POINT ( 'NONE',  ( 7.073120017670000870, -99.73367811500000357, 15.79835279589999963 ) ) ;
#24827 = CARTESIAN_POINT ( 'NONE',  ( 23.56413682950000066, -19.48537698630000037, 1.506493335489999863 ) ) ;
#24828 = CARTESIAN_POINT ( 'NONE',  ( -5.542684685070000228, -95.66919271819999437, -21.81728948419999981 ) ) ;
#24829 = CARTESIAN_POINT ( 'NONE',  ( 13.81100091409999919, -99.92967571559999840, -10.51865105429999936 ) ) ;
#24830 = CARTESIAN_POINT ( 'NONE',  ( 11.77817022719999862, -101.0685849509999912, -10.96540529560000010 ) ) ;
#24831 = DIRECTION ( 'NONE',  ( 0.000000000000000000, -1.000000000000000000, 0.000000000000000000 ) ) ;
#24832 = CARTESIAN_POINT ( 'NONE',  ( -3.883346862689999845, -16.50000000000000000, -7.108418751309999450 ) ) ;
#24833 = CARTESIAN_POINT ( 'NONE',  ( -32.83566817450000030, -79.25000000000000000, -22.22906645670000003 ) ) ;
#24834 = AXIS2_PLACEMENT_3D ( 'NONE', #4934, #1650, #10486 ) ;
#24835 = CARTESIAN_POINT ( 'NONE',  ( 25.93686798816709427, -62.33603094518826992, 1.426352254284204202 ) ) ;
#24836 = CARTESIAN_POINT ( 'NONE',  ( -38.24999999999320011, -65.14196057591033195, -2.700834934057557479 ) ) ;
#24837 = DIRECTION ( 'NONE',  ( 0.000000000000000000, 1.000000000000000000, 0.000000000000000000 ) ) ;
#24838 = CARTESIAN_POINT ( 'NONE',  ( -14.77445022520000073, -101.2530993010000060, 3.545507728379999612 ) ) ;
#24839 = EDGE_LOOP ( 'NONE', ( #7153, #13581, #8547, #9059 ) ) ;
#24840 = CARTESIAN_POINT ( 'NONE',  ( 36.61132492839999486, -74.71742460369999606, -14.71192759290000041 ) ) ;
#24841 = B_SPLINE_CURVE_WITH_KNOTS ( 'NONE', 3,
 ( #25855, #14758, #9715, #7410 ),
 .UNSPECIFIED., .F., .F.,
 ( 4, 4 ),
 ( -66.18347591719999912, -38.72099908220000231 ),
 .UNSPECIFIED. ) ;
#24842 = CARTESIAN_POINT ( 'NONE',  ( 7.844113379649998663, -101.1184174639999895, 13.21637662110000022 ) ) ;
#24843 = AXIS2_PLACEMENT_3D ( 'NONE', #17508, #26393, #15008 ) ;
#24844 = EDGE_CURVE ( 'NONE', #3611, #898, #19238, .T. ) ;
#24845 = DIRECTION ( 'NONE',  ( 0.000000000000000000, 1.000000000000000000, 0.000000000000000000 ) ) ;
#24846 = CARTESIAN_POINT ( 'NONE',  ( -13.69048216150000030, -61.75768530429999714, 21.15265907719999916 ) ) ;
#24847 = DIRECTION ( 'NONE',  ( 0.000000000000000000, 1.000000000000000000, 0.000000000000000000 ) ) ;
#24848 = EDGE_CURVE ( 'NONE', #19645, #8365, #1930, .T. ) ;
#24849 = DIRECTION ( 'NONE',  ( 1.000000000000000000, 0.000000000000000000, 0.000000000000000000 ) ) ;
#24850 = CARTESIAN_POINT ( 'NONE',  ( 20.59810119160000141, -36.00000000000000000, -9.165580181560001094 ) ) ;
#24851 = ADVANCED_FACE ( 'NONE', ( #10769 ), #26538, .T. ) ;
#24852 = CIRCLE ( 'NONE', #26726, 4.999999999999999112 ) ;
#24853 = CARTESIAN_POINT ( 'NONE',  ( -39.50000000000000000, -65.63577453799999262, -2.309401076760000393 ) ) ;
#24854 = ORIENTED_EDGE ( 'NONE', *, *, #6683, .F. ) ;
#24855 = CIRCLE ( 'NONE', #17859, 57.75000000000000000 ) ;
#24856 = CARTESIAN_POINT ( 'NONE',  ( 30.51083463210725810, -74.19211354766501643, -24.52263441801099475 ) ) ;
#24857 = CARTESIAN_POINT ( 'NONE',  ( -23.50863772330000145, -94.59276583650000703, -3.692488328609999648 ) ) ;
#24858 = ORIENTED_EDGE ( 'NONE', *, *, #13684, .F. ) ;
#24859 = CARTESIAN_POINT ( 'NONE',  ( -30.47693414353797792, -92.55017404142812154, 1.185968520876313326 ) ) ;
#24860 = EDGE_LOOP ( 'NONE', ( #6677, #2886, #26098 ) ) ;
#24861 = DIRECTION ( 'NONE',  ( 0.000000000000000000, 1.000000000000000000, 0.000000000000000000 ) ) ;
#24862 = DIRECTION ( 'NONE',  ( -0.8775825618903722036, 0.000000000000000000, 0.4794255386042041156 ) ) ;
#24863 = CARTESIAN_POINT ( 'NONE',  ( 15.74335372269999844, -101.1889999979999999, 2.854262350110000401 ) ) ;
#24864 = AXIS2_PLACEMENT_3D ( 'NONE', #11815, #15893, #16335 ) ;
#24865 = CARTESIAN_POINT ( 'NONE',  ( -7.241427273170902623, -74.22736093603683116, -40.35276762194584421 ) ) ;
#24866 = FACE_OUTER_BOUND ( 'NONE', #10577, .T. ) ;
#24867 = CARTESIAN_POINT ( 'NONE',  ( -21.51944571800000006, -66.74192463980000412, 15.33029011760000060 ) ) ;
#24868 = CARTESIAN_POINT ( 'NONE',  ( -17.53389815281536812, -96.07279461669297405, 13.09664283538910468 ) ) ;
#24869 = ORIENTED_EDGE ( 'NONE', *, *, #130, .F. ) ;
#24870 = FACE_OUTER_BOUND ( 'NONE', #12252, .T. ) ;
#24871 = DIRECTION ( 'NONE',  ( -0.006434372441722441445, 0.000000000000000000, 0.9999792992113792911 ) ) ;
#24872 = CARTESIAN_POINT ( 'NONE',  ( 38.71641004229999794, -73.50000000000000000, -7.135467526410000261 ) ) ;
#24873 = FACE_OUTER_BOUND ( 'NONE', #19352, .T. ) ;
#24874 = CARTESIAN_POINT ( 'NONE',  ( 23.26869159428434131, -63.26419843741122406, -7.439610865658912608 ) ) ;
#24875 = ORIENTED_EDGE ( 'NONE', *, *, #10084, .T. ) ;
#24876 = AXIS2_PLACEMENT_3D ( 'NONE', #12713, #25994, #21626 ) ;
#24877 = CARTESIAN_POINT ( 'NONE',  ( 26.33787588810572444, -92.82529299094895237, -15.38071215267214420 ) ) ;
#24878 = ORIENTED_EDGE ( 'NONE', *, *, #25773, .T. ) ;
#24879 = EDGE_CURVE ( 'NONE', #8141, #25766, #24208, .T. ) ;
#24880 = DIRECTION ( 'NONE',  ( 0.9295286103719511139, 0.000000000000000000, 0.3687499999999862554 ) ) ;
#24881 = EDGE_CURVE ( 'NONE', #20540, #10287, #17420, .T. ) ;
#24882 = CARTESIAN_POINT ( 'NONE',  ( 12.61209325099999923, -101.1889999979999999, -11.02259514940000074 ) ) ;
#24883 = AXIS2_PLACEMENT_3D ( 'NONE', #26583, #20167, #84 ) ;
#24884 = CARTESIAN_POINT ( 'NONE',  ( 5.611330023069999839, -93.37393516990000819, 26.68650669730000047 ) ) ;
#24885 = ADVANCED_FACE ( 'NONE', ( #26692 ), #11215, .T. ) ;
#24886 = EDGE_LOOP ( 'NONE', ( #17495, #25822, #18805, #28550 ) ) ;
#24887 = AXIS2_PLACEMENT_3D ( 'NONE', #27477, #25297, #981 ) ;
#24888 = ORIENTED_EDGE ( 'NONE', *, *, #18836, .T. ) ;
#24889 = DIRECTION ( 'NONE',  ( 1.000000000000000000, 0.000000000000000000, 0.000000000000000000 ) ) ;
#24890 = CARTESIAN_POINT ( 'NONE',  ( 23.03829042120000281, -19.50000000000000000, 10.32398954119999956 ) ) ;
#24891 = CARTESIAN_POINT ( 'NONE',  ( 47.16762201259999898, -74.53410573390000593, -1.089910948100000221 ) ) ;
#24892 = ORIENTED_EDGE ( 'NONE', *, *, #287, .F. ) ;
#24893 = CARTESIAN_POINT ( 'NONE',  ( 7.135467304789999687, -73.50000064450000536, -38.71640881029999548 ) ) ;
#24894 = FACE_OUTER_BOUND ( 'NONE', #2736, .T. ) ;
#24895 = CARTESIAN_POINT ( 'NONE',  ( 7.236990221556244940, -101.1962284174823594, 13.44316210220003249 ) ) ;
#24896 = VECTOR ( 'NONE', #22176, 1000.000000000000000 ) ;
#24897 = B_SPLINE_CURVE_WITH_KNOTS ( 'NONE', 3,
 ( #4099, #12968, #2665, #20732, #24804, #18091 ),
 .UNSPECIFIED., .F., .F.,
 ( 4, 2, 4 ),
 ( 0.000000000000000000, 0.5000000000000000000, 1.000000000000000000 ),
 .UNSPECIFIED. ) ;
#24898 = CARTESIAN_POINT ( 'NONE',  ( 12.37352278080000012, -101.4254868729999970, -10.09472709699999982 ) ) ;
#24899 = CARTESIAN_POINT ( 'NONE',  ( -18.05096283909999855, -93.00000167610001256, -23.30076369320000040 ) ) ;
#24900 = CARTESIAN_POINT ( 'NONE',  ( 5.273680924649999824, -107.3487944130000074, 9.653408180790000515 ) ) ;
#24901 = ORIENTED_EDGE ( 'NONE', *, *, #10114, .F. ) ;
#24902 = CARTESIAN_POINT ( 'NONE',  ( 36.74383121569999844, -74.66666670279998641, -14.69280906399999864 ) ) ;
#24903 = CARTESIAN_POINT ( 'NONE',  ( -16.86763901309999980, -99.92604429489999518, 3.250425998059999877 ) ) ;
#24904 = DIRECTION ( 'NONE',  ( 1.000000000000000000, 0.000000000000000000, 0.000000000000000000 ) ) ;
#24905 = CARTESIAN_POINT ( 'NONE',  ( -21.99985828019999801, -74.00000000000000000, -31.89935321680000158 ) ) ;
#24906 = ORIENTED_EDGE ( 'NONE', *, *, #22100, .T. ) ;
#24907 = DIRECTION ( 'NONE',  ( 1.000000000000000000, 0.000000000000000000, 0.000000000000000000 ) ) ;
#24908 = CARTESIAN_POINT ( 'NONE',  ( -7.511960512013370561, -73.99984148058264566, 38.89461421659916596 ) ) ;
#24909 = LINE ( 'NONE', #13524, #1065 ) ;
#24910 = ORIENTED_EDGE ( 'NONE', *, *, #21169, .F. ) ;
#24911 = CARTESIAN_POINT ( 'NONE',  ( -13.12430011460000046, -92.94829811809999853, -23.71756069369999764 ) ) ;
#24912 = VECTOR ( 'NONE', #19353, 999.9999999999998863 ) ;
#24913 = CARTESIAN_POINT ( 'NONE',  ( 22.62080797870000382, -64.93834956060000252, 11.20705156650000056 ) ) ;
#24914 = CARTESIAN_POINT ( 'NONE',  ( 8.489272773159999730, -34.76176403470000054, -20.80005463859999892 ) ) ;
#24915 = CARTESIAN_POINT ( 'NONE',  ( 16.04726154520435699, -100.8738282915798123, 4.264385135213858646 ) ) ;
#24916 = ADVANCED_FACE ( 'NONE', ( #26108 ), #12820, .F. ) ;
#24917 = CARTESIAN_POINT ( 'NONE',  ( -29.16815472389999897, -74.00000000000000000, -29.16815472389999897 ) ) ;
#24918 = ORIENTED_EDGE ( 'NONE', *, *, #17270, .T. ) ;
#24919 = CARTESIAN_POINT ( 'NONE',  ( 47.25093520489999577, -79.38329488089999586, -0.8867236800390000395 ) ) ;
#24920 = CARTESIAN_POINT ( 'NONE',  ( 6.114061450890000415, -101.1889999979999999, -13.40104985119999981 ) ) ;
#24921 = ADVANCED_FACE ( 'NONE', ( #4837 ), #15987, .T. ) ;
#24922 = CARTESIAN_POINT ( 'NONE',  ( -12.27127883659999874, -64.93834664010000779, -22.06162167850000344 ) ) ;
#24923 = CARTESIAN_POINT ( 'NONE',  ( 23.93802380909999883, -64.72767011149998950, -9.438994838039999280 ) ) ;
#24924 = DIRECTION ( 'NONE',  ( 0.000000000000000000, 1.000000000000000000, 0.000000000000000000 ) ) ;
#24925 = EDGE_CURVE ( 'NONE', #21477, #4628, #28544, .T. ) ;
#24926 = VERTEX_POINT ( 'NONE', #2660 ) ;
#24927 = CARTESIAN_POINT ( 'NONE',  ( -29.17304402409999753, -40.00000000000000000, -53.40089889099999709 ) ) ;
#24928 = CARTESIAN_POINT ( 'NONE',  ( 40.00000000000000000, -73.00000000000000000, 2.433892081919999696E-15 ) ) ;
#24929 = EDGE_LOOP ( 'NONE', ( #18223, #26550, #20107, #10510 ) ) ;
#24930 = CARTESIAN_POINT ( 'NONE',  ( 21.50956136780000350, -52.61368720150000655, 10.11639787100000021 ) ) ;
#24931 = ORIENTED_EDGE ( 'NONE', *, *, #22043, .F. ) ;
#24932 = DIRECTION ( 'NONE',  ( 0.000000000000000000, 1.000000000000000000, 0.000000000000000000 ) ) ;
#24933 = CARTESIAN_POINT ( 'NONE',  ( 13.81100091409999919, -111.0000000000000000, -10.51865105429999936 ) ) ;
#24934 = CARTESIAN_POINT ( 'NONE',  ( -28.75282704045790538, -92.49999918155121748, -2.687052330903884290 ) ) ;
#24935 = DIRECTION ( 'NONE',  ( 0.000000000000000000, 1.000000000000000000, 0.000000000000000000 ) ) ;
#24936 = CARTESIAN_POINT ( 'NONE',  ( -19.51771074589999699, -96.73994798520000415, 8.394649969090000496 ) ) ;
#24937 = CARTESIAN_POINT ( 'NONE',  ( -10.33087021410000084, -18.62222165789999906, -21.72933387530000005 ) ) ;
#24938 = CARTESIAN_POINT ( 'NONE',  ( 21.62393716137362176, -37.83478482166370327, -8.109578283838366985 ) ) ;
#24939 = ORIENTED_EDGE ( 'NONE', *, *, #16186, .T. ) ;
#24940 = CARTESIAN_POINT ( 'NONE',  ( 12.83908560070000071, -94.89197151660000884, -19.89638108760000179 ) ) ;
#24941 = CARTESIAN_POINT ( 'NONE',  ( -37.96285680772825089, -65.71745250376275749, -0.8863062584507671593 ) ) ;
#24942 = CARTESIAN_POINT ( 'NONE',  ( -13.11938740068049825, -92.71619979444491833, 27.53419132531503166 ) ) ;
#24943 = ORIENTED_EDGE ( 'NONE', *, *, #26296, .T. ) ;
#24944 = CARTESIAN_POINT ( 'NONE',  ( -11.98370860700000051, -101.2530993010000060, -9.340542411159999503 ) ) ;
#24945 = DIRECTION ( 'NONE',  ( 1.000000000000000000, 0.000000000000000000, 0.000000000000000000 ) ) ;
#24946 = CARTESIAN_POINT ( 'NONE',  ( 7.727581852389999284, -65.07443093669999712, -23.93312597839999967 ) ) ;
#24947 = ORIENTED_EDGE ( 'NONE', *, *, #1256, .T. ) ;
#24948 = CARTESIAN_POINT ( 'NONE',  ( -17.58843202809999795, -98.51728656799998873, 8.830207771419999574 ) ) ;
#24949 = CARTESIAN_POINT ( 'NONE',  ( 0.6893497139830000453, -99.55609327400000552, -17.37226014440000199 ) ) ;
#24950 = DIRECTION ( 'NONE',  ( -0.8775825618903722036, 0.000000000000000000, 0.4794255386042041156 ) ) ;
#24951 = CARTESIAN_POINT ( 'NONE',  ( -31.00000000000000000, -13.00000000000000000, 4.500000000000000000 ) ) ;
#24952 = CARTESIAN_POINT ( 'NONE',  ( -14.57086084372058998, -74.12888392171852558, 36.26832171247329484 ) ) ;
#24953 = EDGE_CURVE ( 'NONE', #25027, #12424, #489, .T. ) ;
#24954 = CARTESIAN_POINT ( 'NONE',  ( 25.44280605499999837, -65.72122283910000817, -0.3044463870030000296 ) ) ;
#24955 = B_SPLINE_CURVE_WITH_KNOTS ( 'NONE', 5,
 ( #6608, #18117, #13142, #220, #7051, #24672 ),
 .UNSPECIFIED., .F., .F.,
 ( 6, 6 ),
 ( 0.000000000000000000, 1.000000000000000000 ),
 .UNSPECIFIED. ) ;
#24956 = EDGE_LOOP ( 'NONE', ( #22676, #12237, #751, #5948, #19403, #7462 ) ) ;
#24957 = DIRECTION ( 'NONE',  ( 0.000000000000000000, 1.000000000000000000, 0.000000000000000000 ) ) ;
#24958 = DIRECTION ( 'NONE',  ( 1.000000000000000000, 0.000000000000000000, 0.000000000000000000 ) ) ;
#24959 = ORIENTED_EDGE ( 'NONE', *, *, #11749, .T. ) ;
#24960 = CIRCLE ( 'NONE', #2637, 16.00000000000000000 ) ;
#24961 = CARTESIAN_POINT ( 'NONE',  ( 23.54413596224770799, -92.59055325462402664, -19.38875311991260730 ) ) ;
#24962 = CARTESIAN_POINT ( 'NONE',  ( 0.000000000000000000, -10.08849557519999962, 0.000000000000000000 ) ) ;
#24963 = CARTESIAN_POINT ( 'NONE',  ( 22.15930751770139295, -19.46518600424841239, 0.2066986137561050429 ) ) ;
#24964 = CARTESIAN_POINT ( 'NONE',  ( 6.153538926910000484, -92.84292488370000740, 28.82528031139999669 ) ) ;
#24965 = DIRECTION ( 'NONE',  ( -1.000000000000000000, 0.000000000000000000, 0.000000000000000000 ) ) ;
#24966 = CARTESIAN_POINT ( 'NONE',  ( 8.694112515909999672, -36.31461050599999396, -21.07880576559999852 ) ) ;
#24967 = CARTESIAN_POINT ( 'NONE',  ( -37.10038231309999901, -65.31510159580000163, -0.3466308900760000089 ) ) ;
#24968 = ORIENTED_EDGE ( 'NONE', *, *, #24180, .F. ) ;
#24969 = CARTESIAN_POINT ( 'NONE',  ( 8.932460458690000493, -98.93374375299998746, 16.36585915649999734 ) ) ;
#24970 = ADVANCED_FACE ( 'NONE', ( #17947 ), #7026, .T. ) ;
#24971 = CARTESIAN_POINT ( 'NONE',  ( 23.40442542150000094, -18.50000000000000000, 2.199655364299999860 ) ) ;
#24972 = CARTESIAN_POINT ( 'NONE',  ( 0.000000000000000000, 0.000000000000000000, 0.000000000000000000 ) ) ;
#24973 = DIRECTION ( 'NONE',  ( 0.7071067811865475727, 0.000000000000000000, 0.7071067811865475727 ) ) ;
#24974 = CARTESIAN_POINT ( 'NONE',  ( -15.43525461730000004, -101.1461875130000010, 4.782897338129999731 ) ) ;
#24975 = CARTESIAN_POINT ( 'NONE',  ( -1.468618107569999998, -45.99312545570000310, -23.12288400899999985 ) ) ;
#24976 = CARTESIAN_POINT ( 'NONE',  ( 14.57207603078257030, -95.48799328830101274, 17.32764375622651798 ) ) ;
#24977 = DIRECTION ( 'NONE',  ( 0.000000000000000000, 1.000000000000000000, 0.000000000000000000 ) ) ;
#24978 = CARTESIAN_POINT ( 'NONE',  ( -41.00000000000000000, -84.50000000000000000, 10.20110288159999890 ) ) ;
#24979 = CARTESIAN_POINT ( 'NONE',  ( 21.89436955060000045, -49.11506481569999494, -7.274533568899999914 ) ) ;
#24980 = FACE_OUTER_BOUND ( 'NONE', #9129, .T. ) ;
#24981 = CARTESIAN_POINT ( 'NONE',  ( 0.000000000000000000, -108.5000000000000000, 0.000000000000000000 ) ) ;
#24982 = VERTEX_POINT ( 'NONE', #9334 ) ;
#24983 = CARTESIAN_POINT ( 'NONE',  ( -29.76015270875833707, -92.93978723898862881, 6.677089761457638772 ) ) ;
#24984 = ADVANCED_FACE ( 'NONE', ( #22617 ), #5775, .T. ) ;
#24985 = CARTESIAN_POINT ( 'NONE',  ( 7.021283738330000190, -101.6484611540000031, 14.37740230390000029 ) ) ;
#24986 = DIRECTION ( 'NONE',  ( 0.4794255386042036715, 0.000000000000000000, 0.8775825618903724257 ) ) ;
#24987 = CARTESIAN_POINT ( 'NONE',  ( 23.58655624800000083, -94.70873613630000420, -2.249367945439999961 ) ) ;
#24988 = CARTESIAN_POINT ( 'NONE',  ( 19.45347853379999847, -35.02802294540000361, -8.988163599090000844 ) ) ;
#24989 = CARTESIAN_POINT ( 'NONE',  ( -18.69985100839999959, -93.00000000000000000, 22.78328762010000119 ) ) ;
#24990 = EDGE_CURVE ( 'NONE', #26269, #26341, #22072, .T. ) ;
#24991 = DIRECTION ( 'NONE',  ( 0.2414462220490755373, 0.000000000000000000, -0.9704142011833033488 ) ) ;
#24992 = CARTESIAN_POINT ( 'NONE',  ( 40.00000000000000000, -73.50000000000000000, -9.769962616700000205E-15 ) ) ;
#24993 = CARTESIAN_POINT ( 'NONE',  ( -19.98978262542267359, -95.81137667811660208, 9.708844812268232261 ) ) ;
#24994 = CARTESIAN_POINT ( 'NONE',  ( 16.23185304080000080, -99.92384627689999377, 4.745118442920000845 ) ) ;
#24995 = VERTEX_POINT ( 'NONE', #18390 ) ;
#24996 = CARTESIAN_POINT ( 'NONE',  ( 30.67010299991955691, -74.17477598292983032, -24.29988026823843583 ) ) ;
#24997 = CARTESIAN_POINT ( 'NONE',  ( -17.68956059909999823, -98.30614355279999472, -8.105910472710000647 ) ) ;
#24998 = ORIENTED_EDGE ( 'NONE', *, *, #23143, .F. ) ;
#24999 = CARTESIAN_POINT ( 'NONE',  ( -12.89904789370000060, -65.07443093669999712, -21.58991903219999742 ) ) ;
#25000 = DIRECTION ( 'NONE',  ( 0.000000000000000000, 1.000000000000000000, 0.000000000000000000 ) ) ;
#25001 = EDGE_CURVE ( 'NONE', #452, #16695, #26450, .T. ) ;
#25002 = CARTESIAN_POINT ( 'NONE',  ( -3.108624468950000298E-16, -74.00000000000000000, -1.554312234480000048E-16 ) ) ;
#25003 = CARTESIAN_POINT ( 'NONE',  ( -16.49390888960000368, -79.50000000000000000, 44.28897684009999836 ) ) ;
#25004 = CARTESIAN_POINT ( 'NONE',  ( 19.97576656849999921, -38.00000000000000000, -19.97576656849999921 ) ) ;
#25005 = CARTESIAN_POINT ( 'NONE',  ( 23.06813085299999955, -94.22763312370000222, -7.559806761219999949 ) ) ;
#25006 = CARTESIAN_POINT ( 'NONE',  ( -14.24982662769999919, -74.06193868690000670, 36.58417219249999874 ) ) ;
#25007 = CARTESIAN_POINT ( 'NONE',  ( 4.500000000000000000, 0.000000000000000000, 50.00000000000000000 ) ) ;
#25008 = CARTESIAN_POINT ( 'NONE',  ( -16.27155717411393354, -99.02168173220448466, 7.873387082247683466 ) ) ;
#25009 = B_SPLINE_SURFACE_WITH_KNOTS ( 'NONE', 5, 5, ( 
 ( #19636, #28526, #17171, #19922, #19362, #8562, #13416, #24307, #28235 ),
 ( #26060, #6088, #12779, #23877, #12915, #3914, #4195, #6378, #22129 ),
 ( #21828, #4348, #24161, #6238, #19494, #2028, #15103, #17464, #10868 ),
 ( #19778, #28381, #17757, #26350, #8411, #17317, #13363, #1885, #26212 ),
 ( #15394, #24015, #2170, #10722, #28659, #8691, #8844, #26641, #6685 ),
 ( #15549, #1605, #9839, #439, #22266, #16684, #13513, #2614, #26939 ),
 ( #9976, #24600, #13668, #11167, #20081, #18191, #22422, #18891, #27773 ),
 ( #23259, #5476, #298, #7810, #145, #16551, #8995, #11464, #2468 ),
 ( #20370, #9287, #18749, #3302, #9139, #25589, #13810, #27084, #17903 ) ),
 .UNSPECIFIED., .F., .F., .F.,
 ( 6, 3, 6 ),
 ( 6, 3, 6 ),
 ( 7.186332008850000008, 18.82032538960000068, 25.08217527079999698 ),
 ( 0.000000000000000000, 0.2500000000000000000, 0.5000000000000000000 ),
 .UNSPECIFIED. ) ;
#25010 = ORIENTED_EDGE ( 'NONE', *, *, #20939, .T. ) ;
#25011 = CARTESIAN_POINT ( 'NONE',  ( -11.78426840870000092, -72.00000269519999563, -26.58403829429999732 ) ) ;
#25012 = LINE ( 'NONE', #9848, #24676 ) ;
#25013 = CARTESIAN_POINT ( 'NONE',  ( -9.356041104380000917, -84.50000000000000000, 37.60355029590000697 ) ) ;
#25014 = EDGE_CURVE ( 'NONE', #790, #4023, #23664, .T. ) ;
#25015 = CARTESIAN_POINT ( 'NONE',  ( 2.876553231629999985, -91.50000000000000000, 5.265495371340000119 ) ) ;
#25016 = DIRECTION ( 'NONE',  ( 1.000000000000000000, 0.000000000000000000, 0.000000000000000000 ) ) ;
#25017 = ORIENTED_EDGE ( 'NONE', *, *, #862, .F. ) ;
#25018 = AXIS2_PLACEMENT_3D ( 'NONE', #12993, #23663, #6017 ) ;
#25019 = CARTESIAN_POINT ( 'NONE',  ( 26.35926584486895408, -92.81370807106951304, -15.34403634914452397 ) ) ;
#25020 = ORIENTED_EDGE ( 'NONE', *, *, #7942, .T. ) ;
#25021 = AXIS2_PLACEMENT_3D ( 'NONE', #23747, #21564, #25665 ) ;
#25022 = CARTESIAN_POINT ( 'NONE',  ( -2.583989732180000498, -57.40875670289999988, -25.23271578160000317 ) ) ;
#25023 = VECTOR ( 'NONE', #18831, 1000.000000000000000 ) ;
#25024 = CARTESIAN_POINT ( 'NONE',  ( 1.316303147800000017, -94.80026829419999501, 24.39090705379999946 ) ) ;
#25025 = CARTESIAN_POINT ( 'NONE',  ( 5.717411334609999507, -92.96448467939998750, 26.13902206350000057 ) ) ;
#25026 = ORIENTED_EDGE ( 'NONE', *, *, #3753, .T. ) ;
#25027 = VERTEX_POINT ( 'NONE', #20419 ) ;
#25028 = DIRECTION ( 'NONE',  ( 0.000000000000000000, -1.000000000000000000, 0.000000000000000000 ) ) ;
#25029 = CARTESIAN_POINT ( 'NONE',  ( 21.76996726540000182, -37.04760833810000520, -8.797620137550000052 ) ) ;
#25030 = CARTESIAN_POINT ( 'NONE',  ( 46.91509368659999524, -74.22322967379999170, -2.558872053950000058 ) ) ;
#25031 = ORIENTED_EDGE ( 'NONE', *, *, #18225, .T. ) ;
#25032 = CARTESIAN_POINT ( 'NONE',  ( -26.77683864449999973, -30.20000000000000284, -49.01467436490000296 ) ) ;
#25033 = CARTESIAN_POINT ( 'NONE',  ( -11.55286930265329559, -62.03412635121320307, 21.09176644221611241 ) ) ;
#25034 = ORIENTED_EDGE ( 'NONE', *, *, #26610, .F. ) ;
#25035 = CIRCLE ( 'NONE', #3625, 0.9999999999999996669 ) ;
#25036 = CARTESIAN_POINT ( 'NONE',  ( 23.02872706138604997, -64.78279487706441842, 10.89319034239515105 ) ) ;
#25037 = DIRECTION ( 'NONE',  ( 0.000000000000000000, 1.000000000000000000, 0.000000000000000000 ) ) ;
#25038 = CARTESIAN_POINT ( 'NONE',  ( -2.037850653060000017, -66.42763100729999337, -25.87181958200000054 ) ) ;
#25039 = EDGE_CURVE ( 'NONE', #26675, #14431, #9182, .T. ) ;
#25040 = CARTESIAN_POINT ( 'NONE',  ( -16.56294617020000004, -72.37489744399999836, 23.47174545849999916 ) ) ;
#25041 = EDGE_LOOP ( 'NONE', ( #26521, #26171, #11370, #15456 ) ) ;
#25042 = ADVANCED_FACE ( 'NONE', ( #5273 ), #19255, .F. ) ;
#25043 = FACE_OUTER_BOUND ( 'NONE', #14777, .T. ) ;
#25044 = CARTESIAN_POINT ( 'NONE',  ( -2.584575094900000369, -57.80430444439999604, -25.24242493270000054 ) ) ;
#25045 = CARTESIAN_POINT ( 'NONE',  ( 25.53682860819999689, -63.14742133130000923, 1.286276417849999909 ) ) ;
#25046 = CARTESIAN_POINT ( 'NONE',  ( -21.71458329359999695, -74.41849501830000690, -32.69645379630000548 ) ) ;
#25047 = ORIENTED_EDGE ( 'NONE', *, *, #12350, .F. ) ;
#25048 = AXIS2_PLACEMENT_3D ( 'NONE', #3380, #18960, #27843 ) ;
#25049 = CARTESIAN_POINT ( 'NONE',  ( 0.000000000000000000, -94.59276292389999696, 0.000000000000000000 ) ) ;
#25050 = EDGE_CURVE ( 'NONE', #21458, #16504, #12286, .T. ) ;
#25051 = CARTESIAN_POINT ( 'NONE',  ( -0.02543935853460000188, -101.2530993010000060, -15.19457030269999898 ) ) ;
#25052 = CARTESIAN_POINT ( 'NONE',  ( 36.66944334404606565, -74.23450616714526973, -14.39398667539986576 ) ) ;
#25054 = ORIENTED_EDGE ( 'NONE', *, *, #502, .F. ) ;
#25053 = B_SPLINE_CURVE_WITH_KNOTS ( 'NONE', 3,
 ( #13398, #2649, #22458, #22303, #13848, #4827, #24640, #2349, #11500, #11202, #18379, #20113, #2501, #181, #9029, #26678, #7013, #17936, #26830, #19957, #6863, #15727, #4669, #13549, #328, #15880, #22606, #20259, #11355, #13704, #20408, #9322, #18226, #27123, #13997, #7163, #16171 ),
 .UNSPECIFIED., .F., .F.,
 ( 4, 2, 2, 1, 1, 1, 2, 2, 2, 2, 1, 1, 1, 2, 2, 2, 2, 1, 1, 1, 2, 2, 4 ),
 ( 0.000000000000000000, 0.1249999999999811817, 0.1874999999999717726, 0.2187499999999666933, 0.2343749999999644451, 0.2421874999999634459, 0.2460937499999632794, 0.2499999999999630851, 0.3749999999999583111, 0.4374999999999563127, 0.4687499999999551470, 0.4843749999999545364, 0.4921874999999544809, 0.4960937499999547029, 0.4999999999999548139, 0.6249999999999622524, 0.6874999999999660272, 0.7187499999999676925, 0.7343749999999685807, 0.7421874999999692468, 0.7460937499999694689, 0.7499999999999698019, 1.000000000000000000 ),
 .UNSPECIFIED. ) ;
#25055 = EDGE_CURVE ( 'NONE', #22026, #12661, #3461, .T. ) ;
#25056 = CARTESIAN_POINT ( 'NONE',  ( -11.86917066319999847, -93.06764199929999393, -23.73933353450000183 ) ) ;
#25057 = CARTESIAN_POINT ( 'NONE',  ( 23.98990767259999757, -64.35840732030000311, 10.71073183010000029 ) ) ;
#25058 = CARTESIAN_POINT ( 'NONE',  ( 7.215414233289999757, -77.00000000000000000, 40.70731707320000226 ) ) ;
#25059 = CARTESIAN_POINT ( 'NONE',  ( 15.63748056140000209, -101.6484611540000031, 3.386620984279999913 ) ) ;
#25060 = DIRECTION ( 'NONE',  ( 0.000000000000000000, 1.000000000000000000, 0.000000000000000000 ) ) ;
#25061 = VERTEX_POINT ( 'NONE', #24944 ) ;
#25062 = CARTESIAN_POINT ( 'NONE',  ( 22.76317971519999972, -52.57401960330000179, 10.17780311019999928 ) ) ;
#25063 = CARTESIAN_POINT ( 'NONE',  ( 16.42966103859999905, -94.59276292389999696, 17.21499949629999904 ) ) ;
#25064 = AXIS2_PLACEMENT_3D ( 'NONE', #19192, #1441, #8117 ) ;
#25065 = ITEM_DEFINED_TRANSFORMATION ( 'NONE', 'NONE', #12912,  #26433 ) ;
#25066 = CARTESIAN_POINT ( 'NONE',  ( -11.35317482230000152, -18.50000000000000000, 18.33892987359999793 ) ) ;
#25067 = CARTESIAN_POINT ( 'NONE',  ( -12.47307779800000027, -62.13475808420000135, -20.48183934720000110 ) ) ;
#25068 = CARTESIAN_POINT ( 'NONE',  ( 25.71399229409999876, -69.35813701630000594, -10.31084904409999936 ) ) ;
#25069 = CARTESIAN_POINT ( 'NONE',  ( 6.602264112093322090, -93.38552847742499807, 26.87384619217190007 ) ) ;
#25070 = ORIENTED_EDGE ( 'NONE', *, *, #23500, .F. ) ;
#25071 = CARTESIAN_POINT ( 'NONE',  ( -41.75000000000000000, -65.14977478849999670, -2.684678751739999925 ) ) ;
#25072 = ORIENTED_EDGE ( 'NONE', *, *, #10462, .F. ) ;
#25073 = B_SPLINE_CURVE_WITH_KNOTS ( 'NONE', 5,
 ( #28380, #16899, #24014, #21548, #28525, #1604 ),
 .UNSPECIFIED., .F., .F.,
 ( 6, 6 ),
 ( 0.000000000000000000, 1.000000000000000000 ),
 .UNSPECIFIED. ) ;
#25074 = AXIS2_PLACEMENT_3D ( 'NONE', #9156, #166, #15261 ) ;
#25075 = CARTESIAN_POINT ( 'NONE',  ( -11.68189216550000076, -27.06313277699999986, 19.27199430059999941 ) ) ;
#25076 = DIRECTION ( 'NONE',  ( 0.000000000000000000, 1.000000000000000000, 0.000000000000000000 ) ) ;
#25077 = ORIENTED_EDGE ( 'NONE', *, *, #20355, .T. ) ;
#25078 = CARTESIAN_POINT ( 'NONE',  ( 9.356041104380000917, -84.50000000000000000, 37.60355029590000697 ) ) ;
#25079 = CARTESIAN_POINT ( 'NONE',  ( 21.25272724153304438, -34.80518677145862227, -7.596422886174947209 ) ) ;
#25080 = CARTESIAN_POINT ( 'NONE',  ( -0.5335602090290000321, -52.63293862049999916, -23.18581005440000098 ) ) ;
#25081 = CARTESIAN_POINT ( 'NONE',  ( -10.87809348075558624, -19.46531138871780442, -19.32212505103515099 ) ) ;
#25082 = CARTESIAN_POINT ( 'NONE',  ( 22.78264860270000014, -94.59276292389999696, -6.873201011689999085 ) ) ;
#25083 = CARTESIAN_POINT ( 'NONE',  ( -41.14961768690000099, -65.31510159580000163, -2.684458023169999930 ) ) ;
#25084 = CARTESIAN_POINT ( 'NONE',  ( 46.70429134840502172, -79.89085532618133811, -3.466657557652187194 ) ) ;
#25085 = ORIENTED_EDGE ( 'NONE', *, *, #26924, .F. ) ;
#25086 = ADVANCED_FACE ( 'NONE', ( #11660 ), #6873, .T. ) ;
#25087 = VECTOR ( 'NONE', #4611, 1000.000000000000000 ) ;
#25088 = CARTESIAN_POINT ( 'NONE',  ( -32.51122442309999627, -80.25114697639999406, -21.99314580829999954 ) ) ;
#25089 = AXIS2_PLACEMENT_3D ( 'NONE', #18850, #18559, #16645 ) ;
#25090 = DIRECTION ( 'NONE',  ( 0.000000000000000000, 1.000000000000000000, 0.000000000000000000 ) ) ;
#25091 = ORIENTED_EDGE ( 'NONE', *, *, #24688, .T. ) ;
#25092 = DIRECTION ( 'NONE',  ( 0.000000000000000000, 1.000000000000000000, 0.000000000000000000 ) ) ;
#25093 = CARTESIAN_POINT ( 'NONE',  ( -29.41275679339999982, -10.50000000000000000, -53.83969017199999740 ) ) ;
#25094 = CARTESIAN_POINT ( 'NONE',  ( -14.65665288169999947, -79.50000000000000000, 36.94583914790000279 ) ) ;
#25095 = ORIENTED_EDGE ( 'NONE', *, *, #22410, .F. ) ;
#25096 = EDGE_CURVE ( 'NONE', #25651, #22535, #8716, .T. ) ;
#25097 = CARTESIAN_POINT ( 'NONE',  ( 9.348798002780000616, -17.50000000000000000, 17.11285995690000306 ) ) ;
#25098 = CARTESIAN_POINT ( 'NONE',  ( -20.04612630950000352, -45.94038128989999592, 14.54360384760000180 ) ) ;
#25099 = CARTESIAN_POINT ( 'NONE',  ( -24.16979293970000242, -74.00000000000000000, -34.06928787630000244 ) ) ;
#25100 = DIRECTION ( 'NONE',  ( 5.551115123129999410E-17, 0.000000000000000000, -1.000000000000000000 ) ) ;
#25101 = CARTESIAN_POINT ( 'NONE',  ( 23.23323687250000091, -61.84404940159999597, -9.246319667559999900 ) ) ;
#25102 = CARTESIAN_POINT ( 'NONE',  ( 25.99978933049999696, -66.93519943790001037, 0.3672536007030000049 ) ) ;
#25104 = AXIS2_PLACEMENT_3D ( 'NONE', #20363, #14248, #18773 ) ;
#25103 = B_SPLINE_CURVE_WITH_KNOTS ( 'NONE', 3,
 ( #16845, #25735, #5765, #19170 ),
 .UNSPECIFIED., .F., .F.,
 ( 4, 4 ),
 ( 0.000000000000000000, 1.000000000000000000 ),
 .UNSPECIFIED. ) ;
#25105 = CARTESIAN_POINT ( 'NONE',  ( 41.00000000000000000, -84.00000000000000000, 10.20110288159999890 ) ) ;
#25106 = CIRCLE ( 'NONE', #1819, 57.75000000000000000 ) ;
#25107 = AXIS2_PLACEMENT_3D ( 'NONE', #6127, #26252, #8047 ) ;
#25108 = ORIENTED_EDGE ( 'NONE', *, *, #11452, .T. ) ;
#25109 = DIRECTION ( 'NONE',  ( 0.000000000000000000, 1.000000000000000000, 0.000000000000000000 ) ) ;
#25110 = AXIS2_PLACEMENT_3D ( 'NONE', #8310, #24205, #4391 ) ;
#25111 = CARTESIAN_POINT ( 'NONE',  ( 20.64246525220000095, -36.08173683109999530, -8.980509983870000212 ) ) ;
#25112 = CARTESIAN_POINT ( 'NONE',  ( 8.097645732220000170, -101.1461871030000168, 13.98396704560000003 ) ) ;
#25113 = ORIENTED_EDGE ( 'NONE', *, *, #28215, .F. ) ;
#25114 = CARTESIAN_POINT ( 'NONE',  ( 7.255215663259999559, -74.34471143260000758, 40.30304758909999663 ) ) ;
#25115 = CARTESIAN_POINT ( 'NONE',  ( 15.63748056140000209, -101.6484611540000031, 3.386620984279999913 ) ) ;
#25116 = CARTESIAN_POINT ( 'NONE',  ( 0.000000000000000000, -15.80000000000000071, 0.000000000000000000 ) ) ;
#25117 = SURFACE_STYLE_FILL_AREA ( #5298 ) ;
#25118 = CARTESIAN_POINT ( 'NONE',  ( -10.83727467601077699, -93.79427251235401286, -23.30769844343626218 ) ) ;
#25119 = CARTESIAN_POINT ( 'NONE',  ( 7.960428606499999837, -37.73115151110000198, -21.57372765530000081 ) ) ;
#25120 = CARTESIAN_POINT ( 'NONE',  ( 7.625237055219999505, -101.6466297510000061, 14.06768965610000066 ) ) ;
#25121 = EDGE_LOOP ( 'NONE', ( #27060, #26840, #26684, #26773 ) ) ;
#25122 = EDGE_CURVE ( 'NONE', #5884, #15706, #9017, .T. ) ;
#25123 = DIRECTION ( 'NONE',  ( 0.000000000000000000, 1.000000000000000000, 0.000000000000000000 ) ) ;
#25124 = CARTESIAN_POINT ( 'NONE',  ( -4.439198032609999743E-16, -74.50000000000000000, 47.25000000000000000 ) ) ;
#25125 = CARTESIAN_POINT ( 'NONE',  ( 11.40864485750000057, -99.60591459030000294, -13.10462926860000010 ) ) ;
#25126 = ORIENTED_EDGE ( 'NONE', *, *, #20155, .T. ) ;
#25127 = TOROIDAL_SURFACE ( 'NONE', #1394, 60.85000000000000142, 0.5000000000000000000 ) ;
#25128 = CARTESIAN_POINT ( 'NONE',  ( 0.000000000000000000, -18.50000000000000000, 0.000000000000000000 ) ) ;
#25129 = DIRECTION ( 'NONE',  ( 1.000000000000000000, 0.000000000000000000, 0.000000000000000000 ) ) ;
#25130 = CARTESIAN_POINT ( 'NONE',  ( -1.489708121969999910, -39.36011816919999973, -22.89876977989999673 ) ) ;
#25131 = CARTESIAN_POINT ( 'NONE',  ( 14.73729790613776203, -95.40730986357353061, 17.32447803859898983 ) ) ;
#25132 = EDGE_CURVE ( 'NONE', #16242, #17051, #12723, .T. ) ;
#25133 = CIRCLE ( 'NONE', #3276, 59.33923303830000151 ) ;
#25134 = CARTESIAN_POINT ( 'NONE',  ( -38.51943391351900914, -63.07120704560256996, -2.875531170737058773 ) ) ;
#25135 = DIRECTION ( 'NONE',  ( 0.9295286103719527793, 0.000000000000000000, 0.3687499999999814260 ) ) ;
#25136 = CARTESIAN_POINT ( 'NONE',  ( 22.13628143409999893, -57.47600051900000295, -7.675802715190000569 ) ) ;
#25137 = CARTESIAN_POINT ( 'NONE',  ( -43.94912152850000098, -63.00000000000000000, -2.157414923720000210 ) ) ;
#25138 = CARTESIAN_POINT ( 'NONE',  ( 36.74383121569999844, -74.66666669110000498, -14.69280905019999928 ) ) ;
#25139 = EDGE_LOOP ( 'NONE', ( #757, #13338, #2423, #26974 ) ) ;
#25140 = CARTESIAN_POINT ( 'NONE',  ( 6.878957409089999864, -101.2902355740000075, 14.36654009489999950 ) ) ;
#25141 = DIRECTION ( 'NONE',  ( 0.7529607911047510038, 0.000000000000000000, -0.6580653820547830435 ) ) ;
#25142 = CARTESIAN_POINT ( 'NONE',  ( -12.91995238960000059, -67.00951448479999328, 22.59957177110000259 ) ) ;
#25143 = CARTESIAN_POINT ( 'NONE',  ( 7.289738943409999727, -36.07481395120000656, -21.45633483510000161 ) ) ;
#25144 = CARTESIAN_POINT ( 'NONE',  ( 7.248307137522641774, -73.87844996482074578, 39.84323359139695242 ) ) ;
#25145 = CARTESIAN_POINT ( 'NONE',  ( 23.44684503250000063, -93.13202985540000611, 11.98166338640000106 ) ) ;
#25146 = AXIS2_PLACEMENT_3D ( 'NONE', #26666, #15871, #6707 ) ;
#25147 = CARTESIAN_POINT ( 'NONE',  ( 20.21912291310000143, -36.00000000000000000, -9.726844800120000301 ) ) ;
#25148 = DIRECTION ( 'NONE',  ( -0.9295286103719533344, 0.000000000000000000, -0.3687499999999802047 ) ) ;
#25149 = AXIS2_PLACEMENT_3D ( 'NONE', #6116, #2194, #28405 ) ;
#25150 =( GEOMETRIC_REPRESENTATION_CONTEXT ( 3 ) GLOBAL_UNCERTAINTY_ASSIGNED_CONTEXT ( ( #13239 ) ) GLOBAL_UNIT_ASSIGNED_CONTEXT ( ( #11280, #28764, #15951 ) ) REPRESENTATION_CONTEXT ( 'NONE', 'WORKASPACE' ) );
#25151 = CARTESIAN_POINT ( 'NONE',  ( -11.29758003760461449, -43.98373191161520879, -22.34159391827311225 ) ) ;
#25152 = ORIENTED_EDGE ( 'NONE', *, *, #6891, .F. ) ;
#25153 = CARTESIAN_POINT ( 'NONE',  ( 8.071148094770000725, -100.8816835939999947, 13.57632622700000091 ) ) ;
#25154 = CARTESIAN_POINT ( 'NONE',  ( 27.68682485439999752, -31.69999999999999929, 50.68039294919999804 ) ) ;
#25155 = VERTEX_POINT ( 'NONE', #10316 ) ;
#25156 = CARTESIAN_POINT ( 'NONE',  ( -25.09792694589999940, -15.00000000000000000, -45.94144711499999545 ) ) ;
#25157 = ADVANCED_FACE ( 'NONE', ( #10042 ), #17348, .T. ) ;
#25158 = CARTESIAN_POINT ( 'NONE',  ( 0.5062329661385056578, -101.1248211537367894, -16.39898467942452953 ) ) ;
#25159 = DIRECTION ( 'NONE',  ( 0.4794255386042041156, 0.000000000000000000, 0.8775825618903720926 ) ) ;
#25160 = B_SPLINE_CURVE_WITH_KNOTS ( 'NONE', 3,
 ( #23303, #11790, #9747, #13981, #2928, #12215, #761, #7450, #23170, #25220, #18935, #12074, #20984, #27817, #16017, #2778, #26044, #19072, #27954, #26196, #6070, #4033, #23450, #3487, #7994, #16885, #19203, #3621, #23858 ),
 .UNSPECIFIED., .F., .F.,
 ( 4, 2, 1, 1, 2, 2, 2, 2, 1, 2, 2, 2, 2, 2, 2, 4 ),
 ( 0.000000000000000000, 0.1250000000000235922, 0.1875000000000369982, 0.2187500000000420219, 0.2343750000000474065, 0.2500000000000527911, 0.3750000000000170419, 0.4375000000000062728, 0.4687499999999934497, 0.4843749999999881761, 0.4999999999999829026, 0.6249999999999834577, 0.6874999999999762412, 0.7187499999999853451, 0.7499999999999943379, 1.000000000000000000 ),
 .UNSPECIFIED. ) ;
#25161 = DIRECTION ( 'NONE',  ( 0.000000000000000000, 0.000000000000000000, -1.000000000000000000 ) ) ;
#25162 = CARTESIAN_POINT ( 'NONE',  ( -7.215414233289999757, -74.50000000000000000, -40.70731707320000226 ) ) ;
#25163 = CARTESIAN_POINT ( 'NONE',  ( -14.78710411640000011, -74.50000000000000000, 36.35833236359999887 ) ) ;
#25164 = CARTESIAN_POINT ( 'NONE',  ( -21.05833095519999887, -65.01950792369999022, 13.71407545739999989 ) ) ;
#25165 = CARTESIAN_POINT ( 'NONE',  ( -13.68516050610000079, -43.03747692219999976, 20.93629851420000065 ) ) ;
#25166 = ORIENTED_EDGE ( 'NONE', *, *, #7322, .F. ) ;
#25167 = CARTESIAN_POINT ( 'NONE',  ( -12.35346744019999932, -72.02645921720001354, -25.58537703819999720 ) ) ;
#25168 = CARTESIAN_POINT ( 'NONE',  ( 8.805020426260000477, -34.63244859009999743, -20.36793841340000100 ) ) ;
#25169 = FACE_OUTER_BOUND ( 'NONE', #3356, .T. ) ;
#25170 = DIRECTION ( 'NONE',  ( 0.000000000000000000, 1.000000000000000000, 0.000000000000000000 ) ) ;
#25171 = AXIS2_PLACEMENT_3D ( 'NONE', #8634, #15325, #17252 ) ;
#25172 = CARTESIAN_POINT ( 'NONE',  ( 7.498734568567309466, -73.99999920929936081, -38.65106240728522380 ) ) ;
#25173 = ORIENTED_EDGE ( 'NONE', *, *, #22374, .T. ) ;
#25174 = VECTOR ( 'NONE', #17783, 1000.000000000000000 ) ;
#25175 = TOROIDAL_SURFACE ( 'NONE', #7032, 55.85192378860000417, 0.3499999999999999778 ) ;
#25176 = EDGE_LOOP ( 'NONE', ( #11796, #18303, #15972, #9729 ) ) ;
#25177 = EDGE_CURVE ( 'NONE', #11981, #22767, #1103, .T. ) ;
#25178 = DIRECTION ( 'NONE',  ( 0.4862861358100820097, 0.000000000000000000, 0.8737996304181516738 ) ) ;
#25179 = EDGE_CURVE ( 'NONE', #24085, #5884, #24327, .T. ) ;
#25180 = DIRECTION ( 'NONE',  ( 1.000000000000000000, 0.000000000000000000, 0.000000000000000000 ) ) ;
#25181 = CARTESIAN_POINT ( 'NONE',  ( -0.5009807240759999170, -95.72998414420000302, 22.40906914880000045 ) ) ;
#25182 = CARTESIAN_POINT ( 'NONE',  ( 11.26569178309999941, -92.63504499639999779, 27.45908696089999879 ) ) ;
#25183 = ORIENTED_EDGE ( 'NONE', *, *, #6926, .F. ) ;
#25184 = CARTESIAN_POINT ( 'NONE',  ( -11.21686577274311603, -94.79904837829768383, -20.68495353529920777 ) ) ;
#25185 = ORIENTED_EDGE ( 'NONE', *, *, #25916, .F. ) ;
#25186 = CARTESIAN_POINT ( 'NONE',  ( -27.90659341333026688, -93.31462968106396261, 0.8904257685511188791 ) ) ;
#25187 = CARTESIAN_POINT ( 'NONE',  ( -2.790536503729999840, -64.24504439390000243, -26.36014981959999659 ) ) ;
#25188 = CARTESIAN_POINT ( 'NONE',  ( 47.04659111560000184, -74.36053120809999939, -1.844552627969999969 ) ) ;
#25189 = ORIENTED_EDGE ( 'NONE', *, *, #352, .F. ) ;
#25190 = AXIS2_PLACEMENT_3D ( 'NONE', #16618, #18529, #11812 ) ;
#25191 = CARTESIAN_POINT ( 'NONE',  ( 7.244686332491783176, -74.17170883796306669, -40.27753662853213967 ) ) ;
#25192 = LINE ( 'NONE', #27082, #5284 ) ;
#25193 = AXIS2_PLACEMENT_3D ( 'NONE', #23824, #28333, #28751 ) ;
#25194 = ORIENTED_EDGE ( 'NONE', *, *, #27470, .T. ) ;
#25195 = AXIS2_PLACEMENT_3D ( 'NONE', #20451, #4714, #20756 ) ;
#25196 = CARTESIAN_POINT ( 'NONE',  ( -11.20154639050000078, -94.96739875689999621, -21.25936308859999713 ) ) ;
#25197 = CARTESIAN_POINT ( 'NONE',  ( -2.372222499579999866, -65.21231684830000574, -25.69919413619999915 ) ) ;
#25198 = CARTESIAN_POINT ( 'NONE',  ( -15.70782602609999756, -68.38632221809999123, 23.02257119289999920 ) ) ;
#25199 = EDGE_LOOP ( 'NONE', ( #11248, #27691, #21542, #18829 ) ) ;
#25200 = FACE_OUTER_BOUND ( 'NONE', #16742, .T. ) ;
#25201 = CARTESIAN_POINT ( 'NONE',  ( -15.71880468089999816, -100.6825640990000039, 2.591412482229999981 ) ) ;
#25202 = CARTESIAN_POINT ( 'NONE',  ( 26.04683907640000129, -62.95225063429998613, 1.424128180149999867 ) ) ;
#25203 = FACE_OUTER_BOUND ( 'NONE', #2647, .T. ) ;
#25204 = ORIENTED_EDGE ( 'NONE', *, *, #13137, .F. ) ;
#25205 = CARTESIAN_POINT ( 'NONE',  ( -1.068597827310000081, -18.61776472269999871, -21.62742878349999742 ) ) ;
#25206 = CARTESIAN_POINT ( 'NONE',  ( -7.915630935209213348, -100.0863963177362166, 15.30813341843738229 ) ) ;
#25207 = ORIENTED_EDGE ( 'NONE', *, *, #2092, .F. ) ;
#25208 = CARTESIAN_POINT ( 'NONE',  ( -8.556134930689999862, -94.37361474979999798, -22.79835356780000311 ) ) ;
#25209 = CARTESIAN_POINT ( 'NONE',  ( 23.15409266789999876, -63.61851004920001174, 10.62027102839999948 ) ) ;
#25210 = CARTESIAN_POINT ( 'NONE',  ( 8.964905012660000949, -34.98556513209999963, -19.94240293869999903 ) ) ;
#25211 = CARTESIAN_POINT ( 'NONE',  ( 16.65148481214054854, -100.1240332945786662, 4.321656103344765576 ) ) ;
#25212 = CARTESIAN_POINT ( 'NONE',  ( 19.83536231727052268, -94.71481465627687157, 14.13922899595298333 ) ) ;
#25213 = ORIENTED_EDGE ( 'NONE', *, *, #3727, .T. ) ;
#25214 = CIRCLE ( 'NONE', #10729, 0.4999999999999997780 ) ;
#25215 = VECTOR ( 'NONE', #2783, 1000.000000000000000 ) ;
#25216 = AXIS2_PLACEMENT_3D ( 'NONE', #6179, #1409, #14909 ) ;
#25217 = UNCERTAINTY_MEASURE_WITH_UNIT (LENGTH_MEASURE( 1.000000000000000082E-05 ), #7186, 'distance_accuracy_value', 'NONE');
#25218 = EDGE_CURVE ( 'NONE', #12823, #14426, #8421, .T. ) ;
#25219 = CARTESIAN_POINT ( 'NONE',  ( -11.65671671230000150, -61.59933877579999972, -22.96881371439999953 ) ) ;
#25220 = CARTESIAN_POINT ( 'NONE',  ( 37.04698255873401536, -79.90156983920238076, -14.18878285662181327 ) ) ;
#25221 = CARTESIAN_POINT ( 'NONE',  ( 25.45277885500000181, -67.58729785420000269, -10.39245563309999909 ) ) ;
#25222 = CARTESIAN_POINT ( 'NONE',  ( 6.393980055115425998, -93.41742240778975770, 26.81347393697559411 ) ) ;
#25223 = ADVANCED_FACE ( 'NONE', ( #17616 ), #704, .F. ) ;
#25224 = VERTEX_POINT ( 'NONE', #15405 ) ;
#25225 = CARTESIAN_POINT ( 'NONE',  ( 47.00563892014582024, -74.15410710641695857, -1.866436577246293638 ) ) ;
#25226 = ORIENTED_EDGE ( 'NONE', *, *, #20063, .F. ) ;
#25227 = CARTESIAN_POINT ( 'NONE',  ( -10.61285196099999872, -19.46348300730000247, 19.30929595470000137 ) ) ;
#25228 = EDGE_CURVE ( 'NONE', #27862, #23133, #13913, .T. ) ;
#25229 = VERTEX_POINT ( 'NONE', #20239 ) ;
#25230 = CARTESIAN_POINT ( 'NONE',  ( -31.00000000000000000, -13.00000000000000000, -4.500000000000000000 ) ) ;
#25231 = ADVANCED_FACE ( 'NONE', ( #7278 ), #23910, .F. ) ;
#25232 = ORIENTED_EDGE ( 'NONE', *, *, #11674, .T. ) ;
#25233 = CARTESIAN_POINT ( 'NONE',  ( 39.18035607830000089, -73.62951539670000045, 7.219507042780000106 ) ) ;
#25234 = CARTESIAN_POINT ( 'NONE',  ( -10.47910890883315993, -19.47294349888635523, -20.23264493352919402 ) ) ;
#25235 = DIRECTION ( 'NONE',  ( 0.000000000000000000, -1.000000000000000000, 0.000000000000000000 ) ) ;
#25236 = CARTESIAN_POINT ( 'NONE',  ( -9.365829542560001997, -18.50000000000000000, -20.82431110010000097 ) ) ;
#25237 = AXIS2_PLACEMENT_3D ( 'NONE', #18053, #26952, #22140 ) ;
#25238 = CARTESIAN_POINT ( 'NONE',  ( 46.70777991640400728, -79.88906770808442559, -3.456174201335132423 ) ) ;
#25239 = ORIENTED_EDGE ( 'NONE', *, *, #20576, .T. ) ;
#25240 = CARTESIAN_POINT ( 'NONE',  ( -50.00000000000000000, -11.00000000000000000, -2.486899575159999765E-14 ) ) ;
#25241 = CARTESIAN_POINT ( 'NONE',  ( 16.83481230680000351, -99.92967428129999519, 4.239616764530000026 ) ) ;
#25242 = CARTESIAN_POINT ( 'NONE',  ( -19.88566801240000004, -92.51556124920000457, 20.76300894400000274 ) ) ;
#25243 = DIRECTION ( 'NONE',  ( 0.000000000000000000, 1.000000000000000000, 0.000000000000000000 ) ) ;
#25244 = EDGE_LOOP ( 'NONE', ( #3571, #11572, #12121, #18193 ) ) ;
#25245 = DIRECTION ( 'NONE',  ( 0.000000000000000000, -1.000000000000000000, 0.000000000000000000 ) ) ;
#25246 = CARTESIAN_POINT ( 'NONE',  ( 7.292753731799999528, -92.50000000000000000, -29.01615345709999971 ) ) ;
#25247 = DIRECTION ( 'NONE',  ( 0.000000000000000000, 1.000000000000000000, 0.000000000000000000 ) ) ;
#25248 = ORIENTED_EDGE ( 'NONE', *, *, #11635, .T. ) ;
#25249 = CARTESIAN_POINT ( 'NONE',  ( -18.15843401709999938, -97.14937512070000025, 11.14356573500000103 ) ) ;
#25250 = CARTESIAN_POINT ( 'NONE',  ( -19.60499002909999788, -45.96202241439999625, 14.06799618039999977 ) ) ;
#25251 = FACE_OUTER_BOUND ( 'NONE', #25385, .T. ) ;
#25252 = CARTESIAN_POINT ( 'NONE',  ( -38.18612978632862820, -65.73322674265560295, 1.234409484183223604 ) ) ;
#25253 = CARTESIAN_POINT ( 'NONE',  ( -14.82555510052299219, -74.28534546674652006, 36.29020547809800235 ) ) ;
#25254 = AXIS2_PLACEMENT_3D ( 'NONE', #5749, #20929, #14360 ) ;
#25255 = DIRECTION ( 'NONE',  ( 1.000000000000000000, 0.000000000000000000, 0.000000000000000000 ) ) ;
#25256 = FACE_OUTER_BOUND ( 'NONE', #7250, .T. ) ;
#25257 = AXIS2_PLACEMENT_3D ( 'NONE', #23382, #14348, #1252 ) ;
#25258 = ADVANCED_FACE ( 'NONE', ( #11776 ), #20091, .T. ) ;
#25259 = ORIENTED_EDGE ( 'NONE', *, *, #17372, .T. ) ;
#25260 = CARTESIAN_POINT ( 'NONE',  ( 20.34628061889999984, -52.63293862049999916, 11.13082833170000008 ) ) ;
#25261 = CARTESIAN_POINT ( 'NONE',  ( -39.27497438212488845, -73.60295742112906225, -7.213678002770810060 ) ) ;
#25262 = FACE_OUTER_BOUND ( 'NONE', #27927, .T. ) ;
#25263 = ORIENTED_EDGE ( 'NONE', *, *, #19654, .T. ) ;
#25264 = DIRECTION ( 'NONE',  ( 1.000000000000000000, 0.000000000000000000, 0.000000000000000000 ) ) ;
#25265 = CARTESIAN_POINT ( 'NONE',  ( 27.70978180510000044, -92.50000000000000000, 12.74433177200000067 ) ) ;
#25266 = EDGE_CURVE ( 'NONE', #7118, #1115, #7319, .T. ) ;
#25267 = B_SPLINE_SURFACE_WITH_KNOTS ( 'NONE', 5, 5, ( 
 ( #16155, #25062, #15863, #22441, #13687, #5096, #2924, #11787, #2486 ),
 ( #20698, #13326, #26607, #6798, #2136, #13478, #8664, #11287, #6648 ),
 ( #1995, #15660, #21794, #10689, #28632, #20193, #267, #9108, #15356 ),
 ( #15510, #2433, #2281, #1849, #4457, #17572, #11128, #19608, #18009 ),
 ( #26465, #22385, #24718, #26907, #21948, #8810, #24562, #28491, #17722 ),
 ( #19888, #6948, #15808, #17431, #12878, #26767, #24420, #8528, #22230 ) ),
 .UNSPECIFIED., .F., .F., .F.,
 ( 6, 6 ),
 ( 6, 3, 6 ),
 ( 0.000000000000000000, 46.92994236199999847 ),
 ( 0.000000000000000000, 1.000000000000000000, 2.000000000000000000 ),
 .UNSPECIFIED. ) ;
#25268 = FACE_BOUND ( 'NONE', #18623, .T. ) ;
#25269 = CARTESIAN_POINT ( 'NONE',  ( -8.022941090739999837, -100.0496341300000154, 14.88870835790000058 ) ) ;
#25270 = CARTESIAN_POINT ( 'NONE',  ( -18.36547013180332399, -18.60284036876689839, 11.26451427426198215 ) ) ;
#25271 = FACE_OUTER_BOUND ( 'NONE', #18950, .T. ) ;
#25272 = CARTESIAN_POINT ( 'NONE',  ( 7.394414626720000605, -101.1280782930000015, 13.63119500039999998 ) ) ;
#25273 = VERTEX_POINT ( 'NONE', #11176 ) ;
#25274 = CARTESIAN_POINT ( 'NONE',  ( 7.215414233289999757, -82.25000000000000000, -40.70731707320000226 ) ) ;
#25275 = CARTESIAN_POINT ( 'NONE',  ( -42.63274768570000361, -81.75000000000000000, -1.438276615809999992 ) ) ;
#25276 = CARTESIAN_POINT ( 'NONE',  ( -12.71855576417205924, -19.47933348071434523, 19.41975311732825560 ) ) ;
#25277 = CARTESIAN_POINT ( 'NONE',  ( 12.11202172750000017, -100.0012764439999984, -13.34364409169999988 ) ) ;
#25278 = ORIENTED_EDGE ( 'NONE', *, *, #13066, .F. ) ;
#25279 = CARTESIAN_POINT ( 'NONE',  ( -1.588567434916923649, -19.46686856772270602, -22.26502320241943522 ) ) ;
#25280 = AXIS2_PLACEMENT_3D ( 'NONE', #8590, #11037, #17933 ) ;
#25281 = CARTESIAN_POINT ( 'NONE',  ( 11.58748549300000086, -101.1411470200000053, -10.12711838239999906 ) ) ;
#25282 = VECTOR ( 'NONE', #21752, 1000.000000000000000 ) ;
#25283 = CARTESIAN_POINT ( 'NONE',  ( -2.406257486749999952, -39.32886505749999628, -23.82325412870000036 ) ) ;
#25284 = CARTESIAN_POINT ( 'NONE',  ( -16.94283757680843294, -92.86276749033184785, 25.36152676960142927 ) ) ;
#25285 = DIRECTION ( 'NONE',  ( 1.000000000000000000, 0.000000000000000000, 0.000000000000000000 ) ) ;
#25286 = DIRECTION ( 'NONE',  ( 0.000000000000000000, -1.000000000000000000, 0.000000000000000000 ) ) ;
#25287 = CARTESIAN_POINT ( 'NONE',  ( 21.74683343679999936, -44.92713668010000561, -7.877988450920000219 ) ) ;
#25288 = CYLINDRICAL_SURFACE ( 'NONE', #6722, 18.64285714290000229 ) ;
#25289 = CYLINDRICAL_SURFACE ( 'NONE', #225, 30.50000000000002132 ) ;
#25290 = EDGE_LOOP ( 'NONE', ( #28102, #3979, #17456, #15738 ) ) ;
#25291 = CARTESIAN_POINT ( 'NONE',  ( 6.496108347790000792, -101.2358105800000061, 13.76101799030000095 ) ) ;
#25292 = CARTESIAN_POINT ( 'NONE',  ( -32.67527180329999936, -79.50000000000055422, -22.00249031559999935 ) ) ;
#25293 = CIRCLE ( 'NONE', #27150, 7.250000000000000000 ) ;
#25294 = ADVANCED_FACE ( 'NONE', ( #15704 ), #18493, .T. ) ;
#25295 = EDGE_CURVE ( 'NONE', #139, #20804, #9299, .T. ) ;
#25296 = CARTESIAN_POINT ( 'NONE',  ( -11.38188984059999775, -94.78088171070000101, -20.62154665490000127 ) ) ;
#25297 = DIRECTION ( 'NONE',  ( 0.000000000000000000, -1.000000000000000000, 0.000000000000000000 ) ) ;
#25298 = FACE_OUTER_BOUND ( 'NONE', #16115, .T. ) ;
#25299 = AXIS2_PLACEMENT_3D ( 'NONE', #1425, #28205, #14664 ) ;
#25300 = CARTESIAN_POINT ( 'NONE',  ( 16.79922297439999923, -99.53431386179998697, 4.586272525910000120 ) ) ;
#25301 = CIRCLE ( 'NONE', #14579, 5.500000000000001776 ) ;
#25302 = CARTESIAN_POINT ( 'NONE',  ( -7.105427357599999217E-15, -84.00000000000000000, -3.552713678799999608E-15 ) ) ;
#25303 = ADVANCED_FACE ( 'NONE', ( #5083 ), #9008, .T. ) ;
#25304 = DIRECTION ( 'NONE',  ( 0.000000000000000000, 1.000000000000000000, 0.000000000000000000 ) ) ;
#25305 = ORIENTED_EDGE ( 'NONE', *, *, #24848, .T. ) ;
#25306 = CARTESIAN_POINT ( 'NONE',  ( 30.67453910217138002, -74.17429583352173950, -24.29361569179353353 ) ) ;
#25307 = CARTESIAN_POINT ( 'NONE',  ( -20.43643619460000238, -93.49011727610000833, 16.37406953600000037 ) ) ;
#25308 = ORIENTED_EDGE ( 'NONE', *, *, #5155, .T. ) ;
#25309 = DIRECTION ( 'NONE',  ( 0.000000000000000000, 1.000000000000000000, 0.000000000000000000 ) ) ;
#25310 = CARTESIAN_POINT ( 'NONE',  ( -0.007034495156453384086, -101.6297509123136393, -16.01459432531875748 ) ) ;
#25311 = CARTESIAN_POINT ( 'NONE',  ( -7.528851423409999022, -74.04592585209999811, 39.12588484300000147 ) ) ;
#25312 = CARTESIAN_POINT ( 'NONE',  ( -12.89904789370000060, -65.07443093669999712, -21.58991903219999742 ) ) ;
#25313 = CARTESIAN_POINT ( 'NONE',  ( 26.51571562290000017, -74.19534091600000636, -28.99561388480000090 ) ) ;
#25314 = CARTESIAN_POINT ( 'NONE',  ( 10.16048931789999976, -72.75494322130001024, -26.79207077499999912 ) ) ;
#25315 = B_SPLINE_CURVE_WITH_KNOTS ( 'NONE', 5,
 ( #25451, #27202, #14079, #997, #15963, #22980 ),
 .UNSPECIFIED., .F., .F.,
 ( 6, 6 ),
 ( 0.000000000000000000, 1.000000000000000000 ),
 .UNSPECIFIED. ) ;
#25316 = CARTESIAN_POINT ( 'NONE',  ( 23.92048446921776161, -92.96960399593338309, -18.92248458225377661 ) ) ;
#25317 = CARTESIAN_POINT ( 'NONE',  ( -12.84661343289999991, -72.82938918050000154, -25.64624284649999808 ) ) ;
#25318 = CARTESIAN_POINT ( 'NONE',  ( 8.132924317199998754, -25.50459660499999970, -20.70967061410000198 ) ) ;
#25319 = CARTESIAN_POINT ( 'NONE',  ( -1.156001381987856513, -57.47571023478692354, -23.39939165675805910 ) ) ;
#25320 = CIRCLE ( 'NONE', #20173, 0.4999999999999982236 ) ;
#25321 = DIRECTION ( 'NONE',  ( 0.000000000000000000, -1.000000000000000000, 0.000000000000000000 ) ) ;
#25322 = ORIENTED_EDGE ( 'NONE', *, *, #9898, .F. ) ;
#25323 = CARTESIAN_POINT ( 'NONE',  ( -27.18988201479999844, -20.30155444569999901, -49.77074518290000071 ) ) ;
#25324 = VERTEX_POINT ( 'NONE', #2764 ) ;
#25325 = EDGE_CURVE ( 'NONE', #2790, #24185, #19126, .T. ) ;
#25326 = TOROIDAL_SURFACE ( 'NONE', #7184, 43.34897771020000334, 20.00000000000000000 ) ;
#25327 = CARTESIAN_POINT ( 'NONE',  ( -1.156026911079999886, -57.91337896769999816, -23.41449751500000076 ) ) ;
#25328 = AXIS2_PLACEMENT_3D ( 'NONE', #17407, #4572, #22068 ) ;
#25329 = DIRECTION ( 'NONE',  ( 0.000000000000000000, -1.000000000000000000, 0.000000000000000000 ) ) ;
#25330 = EDGE_CURVE ( 'NONE', #3267, #12297, #10074, .T. ) ;
#25331 = CARTESIAN_POINT ( 'NONE',  ( 4.060851860889999720, -93.80272730500000478, 26.06633832969999887 ) ) ;
#25332 = ORIENTED_EDGE ( 'NONE', *, *, #4581, .T. ) ;
#25333 = FACE_OUTER_BOUND ( 'NONE', #27696, .T. ) ;
#25334 = CARTESIAN_POINT ( 'NONE',  ( 20.58262107270000030, -36.00000000000000000, -9.698193473849999080 ) ) ;
#25335 = CARTESIAN_POINT ( 'NONE',  ( -0.6441375867304897085, -93.86980009075321618, 25.50348311024104575 ) ) ;
#25336 = ORIENTED_EDGE ( 'NONE', *, *, #8666, .F. ) ;
#25337 = AXIS2_PLACEMENT_3D ( 'NONE', #14710, #17041, #16485 ) ;
#25338 = CARTESIAN_POINT ( 'NONE',  ( -4.500000000000000000, 0.000000000000000000, -50.00000000000000000 ) ) ;
#25339 = CARTESIAN_POINT ( 'NONE',  ( 0.000000000000000000, -16.00000000000000000, 0.000000000000000000 ) ) ;
#25340 = CARTESIAN_POINT ( 'NONE',  ( 0.000000000000000000, -11.85850980319999870, 0.000000000000000000 ) ) ;
#25341 = CARTESIAN_POINT ( 'NONE',  ( -1.816673240429999892, -68.12125821070000598, -26.48053705119999890 ) ) ;
#25342 = CARTESIAN_POINT ( 'NONE',  ( -15.36964020949999998, -68.58917995980000626, 22.84471883390000002 ) ) ;
#25343 = ORIENTED_EDGE ( 'NONE', *, *, #9071, .T. ) ;
#25344 = CARTESIAN_POINT ( 'NONE',  ( 36.62466550090000084, -74.65121098390000043, -14.68734464040000098 ) ) ;
#25345 = AXIS2_PLACEMENT_3D ( 'NONE', #20310, #28615, #2404 ) ;
#25346 = CARTESIAN_POINT ( 'NONE',  ( -15.80605669150000203, -101.3276421320000082, 3.296406198950000199 ) ) ;
#25347 = CARTESIAN_POINT ( 'NONE',  ( -20.73247391559999997, -63.62260287809999681, 13.04049290600000077 ) ) ;
#25348 = ADVANCED_FACE ( 'NONE', ( #11924 ), #19202, .T. ) ;
#25349 = EDGE_LOOP ( 'NONE', ( #26922, #20514, #20465, #14731, #14067 ) ) ;
#25350 = VECTOR ( 'NONE', #11284, 1000.000000000000000 ) ;
#25351 = CARTESIAN_POINT ( 'NONE',  ( 7.215414233289999757, -82.25000000000000000, 40.70731707320000226 ) ) ;
#25352 = CARTESIAN_POINT ( 'NONE',  ( -3.667491169959999908, -18.50000000000000000, -24.01996181969999711 ) ) ;
#25353 = CARTESIAN_POINT ( 'NONE',  ( 36.22844186549999534, -74.00000000000000000, -13.75000000000000000 ) ) ;
#25354 = VERTEX_POINT ( 'NONE', #26329 ) ;
#25355 = DIRECTION ( 'NONE',  ( -1.000000000000000000, 0.000000000000000000, 6.505213034913020688E-16 ) ) ;
#25356 = CARTESIAN_POINT ( 'NONE',  ( -40.50000000000000000, -63.30468293320000583, -2.309401076760000393 ) ) ;
#25357 = DIRECTION ( 'NONE',  ( 0.000000000000000000, -1.000000000000000000, 0.000000000000000000 ) ) ;
#25358 = CARTESIAN_POINT ( 'NONE',  ( 16.68572014148854166, -100.0863963178369431, 4.310789395909731425 ) ) ;
#25359 = DIRECTION ( 'NONE',  ( 0.000000000000000000, 1.000000000000000000, 0.000000000000000000 ) ) ;
#25360 = VERTEX_POINT ( 'NONE', #3750 ) ;
#25361 = AXIS2_PLACEMENT_3D ( 'NONE', #4578, #2698, #22360 ) ;
#25362 = EDGE_CURVE ( 'NONE', #1165, #8148, #14916, .T. ) ;
#25363 = CIRCLE ( 'NONE', #11366, 0.5000000000000004441 ) ;
#25364 = DIRECTION ( 'NONE',  ( 0.000000000000000000, -1.000000000000000000, 0.000000000000000000 ) ) ;
#25365 = DIRECTION ( 'NONE',  ( 0.000000000000000000, 1.000000000000000000, 0.000000000000000000 ) ) ;
#25366 = CARTESIAN_POINT ( 'NONE',  ( 8.971603365988027434, -93.12686175135999633, 27.38471516527505756 ) ) ;
#25367 = EDGE_LOOP ( 'NONE', ( #26780, #10057, #14283, #8488, #16293, #9568, #27263, #14688, #9890, #22603, #24284, #22450, #7696, #2743, #8157, #2896 ) ) ;
#25368 = DIRECTION ( 'NONE',  ( -0.7071067811865470176, 0.000000000000000000, 0.7071067811865480168 ) ) ;
#25369 = LINE ( 'NONE', #11795, #11383 ) ;
#25370 = ORIENTED_EDGE ( 'NONE', *, *, #26696, .F. ) ;
#25371 = TOROIDAL_SURFACE ( 'NONE', #18396, 7.750000000000000000, 0.5000000000000000000 ) ;
#25372 = CARTESIAN_POINT ( 'NONE',  ( -13.46142422580000009, -34.61116027599999256, 20.44677669700000422 ) ) ;
#25373 = CARTESIAN_POINT ( 'NONE',  ( 28.69894246159999796, -72.00000000000000000, -10.33698060819999931 ) ) ;
#25374 = ORIENTED_EDGE ( 'NONE', *, *, #14703, .F. ) ;
#25375 = DIRECTION ( 'NONE',  ( 0.000000000000000000, 1.000000000000000000, 0.000000000000000000 ) ) ;
#25376 = CARTESIAN_POINT ( 'NONE',  ( 40.70731707320000226, -74.50000000000000000, 7.215414233289999757 ) ) ;
#25377 = DIRECTION ( 'NONE',  ( 1.000000000000000000, 0.000000000000000000, 0.000000000000000000 ) ) ;
#25378 = FACE_OUTER_BOUND ( 'NONE', #2775, .T. ) ;
#25379 = CARTESIAN_POINT ( 'NONE',  ( 7.635702898730000854, -101.6454117330000031, 14.06304778130000166 ) ) ;
#25380 = VERTEX_POINT ( 'NONE', #19755 ) ;
#25381 = CARTESIAN_POINT ( 'NONE',  ( -32.63327488449999692, -79.88238632670000072, -22.07483759460000172 ) ) ;
#25382 = CARTESIAN_POINT ( 'NONE',  ( 21.27250945180000130, -96.93384555780001222, 0.8126110531310000162 ) ) ;
#25383 = EDGE_CURVE ( 'NONE', #17197, #11057, #12486, .T. ) ;
#25384 = DIRECTION ( 'NONE',  ( 0.000000000000000000, 1.000000000000000000, 0.000000000000000000 ) ) ;
#25385 = EDGE_LOOP ( 'NONE', ( #20482, #18654, #9010, #18943 ) ) ;
#25386 = AXIS2_PLACEMENT_3D ( 'NONE', #2818, #11828, #800 ) ;
#25387 = CARTESIAN_POINT ( 'NONE',  ( 29.72283664746381149, -92.84927079009172246, 6.841275840752675030 ) ) ;
#25388 = CARTESIAN_POINT ( 'NONE',  ( -6.514305738480000052, -74.00000000000000000, 35.51864961870000315 ) ) ;
#25389 = EDGE_LOOP ( 'NONE', ( #24295, #13230, #19658, #8815 ) ) ;
#25390 = CARTESIAN_POINT ( 'NONE',  ( 3.595691539529999758, -0.5000000000000000000, 6.581869214180000149 ) ) ;
#25391 = AXIS2_PLACEMENT_3D ( 'NONE', #26810, #4803, #2327 ) ;
#25392 = B_SPLINE_CURVE_WITH_KNOTS ( 'NONE', 5,
 ( #14049, #21191, #27878, #5014, #22805, #2843 ),
 .UNSPECIFIED., .F., .F.,
 ( 6, 6 ),
 ( 0.000000000000000000, 1.000000000000000000 ),
 .UNSPECIFIED. ) ;
#25393 = CARTESIAN_POINT ( 'NONE',  ( -20.17987348730000008, -39.29539198449999304, 14.62286557340000215 ) ) ;
#25394 = DIRECTION ( 'NONE',  ( -9.436895709310000674E-16, 0.000000000000000000, 1.000000000000000000 ) ) ;
#25395 = CARTESIAN_POINT ( 'NONE',  ( -38.25000000000000711, -65.67306013599088033, 1.491601497604051918 ) ) ;
#25396 = EDGE_CURVE ( 'NONE', #11515, #21778, #10552, .T. ) ;
#25397 = CARTESIAN_POINT ( 'NONE',  ( 23.27434332070000167, -58.85141487709999808, -9.477375906779998971 ) ) ;
#25398 = MANIFOLD_SOLID_BREP ( 'Rotational Bodies', #19785 ) ;
#25399 = ORIENTED_EDGE ( 'NONE', *, *, #16722, .F. ) ;
#25400 = FACE_BOUND ( 'NONE', #25443, .T. ) ;
#25401 = CARTESIAN_POINT ( 'NONE',  ( -22.22906643760000023, -79.50000000000000000, -32.83566815539999340 ) ) ;
#25402 = ORIENTED_EDGE ( 'NONE', *, *, #2484, .T. ) ;
#25403 = CARTESIAN_POINT ( 'NONE',  ( 7.215414233289999757, -74.50000000000000000, 40.70731707320000226 ) ) ;
#25404 = CARTESIAN_POINT ( 'NONE',  ( -41.75000000000000000, -63.30468293320000583, 1.587713240270000048 ) ) ;
#25405 = CARTESIAN_POINT ( 'NONE',  ( -18.13877171349999884, -92.50000171950000549, -23.79299170569999688 ) ) ;
#25406 = DIRECTION ( 'NONE',  ( 0.000000000000000000, 1.000000000000000000, 0.000000000000000000 ) ) ;
#25407 = DIRECTION ( 'NONE',  ( 0.000000000000000000, -1.000000000000000000, 0.000000000000000000 ) ) ;
#25408 = CARTESIAN_POINT ( 'NONE',  ( 7.345882526619999631, -101.1398235650000146, 13.52469188849999959 ) ) ;
#25409 = ORIENTED_EDGE ( 'NONE', *, *, #19619, .F. ) ;
#25410 = CARTESIAN_POINT ( 'NONE',  ( -43.25910744576837175, -65.11704020644228308, -0.1219423816561529955 ) ) ;
#25411 = CARTESIAN_POINT ( 'NONE',  ( -23.87973397989999924, -93.75379239759999450, -7.203585628490000836 ) ) ;
#25412 = CARTESIAN_POINT ( 'NONE',  ( 12.03370358959999820, -98.60488091059998794, -15.63955140670000077 ) ) ;
#25413 = ORIENTED_EDGE ( 'NONE', *, *, #14294, .T. ) ;
#25414 = CARTESIAN_POINT ( 'NONE',  ( 20.35668408949999986, -18.85700241039999980, -8.076030211610000009 ) ) ;
#25415 = ADVANCED_FACE ( 'NONE', ( #26184 ), #6215, .F. ) ;
#25416 = DIRECTION ( 'NONE',  ( 0.000000000000000000, 0.000000000000000000, -1.000000000000000000 ) ) ;
#25417 = LINE ( 'NONE', #18277, #28785 ) ;
#25418 = DIRECTION ( 'NONE',  ( 0.5853721519882836288, 0.000000000000000000, 0.8107647276963926286 ) ) ;
#25419 = EDGE_CURVE ( 'NONE', #27403, #24185, #28152, .T. ) ;
#25420 = CARTESIAN_POINT ( 'NONE',  ( -37.81585169939486946, -65.66527311162126068, 0.7597073328712810047 ) ) ;
#25421 = CARTESIAN_POINT ( 'NONE',  ( 20.33060048340120574, -36.00000012572794361, -9.320855385822547134 ) ) ;
#25422 = CARTESIAN_POINT ( 'NONE',  ( 22.19980545599999999, -53.27760474010000280, -8.563702697329999225 ) ) ;
#25423 = EDGE_CURVE ( 'NONE', #4890, #24185, #22540, .T. ) ;
#25424 = DIRECTION ( 'NONE',  ( 0.000000000000000000, -1.000000000000000000, 0.000000000000000000 ) ) ;
#25425 = DIRECTION ( 'NONE',  ( 0.4794255386042042266, 0.000000000000000000, 0.8775825618903720926 ) ) ;
#25426 = ORIENTED_EDGE ( 'NONE', *, *, #10950, .F. ) ;
#25427 = ADVANCED_FACE ( 'NONE', ( #24873 ), #22550, .F. ) ;
#25428 = CARTESIAN_POINT ( 'NONE',  ( 7.023258447689999961, -101.4254868729999970, 14.34178107630000021 ) ) ;
#25429 = CARTESIAN_POINT ( 'NONE',  ( -35.61208719050000582, -66.25000000000000000, 2.397127693020000283 ) ) ;
#25430 = CARTESIAN_POINT ( 'NONE',  ( 7.635702898730000854, -101.6454117330000031, 14.06304778130000166 ) ) ;
#25431 = AXIS2_PLACEMENT_3D ( 'NONE', #16048, #4980, #13867 ) ;
#25432 = DIRECTION ( 'NONE',  ( 0.000000000000000000, 1.000000000000000000, 0.000000000000000000 ) ) ;
#25433 = CARTESIAN_POINT ( 'NONE',  ( 8.773402987799999053, -35.75421199320000198, -20.69709838450000206 ) ) ;
#25434 = CARTESIAN_POINT ( 'NONE',  ( 7.169550435208813965, -73.50000000000002842, 38.90587669203541310 ) ) ;
#25435 = CARTESIAN_POINT ( 'NONE',  ( 22.96745989159999723, -18.50000000000000000, 9.091461454319999191 ) ) ;
#25436 = CARTESIAN_POINT ( 'NONE',  ( -19.58257540287776166, -93.15741110474085929, -20.89612884129461179 ) ) ;
#25437 = CARTESIAN_POINT ( 'NONE',  ( 0.3059185938709999553, -111.0000000000000000, 14.72672055670000013 ) ) ;
#25438 = EDGE_LOOP ( 'NONE', ( #3970, #11036, #5764, #10435 ) ) ;
#25439 = SPHERICAL_SURFACE ( 'NONE', #17096, 2.000000000000000000 ) ;
#25440 = CARTESIAN_POINT ( 'NONE',  ( -17.09009608839999927, -99.55609322370000314, 3.193624944930000265 ) ) ;
#25441 = ORIENTED_EDGE ( 'NONE', *, *, #12355, .F. ) ;
#25442 = CARTESIAN_POINT ( 'NONE',  ( 27.35691629450000306, -72.00000000000000000, -11.81987123310000065 ) ) ;
#25443 = EDGE_LOOP ( 'NONE', ( #27538, #3403 ) ) ;
#25444 = CARTESIAN_POINT ( 'NONE',  ( 8.489585298007764180, -93.04141874247987687, -27.18617793450870579 ) ) ;
#25445 = CARTESIAN_POINT ( 'NONE',  ( -7.253522899010000025, -73.81625264650000418, 39.23046895160000247 ) ) ;
#25446 = CARTESIAN_POINT ( 'NONE',  ( 13.12524984231539804, -92.96960399592983038, 27.53139692395792792 ) ) ;
#25447 = CARTESIAN_POINT ( 'NONE',  ( -12.09704001540000107, -80.00000000000000000, 47.10905722069999513 ) ) ;
#25448 = CARTESIAN_POINT ( 'NONE',  ( -23.16986609970000188, -72.82938648530000592, 16.90925194980000157 ) ) ;
#25449 = CARTESIAN_POINT ( 'NONE',  ( 21.84907504069999717, -73.17614430409999215, -31.22910235029999981 ) ) ;
#25450 = EDGE_CURVE ( 'NONE', #8830, #28301, #14160, .T. ) ;
#25451 = CARTESIAN_POINT ( 'NONE',  ( -1.604070449259999753, -100.9197075889999979, -15.54198650660000069 ) ) ;
#25452 = CARTESIAN_POINT ( 'NONE',  ( 23.79740151902118228, -92.74292563041596793, -19.07705719069169348 ) ) ;
#25453 = FACE_OUTER_BOUND ( 'NONE', #6698, .T. ) ;
#25454 = CARTESIAN_POINT ( 'NONE',  ( 8.972032747380000117, -25.54957623849999848, -19.59884268089999892 ) ) ;
#25455 = FACE_OUTER_BOUND ( 'NONE', #16632, .T. ) ;
#25456 = PRESENTATION_STYLE_ASSIGNMENT (( #16559 ) ) ;
#25457 = VERTEX_POINT ( 'NONE', #26619 ) ;
#25458 = EDGE_CURVE ( 'NONE', #927, #1616, #4385, .T. ) ;
#25459 = DIRECTION ( 'NONE',  ( 1.000000000000000000, 0.000000000000000000, 0.000000000000000000 ) ) ;
#25460 = VERTEX_POINT ( 'NONE', #27209 ) ;
#25461 = CARTESIAN_POINT ( 'NONE',  ( -1.449479884000000052, -58.34046154589999844, -23.55113706229999693 ) ) ;
#25462 = CARTESIAN_POINT ( 'NONE',  ( 40.00000000000000000, -82.25000000000000000, 0.000000000000000000 ) ) ;
#25463 = FACE_OUTER_BOUND ( 'NONE', #11886, .T. ) ;
#25464 = ORIENTED_EDGE ( 'NONE', *, *, #14417, .F. ) ;
#25465 = CARTESIAN_POINT ( 'NONE',  ( -11.20154639050000078, -94.96739875689999621, -21.25936308859999713 ) ) ;
#25466 = CARTESIAN_POINT ( 'NONE',  ( -0.5335602090290000321, -52.63293862049999916, -23.18581005440000098 ) ) ;
#25467 = CARTESIAN_POINT ( 'NONE',  ( -7.215414233289999757, -74.50000000000000000, -40.70731707320000226 ) ) ;
#25468 = VERTEX_POINT ( 'NONE', #15671 ) ;
#25469 = CARTESIAN_POINT ( 'NONE',  ( 7.398926161578894600, -36.73003209889780152, -21.48136641451177908 ) ) ;
#25470 = CARTESIAN_POINT ( 'NONE',  ( -11.31192030519693326, -60.02098066203591031, 20.72433129729396839 ) ) ;
#25471 = CARTESIAN_POINT ( 'NONE',  ( -2.892691684889999948, -71.70959084179999365, -28.02986260229999971 ) ) ;
#25472 = CARTESIAN_POINT ( 'NONE',  ( -14.72314245780000164, -71.04327856650000683, 23.66650937980000080 ) ) ;
#25473 = VERTEX_POINT ( 'NONE', #7248 ) ;
#25474 = CARTESIAN_POINT ( 'NONE',  ( 36.57652955130000549, -74.41832496969999511, -14.62770612210000110 ) ) ;
#25475 = ADVANCED_FACE ( 'NONE', ( #16113 ), #6808, .F. ) ;
#25476 = MECHANICAL_DESIGN_GEOMETRIC_PRESENTATION_REPRESENTATION (  '', ( #19422 ), #24059 ) ;
#25477 = CARTESIAN_POINT ( 'NONE',  ( -15.86429039329999924, -100.7450341080000129, 3.014304981200000455 ) ) ;
#25478 = CARTESIAN_POINT ( 'NONE',  ( 25.36165982329999835, -58.81334883509999401, 1.380217915539999840 ) ) ;
#25479 = CARTESIAN_POINT ( 'NONE',  ( -6.236885381186699995, -101.3051320416518024, 14.59871265079590863 ) ) ;
#25480 = VERTEX_POINT ( 'NONE', #25015 ) ;
#25481 = DIRECTION ( 'NONE',  ( 0.000000000000000000, 1.000000000000000000, 0.000000000000000000 ) ) ;
#25482 = CARTESIAN_POINT ( 'NONE',  ( -3.561278452559999863, -18.50000000000000000, -23.17450688339999942 ) ) ;
#25483 = CARTESIAN_POINT ( 'NONE',  ( 36.42686065015308827, -74.03769727758323427, -14.02198836895357026 ) ) ;
#25484 = VERTEX_POINT ( 'NONE', #22839 ) ;
#25485 = ADVANCED_FACE ( 'NONE', ( #2292 ), #20204, .T. ) ;
#25486 = CYLINDRICAL_SURFACE ( 'NONE', #27035, 18.64285714289999873 ) ;
#25487 = AXIS2_PLACEMENT_3D ( 'NONE', #9342, #20424, #27285 ) ;
#25488 = FACE_OUTER_BOUND ( 'NONE', #26519, .T. ) ;
#25489 = CARTESIAN_POINT ( 'NONE',  ( 19.98296175649999995, -94.98812477599999227, 14.17692170039999944 ) ) ;
#25490 = ORIENTED_EDGE ( 'NONE', *, *, #20788, .T. ) ;
#25491 = UNCERTAINTY_MEASURE_WITH_UNIT (LENGTH_MEASURE( 1.000000000000000082E-05 ), #18542, 'distance_accuracy_value', 'NONE');
#25492 = B_SPLINE_SURFACE_WITH_KNOTS ( 'NONE', 5, 5, ( 
 ( #11960, #343, #20276, #3108, #15897, #16188, #22918, #20423, #18536 ),
 ( #27429, #20577, #5132, #11665, #27137, #641, #7479, #493, #9490 ),
 ( #13865, #4841, #13720, #9630, #16340, #25249, #7318, #5277, #7179 ),
 ( #2809, #9187, #932, #11819, #14165, #16044, #24948, #22768, #2516 ),
 ( #26845, #24655, #2957, #11372, #791, #18394, #23064, #20873, #9775 ),
 ( #6879, #15744, #4686, #8159, #1480, #12511, #23603, #8021, #7760 ) ),
 .UNSPECIFIED., .F., .F., .F.,
 ( 6, 6 ),
 ( 6, 3, 6 ),
 ( 22.76138574470000009, 41.46675637300000261 ),
 ( 0.000000000000000000, 0.2500000000000000000, 0.5000000000000000000 ),
 .UNSPECIFIED. ) ;
#25493 = CARTESIAN_POINT ( 'NONE',  ( -0.6772741170208298467, -79.75814015466558260, 47.21855544081748945 ) ) ;
#25494 = ORIENTED_EDGE ( 'NONE', *, *, #11467, .F. ) ;
#25495 = AXIS2_PLACEMENT_3D ( 'NONE', #27112, #5394, #469 ) ;
#25496 = EDGE_CURVE ( 'NONE', #3132, #15723, #15646, .T. ) ;
#25497 = CARTESIAN_POINT ( 'NONE',  ( -27.04683438039999999, -74.50000000000000000, -36.23922253580000330 ) ) ;
#25498 = DIRECTION ( 'NONE',  ( 0.7600087925152557711, -0.5000000000001688649, 0.4151946956541399114 ) ) ;
#25499 = ORIENTED_EDGE ( 'NONE', *, *, #16156, .F. ) ;
#25500 = CARTESIAN_POINT ( 'NONE',  ( -12.43025579110000045, -34.65279261700000291, 19.60331251459999891 ) ) ;
#25501 = CARTESIAN_POINT ( 'NONE',  ( -5.733321685880000018, -101.0535396030000044, 14.50026364080000008 ) ) ;
#25502 = EDGE_LOOP ( 'NONE', ( #7839, #19429, #18610, #19293, #26006 ) ) ;
#25503 = FACE_OUTER_BOUND ( 'NONE', #2718, .T. ) ;
#25504 = CARTESIAN_POINT ( 'NONE',  ( 39.45579440730000442, -74.12477399299999092, 7.440489808619999756 ) ) ;
#25505 = DIRECTION ( 'NONE',  ( -0.09756097560976770278, 0.000000000000000000, 0.9952295494196655712 ) ) ;
#25506 = CARTESIAN_POINT ( 'NONE',  ( 18.49452695338690233, -98.73470581664456347, -0.2805694970595983273 ) ) ;
#25507 = CARTESIAN_POINT ( 'NONE',  ( -13.44405788329999929, -68.28990366489999531, 22.97003105929999833 ) ) ;
#25508 = ORIENTED_EDGE ( 'NONE', *, *, #15265, .F. ) ;
#25509 = CARTESIAN_POINT ( 'NONE',  ( -32.50321504749999946, -80.12422352349999244, -22.09864494740000040 ) ) ;
#25510 = EDGE_CURVE ( 'NONE', #6300, #5390, #18780, .T. ) ;
#25511 = CARTESIAN_POINT ( 'NONE',  ( -11.87191034930000022, -15.14308496720000008, -21.73138612759999688 ) ) ;
#25512 = CARTESIAN_POINT ( 'NONE',  ( -20.20541296980000112, -94.98812148390000232, 12.40015329510000086 ) ) ;
#25513 = DIRECTION ( 'NONE',  ( 1.000000000000000000, 0.000000000000000000, 0.000000000000000000 ) ) ;
#25514 = ORIENTED_EDGE ( 'NONE', *, *, #12389, .T. ) ;
#25515 = B_SPLINE_CURVE_WITH_KNOTS ( 'NONE', 5,
 ( #2047, #13537, #18066, #6706, #2335, #15869, #11189, #13692, #24775 ),
 .UNSPECIFIED., .F., .F.,
 ( 6, 3, 6 ),
 ( 0.000000000000000000, 0.5000000000000000000, 1.000000000000000000 ),
 .UNSPECIFIED. ) ;
#25516 = CARTESIAN_POINT ( 'NONE',  ( -2.155284377200000545, -80.29279205369999772, 46.98362450949999669 ) ) ;
#25517 = CARTESIAN_POINT ( 'NONE',  ( 22.35420107259999867, -19.50000000000000000, 9.881343484100000296 ) ) ;
#25518 = ORIENTED_EDGE ( 'NONE', *, *, #8866, .T. ) ;
#25519 = AXIS2_PLACEMENT_3D ( 'NONE', #14351, #14626, #21335 ) ;
#25520 = CARTESIAN_POINT ( 'NONE',  ( -13.09441083470000144, -92.84549618469999643, -23.96915825600000005 ) ) ;
#25521 = FACE_OUTER_BOUND ( 'NONE', #8122, .T. ) ;
#25522 = CARTESIAN_POINT ( 'NONE',  ( -7.931859541086235588, -99.76647888979522349, 15.39525047448377926 ) ) ;
#25523 = CARTESIAN_POINT ( 'NONE',  ( 31.03653123039999784, -73.81134274429999209, -23.56262533510000168 ) ) ;
#25524 = CARTESIAN_POINT ( 'NONE',  ( -14.34881109840844715, -70.26101182088159192, 23.47553979952874670 ) ) ;
#25525 = ADVANCED_BREP_SHAPE_REPRESENTATION ( '', ( #6684, #26433 ), #1786 ) ;
#25526 = CARTESIAN_POINT ( 'NONE',  ( 26.03240350960000171, -67.01088404440000090, -0.1105166297070000053 ) ) ;
#25527 = ORIENTED_EDGE ( 'NONE', *, *, #10785, .T. ) ;
#25528 = EDGE_CURVE ( 'NONE', #2579, #2729, #2066, .T. ) ;
#25529 = CARTESIAN_POINT ( 'NONE',  ( -22.65530694619999963, -72.00000000000000000, 18.22957389299999775 ) ) ;
#25530 = CARTESIAN_POINT ( 'NONE',  ( 19.86285231560000142, -35.99517856170000130, -9.398749189900000189 ) ) ;
#25531 = DIRECTION ( 'NONE',  ( 0.3687499999999814260, 0.000000000000000000, -0.9295286103719527793 ) ) ;
#25532 = ORIENTED_EDGE ( 'NONE', *, *, #19026, .T. ) ;
#25533 = CARTESIAN_POINT ( 'NONE',  ( -13.21936873900000009, -100.9405348700000076, -8.915374923630000836 ) ) ;
#25534 = TOROIDAL_SURFACE ( 'NONE', #3211, 29.91857981989999971, 10.00000000000000000 ) ;
#25535 = DIRECTION ( 'NONE',  ( 1.000000000000000000, 0.000000000000000000, 0.000000000000000000 ) ) ;
#25536 = ORIENTED_EDGE ( 'NONE', *, *, #28273, .T. ) ;
#25537 = DIRECTION ( 'NONE',  ( -1.000000000000000000, 0.000000000000000000, -3.154042683594194627E-16 ) ) ;
#25538 = DIRECTION ( 'NONE',  ( -0.8775825618903722036, 0.000000000000000000, 0.4794255386042041156 ) ) ;
#25539 = EDGE_CURVE ( 'NONE', #22334, #7778, #25596, .T. ) ;
#25540 = CARTESIAN_POINT ( 'NONE',  ( 7.269124901809999706, -101.2512678979999947, 13.34492656639999986 ) ) ;
#25541 = EDGE_LOOP ( 'NONE', ( #13922, #22575, #5579, #24968, #26405, #349 ) ) ;
#25542 = CARTESIAN_POINT ( 'NONE',  ( -43.26282332285115473, -65.11500191527875359, -0.1170746919366537492 ) ) ;
#25543 = CARTESIAN_POINT ( 'NONE',  ( -28.51730836919999845, -92.58502644590001296, -2.516715198190000002 ) ) ;
#25544 = CARTESIAN_POINT ( 'NONE',  ( 10.66329234459999853, -95.90105813160000992, -20.27129911129999940 ) ) ;
#25545 = EDGE_LOOP ( 'NONE', ( #8418, #27826, #18958, #23392, #16663 ) ) ;
#25546 = CARTESIAN_POINT ( 'NONE',  ( -14.01103650240000142, -74.00781516410000904, 36.37014139069999885 ) ) ;
#25547 = B_SPLINE_CURVE_WITH_KNOTS ( 'NONE', 3,
 ( #17047, #27988, #19235, #8161, #1749, #19375 ),
 .UNSPECIFIED., .F., .F.,
 ( 4, 2, 4 ),
 ( 0.000000000000000000, 0.5000000000000000000, 1.000000000000000000 ),
 .UNSPECIFIED. ) ;
#25548 = CARTESIAN_POINT ( 'NONE',  ( -42.75000000000000000, -65.00000000000000000, 1.587713240270000048 ) ) ;
#25549 = DIRECTION ( 'NONE',  ( 0.000000000000000000, -1.000000000000000000, 0.000000000000000000 ) ) ;
#25550 = PLANE ( 'NONE',  #16814 ) ;
#25551 = FACE_OUTER_BOUND ( 'NONE', #26670, .T. ) ;
#25552 = B_SPLINE_CURVE_WITH_KNOTS ( 'NONE', 5,
 ( #12509, #19505, #5828, #21418, #15111, #1477 ),
 .UNSPECIFIED., .F., .F.,
 ( 6, 6 ),
 ( -46.77973719450000090, 0.000000000000000000 ),
 .UNSPECIFIED. ) ;
#25553 = VECTOR ( 'NONE', #10354, 1000.000000000000000 ) ;
#25554 = CARTESIAN_POINT ( 'NONE',  ( 40.00000000000000000, -74.00000000000000000, 1.960630394010000073E-15 ) ) ;
#25555 = CARTESIAN_POINT ( 'NONE',  ( -38.55000000000000426, -65.14977478849999670, -2.857883832489999776 ) ) ;
#25556 = CARTESIAN_POINT ( 'NONE',  ( -38.96762186407187301, -74.02518375728683964, -7.561767224770083118 ) ) ;
#25557 = CARTESIAN_POINT ( 'NONE',  ( -11.29865404370000093, -27.06785567070000198, -19.22788970119999874 ) ) ;
#25558 = EDGE_LOOP ( 'NONE', ( #27664, #7200, #23011, #8553 ) ) ;
#25559 = AXIS2_PLACEMENT_3D ( 'NONE', #25447, #26294, #12574 ) ;
#25560 = AXIS2_PLACEMENT_3D ( 'NONE', #14372, #10390, #14503 ) ;
#25561 = AXIS2_PLACEMENT_3D ( 'NONE', #10906, #8305, #26250 ) ;
#25562 = CARTESIAN_POINT ( 'NONE',  ( 6.852899841210000176, -101.1617736559999940, 14.17211744369999948 ) ) ;
#25563 = CARTESIAN_POINT ( 'NONE',  ( 13.64609657498295370, -96.57210918286925505, -16.84344588869538839 ) ) ;
#25564 = AXIS2_PLACEMENT_3D ( 'NONE', #11804, #3228, #20716 ) ;
#25565 = CARTESIAN_POINT ( 'NONE',  ( 7.318052426040000391, -101.1822553929999913, 13.41977313900000013 ) ) ;
#25566 = CARTESIAN_POINT ( 'NONE',  ( -11.25330392600000096, -94.84395216780001192, -20.59896425910000062 ) ) ;
#25567 = CARTESIAN_POINT ( 'NONE',  ( 7.356932666920000585, -36.56810636680000215, -21.47791282949999925 ) ) ;
#25568 = DIRECTION ( 'NONE',  ( 0.000000000000000000, 1.000000000000000000, 0.000000000000000000 ) ) ;
#25569 = B_SPLINE_CURVE_WITH_KNOTS ( 'NONE', 3,
 ( #3488, #14545, #27818, #19073, #14952, #23859, #25633, #28365, #5803, #23718, #3899, #23577, #8132, #16740, #5931, #3622, #5665, #19204, #19349, #17156, #12348, #10022, #21258, #1310, #21394, #10154, #12623, #8395, #16886, #15090, #28092, #26045, #17018, #7995, #27955, #25906, #1450, #21535, #6071, #26197, #12762, #21672, #1723, #6224, #3352, #17243, #15169, #28304, #24079, #4117, #8622, #17387, #19707, #17529, #17676, #28452, #1671, #3839, #10647 ),
 .UNSPECIFIED., .F., .F.,
 ( 4, 2, 1, 1, 2, 2, 2, 1, 1, 1, 2, 2, 2, 2, 2, 2, 2, 1, 1, 2, 2, 2, 2, 1, 2, 2, 2, 1, 2, 2, 2, 2, 2, 4 ),
 ( 0.000000000000000000, 0.06250000000013401780, 0.09375000000019519109, 0.1093750000002202127, 0.1171875000002372408, 0.1250000000002542688, 0.1875000000004052869, 0.2187500000004812262, 0.2343750000005198064, 0.2421875000005390965, 0.2460937500005491718, 0.2500000000005592748, 0.3125000000005516698, 0.3437500000005482281, 0.3750000000005447864, 0.4375000000005389578, 0.4687500000005295764, 0.4843750000005255796, 0.4921875000005235812, 0.4960937500005233591, 0.5000000000005231371, 0.5625000000004112266, 0.5937500000003553824, 0.6093750000003334000, 0.6171875000003288481, 0.6250000000003242961, 0.6875000000002615685, 0.7187500000002239320, 0.7343750000002052802, 0.7500000000001865175, 0.8125000000001336709, 0.8437500000001117995, 0.8750000000000900391, 1.000000000000000000 ),
 .UNSPECIFIED. ) ;
#25570 = CARTESIAN_POINT ( 'NONE',  ( 26.68170793902356763, -93.00000166546708158, -11.33666327679907049 ) ) ;
#25571 = ADVANCED_FACE ( 'NONE', ( #12026 ), #5487, .F. ) ;
#25572 = DIRECTION ( 'NONE',  ( 0.000000000000000000, 1.000000000000000000, 0.000000000000000000 ) ) ;
#25573 = EDGE_CURVE ( 'NONE', #7860, #13129, #18363, .T. ) ;
#25574 = LINE ( 'NONE', #23385, #8415 ) ;
#25575 = ORIENTED_EDGE ( 'NONE', *, *, #4032, .T. ) ;
#25576 = AXIS2_PLACEMENT_3D ( 'NONE', #18391, #16875, #9771 ) ;
#25577 = CARTESIAN_POINT ( 'NONE',  ( -1.800056393709054570, -69.76823740066200230, -27.23143567540053311 ) ) ;
#25578 = CARTESIAN_POINT ( 'NONE',  ( -12.69354235982726742, -63.63799308303316593, -20.95011642351082415 ) ) ;
#25579 = ORIENTED_EDGE ( 'NONE', *, *, #24810, .F. ) ;
#25580 = ADVANCED_FACE ( 'NONE', ( #12173 ), #15511, .F. ) ;
#25581 = DIRECTION ( 'NONE',  ( -1.000000000000000000, 0.000000000000000000, 0.000000000000000000 ) ) ;
#25582 = EDGE_CURVE ( 'NONE', #19131, #13461, #3038, .T. ) ;
#25583 = AXIS2_PLACEMENT_3D ( 'NONE', #11273, #28337, #10679 ) ;
#25584 = AXIS2_PLACEMENT_3D ( 'NONE', #7310, #13855, #7169 ) ;
#25585 = CARTESIAN_POINT ( 'NONE',  ( 0.5752469741175000317, -100.9229461903683926, -16.55552124226701594 ) ) ;
#25586 = B_SPLINE_CURVE_WITH_KNOTS ( 'NONE', 3,
 ( #17257, #12722, #8221, #17113, #8356, #26156, #25870, #5895, #12439, #3579, #19307, #6028, #21775, #6325, #15052, #3996, #23818, #21635, #25730, #1826, #16982, #21351, #28189, #28470, #12857, #26303, #4138, #10669, #19582, #5760, #24101, #3861, #16841, #8508 ),
 .UNSPECIFIED., .F., .F.,
 ( 4, 2, 2, 2, 1, 1, 2, 2, 2, 2, 1, 1, 2, 2, 2, 2, 2, 2, 4 ),
 ( 0.000000000000000000, 0.1249999999999426292, 0.1874999999999139300, 0.2187499999998982481, 0.2343749999998903932, 0.2421874999998879785, 0.2460937499998875622, 0.2499999999998871458, 0.3749999999999151234, 0.4374999999999292233, 0.4687499999999348299, 0.4843749999999376610, 0.4921874999999391598, 0.4999999999999406031, 0.6249999999999575895, 0.6874999999999661382, 0.7187499999999695799, 0.7499999999999729106, 1.000000000000000000 ),
 .UNSPECIFIED. ) ;
#25587 = DIRECTION ( 'NONE',  ( -0.9950133697301837277, 0.000000000000000000, 0.09974163653251839901 ) ) ;
#25588 = CARTESIAN_POINT ( 'NONE',  ( 13.40137751648780373, -92.68577957619636720, 27.39809740741056743 ) ) ;
#25589 = CARTESIAN_POINT ( 'NONE',  ( -11.69653564380000077, -94.52419443349998573, -20.97821456950000041 ) ) ;
#25590 = CARTESIAN_POINT ( 'NONE',  ( 20.34158267359999783, -73.93832881409998947, -32.34203349919999937 ) ) ;
#25591 = DIRECTION ( 'NONE',  ( -0.4151946956541399669, 0.5000000000001689759, -0.7600087925152558821 ) ) ;
#25592 = CARTESIAN_POINT ( 'NONE',  ( -18.26050467580000003, -97.41004717059999507, 11.26842931770000078 ) ) ;
#25593 = CARTESIAN_POINT ( 'NONE',  ( 22.66360738736820579, -92.65509297698689295, 15.93307463348966202 ) ) ;
#25594 = CARTESIAN_POINT ( 'NONE',  ( 4.656214649959999954E-15, -79.00000000000000000, 40.00000000000000000 ) ) ;
#25595 = DIRECTION ( 'NONE',  ( -0.7071067811865475727, 0.000000000000000000, 0.7071067811865475727 ) ) ;
#25596 = LINE ( 'NONE', #14086, #13688 ) ;
#25597 = ORIENTED_EDGE ( 'NONE', *, *, #3582, .F. ) ;
#25598 = CARTESIAN_POINT ( 'NONE',  ( -41.45000000000000284, -65.14977478849999670, 2.857883832489999776 ) ) ;
#25599 = VERTEX_POINT ( 'NONE', #14648 ) ;
#25600 = TOROIDAL_SURFACE ( 'NONE', #12999, 7.750000000000000000, 0.5000000000000000000 ) ;
#25601 = AXIS2_PLACEMENT_3D ( 'NONE', #26801, #19926, #22425 ) ;
#25602 = DIRECTION ( 'NONE',  ( -0.09756097560976716154, 0.000000000000000000, -0.9952295494196655712 ) ) ;
#25603 = B_SPLINE_CURVE_WITH_KNOTS ( 'NONE', 3,
 ( #10493, #28023, #19408, #14744, #23516, #21738 ),
 .UNSPECIFIED., .F., .F.,
 ( 4, 2, 4 ),
 ( 0.000000000000000000, 0.5000000000000000000, 1.000000000000000000 ),
 .UNSPECIFIED. ) ;
#25604 = DIRECTION ( 'NONE',  ( -0.8775825618903722036, 0.000000000000000000, 0.4794255386042041156 ) ) ;
#25605 = CARTESIAN_POINT ( 'NONE',  ( 20.01429421219999938, -35.44265673480000345, -8.963580811669999093 ) ) ;
#25606 = EDGE_CURVE ( 'NONE', #25473, #10539, #15262, .T. ) ;
#25607 = B_SPLINE_CURVE_WITH_KNOTS ( 'NONE', 3,
 ( #19679, #5854, #21874, #28568, #15284, #24206, #13114, #10348, #10912, #22025, #8183, #14735, #17069, #2073, #25831, #25963, #14866, #5987, #13560, #2658, #9331, #4971, #8886, #16037, #28697, #26535, #27132, #9038, #6579, #19967, #11213, #7022 ),
 .UNSPECIFIED., .F., .F.,
 ( 4, 2, 1, 1, 1, 2, 2, 2, 1, 1, 1, 2, 2, 2, 1, 1, 1, 1, 2, 2, 4 ),
 ( 0.000000000000000000, 0.1250000000001095235, 0.1875000000001643408, 0.2187500000001895428, 0.2343750000002022271, 0.2421875000002085554, 0.2500000000002148837, 0.3750000000003662071, 0.4375000000004459211, 0.4687500000004778400, 0.4843750000004859446, 0.4921875000004900524, 0.5000000000004941603, 0.6250000000006031842, 0.6875000000006669110, 0.7187500000007002177, 0.7343750000007220891, 0.7421875000007379652, 0.7460937500007444045, 0.7500000000007508438, 1.000000000000000000 ),
 .UNSPECIFIED. ) ;
#25608 = ORIENTED_EDGE ( 'NONE', *, *, #4342, .F. ) ;
#25609 = DIRECTION ( 'NONE',  ( 0.000000000000000000, 0.000000000000000000, 1.000000000000000000 ) ) ;
#25610 = VERTEX_POINT ( 'NONE', #23266 ) ;
#25611 = CARTESIAN_POINT ( 'NONE',  ( -1.315109685649999971, -92.50000000000000000, -30.47163412939999816 ) ) ;
#25612 = CARTESIAN_POINT ( 'NONE',  ( 40.65508461000000295, -79.00000000000000000, -13.75000000000000000 ) ) ;
#25613 = ADVANCED_FACE ( 'NONE', ( #9566 ), #17887, .T. ) ;
#25614 = CARTESIAN_POINT ( 'NONE',  ( -41.75000000000000000, -65.17124718639999514, 2.640283750780000105 ) ) ;
#25615 = AXIS2_PLACEMENT_3D ( 'NONE', #13630, #24862, #4896 ) ;
#25616 = CARTESIAN_POINT ( 'NONE',  ( -22.09417056399443169, -74.04315698458545114, -32.28351515837096741 ) ) ;
#25617 = ORIENTED_EDGE ( 'NONE', *, *, #13509, .F. ) ;
#25618 = TOROIDAL_SURFACE ( 'NONE', #15341, 0.5000000000000000000, 0.5000000000000000000 ) ;
#25619 = CARTESIAN_POINT ( 'NONE',  ( -15.42268928930000094, -101.5369814700000148, 4.259183639510000674 ) ) ;
#25620 = CARTESIAN_POINT ( 'NONE',  ( -16.03654356910000089, -101.2023582690000012, 3.165913905190000044 ) ) ;
#25621 = CARTESIAN_POINT ( 'NONE',  ( 23.97433208980000074, -62.13475808409999956, -0.5610825628509999996 ) ) ;
#25622 = CARTESIAN_POINT ( 'NONE',  ( -20.78736624049999904, -63.14819481680000735, 14.88907486529999957 ) ) ;
#25623 = ORIENTED_EDGE ( 'NONE', *, *, #14628, .F. ) ;
#25624 = DIRECTION ( 'NONE',  ( 1.000000000000000000, 0.000000000000000000, 0.000000000000000000 ) ) ;
#25625 = CARTESIAN_POINT ( 'NONE',  ( -3.338365958889999874, -18.50000000000000000, -23.63904113259999917 ) ) ;
#25626 = CARTESIAN_POINT ( 'NONE',  ( 36.73433531666305640, -74.37420903145732609, -14.53002935066677459 ) ) ;
#25627 = ORIENTED_EDGE ( 'NONE', *, *, #1880, .F. ) ;
#25628 = DIRECTION ( 'NONE',  ( 0.4794255386042036715, 0.000000000000000000, 0.8775825618903724257 ) ) ;
#25629 = CARTESIAN_POINT ( 'NONE',  ( 36.93547111259999838, -80.07278442950000397, -13.78755837009999929 ) ) ;
#25630 = CARTESIAN_POINT ( 'NONE',  ( 36.71193690820000199, -74.86352340930001503, -14.74418008200000152 ) ) ;
#25631 = ORIENTED_EDGE ( 'NONE', *, *, #23078, .T. ) ;
#25632 = EDGE_CURVE ( 'NONE', #25958, #12242, #23029, .T. ) ;
#25633 = CARTESIAN_POINT ( 'NONE',  ( 6.990562848071419033, -100.1406256088127122, 15.70413603688146331 ) ) ;
#25634 = TOROIDAL_SURFACE ( 'NONE', #1900, 55.85192378860000417, 0.3499999999999999778 ) ;
#25635 = CARTESIAN_POINT ( 'NONE',  ( -0.8967168713914961398, -79.84002594721414425, 47.19433117586794424 ) ) ;
#25636 = CIRCLE ( 'NONE', #10258, 1.999999999999997558 ) ;
#25637 = VERTEX_POINT ( 'NONE', #21088 ) ;
#25638 = EDGE_CURVE ( 'NONE', #8854, #10427, #20212, .T. ) ;
#25639 = VECTOR ( 'NONE', #13681, 999.9999999999998863 ) ;
#25640 = CARTESIAN_POINT ( 'NONE',  ( -18.29385458159615396, -98.30143183942811902, 5.155709219538591626 ) ) ;
#25641 = ORIENTED_EDGE ( 'NONE', *, *, #22719, .T. ) ;
#25642 = CARTESIAN_POINT ( 'NONE',  ( 28.55300759750000239, -92.83702889490000132, 8.518421555419999791 ) ) ;
#25643 = CARTESIAN_POINT ( 'NONE',  ( -6.181362597580000617, -101.1716782170000073, 14.46875015949999899 ) ) ;
#25644 = VERTEX_POINT ( 'NONE', #3580 ) ;
#25645 = CARTESIAN_POINT ( 'NONE',  ( -41.96540734349659374, -63.35496135697054854, 0.9466671610960367689 ) ) ;
#25646 = EDGE_CURVE ( 'NONE', #5424, #17168, #7210, .T. ) ;
#25647 = DIRECTION ( 'NONE',  ( 0.000000000000000000, 0.000000000000000000, 1.000000000000000000 ) ) ;
#25648 = CARTESIAN_POINT ( 'NONE',  ( 23.54313657600000198, -94.98812477599999227, -6.784142512209999865 ) ) ;
#25649 = CARTESIAN_POINT ( 'NONE',  ( -43.07153896660000214, -69.50000000000000000, -1.677989385109999843 ) ) ;
#25650 = CARTESIAN_POINT ( 'NONE',  ( 47.04106180647456625, -79.61201027780809625, -2.182424667423416675 ) ) ;
#25651 = VERTEX_POINT ( 'NONE', #18615 ) ;
#25652 = DIRECTION ( 'NONE',  ( 0.000000000000000000, 1.000000000000000000, 0.000000000000000000 ) ) ;
#25653 = CARTESIAN_POINT ( 'NONE',  ( 19.84870995880000066, -97.83383802310000021, 2.182632968150000075 ) ) ;
#25654 = CARTESIAN_POINT ( 'NONE',  ( -20.80195327079999856, -93.01591283300000157, 16.29683310170000254 ) ) ;
#25655 = DIRECTION ( 'NONE',  ( 0.000000000000000000, -1.000000000000000000, 0.000000000000000000 ) ) ;
#25656 = CARTESIAN_POINT ( 'NONE',  ( -2.358001274529999858, -55.01779585689999408, -24.27108329320000024 ) ) ;
#25657 = CIRCLE ( 'NONE', #2872, 3.499999999999999556 ) ;
#25658 = CARTESIAN_POINT ( 'NONE',  ( -2.679185798610000444E-13, -79.50000000000000000, 47.25000000000000000 ) ) ;
#25659 = CARTESIAN_POINT ( 'NONE',  ( -37.60355029590000697, -84.50000000000000000, -9.356041104380000917 ) ) ;
#25660 = ORIENTED_EDGE ( 'NONE', *, *, #24061, .T. ) ;
#25661 = AXIS2_PLACEMENT_3D ( 'NONE', #3217, #23721, #28226 ) ;
#25662 = CYLINDRICAL_SURFACE ( 'NONE', #1584, 34.89999999999999858 ) ;
#25663 = AXIS2_PLACEMENT_3D ( 'NONE', #23956, #24384, #4424 ) ;
#25664 = CARTESIAN_POINT ( 'NONE',  ( 0.000000000000000000, -15.49681045920000066, 0.000000000000000000 ) ) ;
#25665 = DIRECTION ( 'NONE',  ( 0.8172561201429201505, 0.000000000000000000, 0.5762746169049446365 ) ) ;
#25666 = CARTESIAN_POINT ( 'NONE',  ( -38.08919256720000135, -65.74290439030001210, 1.043878858160000034 ) ) ;
#25667 = CARTESIAN_POINT ( 'NONE',  ( -14.15696331435236033, -74.02271853708172955, 36.23139294035578217 ) ) ;
#25668 = B_SPLINE_SURFACE_WITH_KNOTS ( 'NONE', 5, 5, ( 
 ( #16535, #27326, #22812, #27627, #9958, #25567 ),
 ( #16088, #20628, #25433, #20776, #14214, #3288 ),
 ( #686, #5601, #5176, #5023, #16231, #25143 ),
 ( #14058, #3007, #3145, #23381, #14622, #3560 ),
 ( #1251, #19417, #19555, #24073, #12415, #23524 ),
 ( #28298, #23799, #5740, #10090, #19007, #8202 ) ),
 .UNSPECIFIED., .F., .F., .F.,
 ( 6, 6 ),
 ( 6, 6 ),
 ( 1.600842967049999954, 3.163651481680000099 ),
 ( 0.000000000000000000, 2.000000000000000000 ),
 .UNSPECIFIED. ) ;
#25669 =( LENGTH_UNIT ( ) NAMED_UNIT ( * ) SI_UNIT ( .MILLI., .METRE. ) );
#25670 = MANIFOLD_SOLID_BREP ( 'Rotational Bodies', #17472 ) ;
#25672 = ORIENTED_EDGE ( 'NONE', *, *, #47, .F. ) ;
#25671 = ADVANCED_FACE ( 'NONE', ( #28190 ), #8256, .T. ) ;
#25673 = EDGE_CURVE ( 'NONE', #18774, #24426, #11461, .T. ) ;
#25674 = CARTESIAN_POINT ( 'NONE',  ( 21.15739348700000377, -35.90623960370000134, -8.363368093209999188 ) ) ;
#25675 = CARTESIAN_POINT ( 'NONE',  ( 19.92559242949999998, -35.99861502429999405, -9.426072644010000445 ) ) ;
#25676 = CARTESIAN_POINT ( 'NONE',  ( 7.120468124967428203, -92.55389105865127419, -28.82010846582078045 ) ) ;
#25677 = ORIENTED_EDGE ( 'NONE', *, *, #21253, .T. ) ;
#25678 = EDGE_CURVE ( 'NONE', #26457, #6032, #8569, .T. ) ;
#25679 = AXIS2_PLACEMENT_3D ( 'NONE', #10584, #15251, #24172 ) ;
#25680 = CARTESIAN_POINT ( 'NONE',  ( -13.25127150620000016, -101.2490009469999990, -9.112328469719999546 ) ) ;
#25681 = VECTOR ( 'NONE', #20687, 999.9999999999998863 ) ;
#25682 = CARTESIAN_POINT ( 'NONE',  ( -7.876988035330001026, -100.4071172650000108, 14.82857468579999960 ) ) ;
#25683 = VERTEX_POINT ( 'NONE', #18131 ) ;
#25684 = CARTESIAN_POINT ( 'NONE',  ( -1.283017171710000071, -101.3150694429999987, -16.20107591070000197 ) ) ;
#25685 = CARTESIAN_POINT ( 'NONE',  ( 26.69293917519999937, -30.50310889129999836, 48.86109741659999628 ) ) ;
#25686 = CARTESIAN_POINT ( 'NONE',  ( 7.602022623930000833, -101.5367116919999972, 14.07888202740000239 ) ) ;
#25687 = ORIENTED_EDGE ( 'NONE', *, *, #12420, .T. ) ;
#25688 = DIRECTION ( 'NONE',  ( 1.000000000000000000, 0.000000000000000000, 0.000000000000000000 ) ) ;
#25689 = CARTESIAN_POINT ( 'NONE',  ( -29.91145159459999903, -92.50000467790000869, -0.6532164815390000268 ) ) ;
#25690 = CARTESIAN_POINT ( 'NONE',  ( 26.68243298039999800, -70.99734270939998737, 10.68791969299999955 ) ) ;
#25691 = CARTESIAN_POINT ( 'NONE',  ( 11.33780749240000141, -100.8733984769999950, -10.89600342719999837 ) ) ;
#25692 = ORIENTED_EDGE ( 'NONE', *, *, #14208, .F. ) ;
#25693 = CARTESIAN_POINT ( 'NONE',  ( 19.88144391770000041, -18.50000000000000000, -7.765653790140000012 ) ) ;
#25694 = CARTESIAN_POINT ( 'NONE',  ( 11.58372824880000174, -101.1292389529999980, -10.30936447240000042 ) ) ;
#25695 = CARTESIAN_POINT ( 'NONE',  ( -14.38874196869999977, -74.12911414260001663, 36.70801399449999991 ) ) ;
#25696 = CARTESIAN_POINT ( 'NONE',  ( -17.78957887869999865, -94.03833868319999567, 17.10921786280000134 ) ) ;
#25697 = CARTESIAN_POINT ( 'NONE',  ( -18.23251993885847710, -92.52498922770502077, 24.45057987636252150 ) ) ;
#25698 = ORIENTED_EDGE ( 'NONE', *, *, #3312, .F. ) ;
#25699 = CARTESIAN_POINT ( 'NONE',  ( -24.21840725559999896, -74.50000000000000000, -34.11790219230000076 ) ) ;
#25700 = EDGE_CURVE ( 'NONE', #27727, #15327, #4875, .T. ) ;
#25701 = FACE_OUTER_BOUND ( 'NONE', #25121, .T. ) ;
#25702 = CARTESIAN_POINT ( 'NONE',  ( 34.06016921999999880, -74.00000000000000000, -9.364021409339999380 ) ) ;
#25703 = CARTESIAN_POINT ( 'NONE',  ( 7.135467304789999687, -73.50000064450000536, -38.71640881029999548 ) ) ;
#25704 = CARTESIAN_POINT ( 'NONE',  ( 21.30374392919999949, -60.30889230620000063, 10.62872870579999862 ) ) ;
#25705 = DIRECTION ( 'NONE',  ( -0.2414462220490755096, 0.000000000000000000, 0.9704142011833032377 ) ) ;
#25706 = CIRCLE ( 'NONE', #16853, 22.03370205219999889 ) ;
#25707 = ORIENTED_EDGE ( 'NONE', *, *, #19693, .T. ) ;
#25708 = CARTESIAN_POINT ( 'NONE',  ( 6.745190077079999291, -100.5229262450000078, 15.47590599200000128 ) ) ;
#25709 = CARTESIAN_POINT ( 'NONE',  ( 13.81100091409999919, -99.92967571559999840, -10.51865105429999936 ) ) ;
#25710 = CARTESIAN_POINT ( 'NONE',  ( -11.46795327739999948, -94.84072973010000851, -21.30482454299999873 ) ) ;
#25711 = DIRECTION ( 'NONE',  ( 1.000000000000000000, 0.000000000000000000, 0.000000000000000000 ) ) ;
#25712 = CARTESIAN_POINT ( 'NONE',  ( 23.14416696340000001, -57.40875702419999982, 10.37855830930000067 ) ) ;
#25713 = FACE_OUTER_BOUND ( 'NONE', #2479, .T. ) ;
#25714 = CARTESIAN_POINT ( 'NONE',  ( -6.439729480049999566, -101.2530993010000060, 13.76171823350000167 ) ) ;
#25715 = B_SPLINE_CURVE_WITH_KNOTS ( 'NONE', 3,
 ( #6617, #26432, #15476, #12851, #8500, #10809, #6768, #15629, #24528, #13444, #24387, #15326, #22201, #6318, #4565, #26730, #26147, #19854, #2245, #2113, #28463, #8635, #10946, #20006, #22352, #19719, #28605, #17542, #24243, #4279 ),
 .UNSPECIFIED., .F., .F.,
 ( 4, 1, 1, 1, 1, 2, 2, 1, 1, 1, 1, 2, 2, 2, 1, 1, 1, 1, 2, 2, 4 ),
 ( 0.000000000000000000, 0.1249999999999575895, 0.1874999999999370504, 0.2187499999999273637, 0.2343749999999251155, 0.2421874999999223954, 0.2499999999999197309, 0.3749999999998104294, 0.4374999999997585820, 0.4687499999997326583, 0.4843749999997227218, 0.4921874999997177258, 0.4999999999997127298, 0.6249999999996563860, 0.6874999999996247446, 0.7187499999996056488, 0.7343749999995959898, 0.7421874999995905497, 0.7460937499995909938, 0.7499999999995914379, 1.000000000000000000 ),
 .UNSPECIFIED. ) ;
#25716 = ORIENTED_EDGE ( 'NONE', *, *, #8198, .F. ) ;
#25717 = CIRCLE ( 'NONE', #8027, 2.000000000000000000 ) ;
#25718 = CARTESIAN_POINT ( 'NONE',  ( -5.360408304419999936, -101.0356131030000029, 14.51726283890000069 ) ) ;
#25719 = DIRECTION ( 'NONE',  ( 1.000000000000000000, 0.000000000000000000, 0.000000000000000000 ) ) ;
#25720 = ORIENTED_EDGE ( 'NONE', *, *, #15323, .F. ) ;
#25721 = CIRCLE ( 'NONE', #13126, 30.50381168839999901 ) ;
#25722 = CARTESIAN_POINT ( 'NONE',  ( 0.5820789627235478658, -100.8945630385067176, -16.57764313316371130 ) ) ;
#25723 = DIRECTION ( 'NONE',  ( 0.000000000000000000, -1.000000000000000000, 0.000000000000000000 ) ) ;
#25724 = CARTESIAN_POINT ( 'NONE',  ( 13.30333552573421940, -92.74292563041898063, 27.44579556150942423 ) ) ;
#25725 = CYLINDRICAL_SURFACE ( 'NONE', #20432, 7.249999999999999112 ) ;
#25726 = CARTESIAN_POINT ( 'NONE',  ( -8.303419408699999948, -99.91102932029998840, 14.75134094139999874 ) ) ;
#25727 = PRODUCT_DEFINITION_SHAPE ( 'NONE', 'NONE',  #28805 ) ;
#25728 = EDGE_CURVE ( 'NONE', #18453, #7330, #26273, .T. ) ;
#25729 = CARTESIAN_POINT ( 'NONE',  ( 11.86104588439999930, -101.2306315440000049, -11.05401200120000027 ) ) ;
#25730 = CARTESIAN_POINT ( 'NONE',  ( -18.62649937282418833, -19.47440675035247537, 13.29909953111004661 ) ) ;
#25731 = SPHERICAL_SURFACE ( 'NONE', #7712, 2.000000494509999616 ) ;
#25732 = CARTESIAN_POINT ( 'NONE',  ( 0.000000000000000000, -91.50000000000000000, 0.000000000000000000 ) ) ;
#25733 = ORIENTED_EDGE ( 'NONE', *, *, #16324, .T. ) ;
#25734 = EDGE_CURVE ( 'NONE', #6019, #5317, #11358, .T. ) ;
#25735 = CARTESIAN_POINT ( 'NONE',  ( -10.76213870606590106, -31.71488124271929010, 19.71543491739382148 ) ) ;
#25736 = AXIS2_PLACEMENT_3D ( 'NONE', #24962, #16506, #16639 ) ;
#25737 = ORIENTED_EDGE ( 'NONE', *, *, #503, .T. ) ;
#25738 = EDGE_CURVE ( 'NONE', #6357, #20759, #26880, .T. ) ;
#25739 = TOROIDAL_SURFACE ( 'NONE', #2491, 19.50000000000000000, 3.000000000000000000 ) ;
#25740 = EDGE_CURVE ( 'NONE', #22807, #14760, #12741, .T. ) ;
#25741 = ORIENTED_EDGE ( 'NONE', *, *, #8241, .T. ) ;
#25742 = CARTESIAN_POINT ( 'NONE',  ( -0.8576412294919999457, -60.34598855900000558, -23.61251632689999980 ) ) ;
#25743 = CARTESIAN_POINT ( 'NONE',  ( 11.17657069110000023, -36.00000000000000000, -21.93565779399999727 ) ) ;
#25744 = LINE ( 'NONE', #5633, #3251 ) ;
#25745 = CARTESIAN_POINT ( 'NONE',  ( 5.813199663199999812, -6.776234273679999198, 10.64099060729999913 ) ) ;
#25746 = CARTESIAN_POINT ( 'NONE',  ( 19.90742232022705593, -19.48077950575742534, -8.670048025615079368 ) ) ;
#25747 = ORIENTED_EDGE ( 'NONE', *, *, #12503, .F. ) ;
#25748 = AXIS2_PLACEMENT_3D ( 'NONE', #18540, #18096, #4982 ) ;
#25749 = FACE_OUTER_BOUND ( 'NONE', #960, .T. ) ;
#25750 = ORIENTED_EDGE ( 'NONE', *, *, #14580, .F. ) ;
#25751 = CARTESIAN_POINT ( 'NONE',  ( -40.50000000000000000, -63.30468293320000583, 2.309401076760000393 ) ) ;
#25752 = CARTESIAN_POINT ( 'NONE',  ( 8.611797725689999794, -36.09912295260000548, -20.95164070679999924 ) ) ;
#25753 = CIRCLE ( 'NONE', #18782, 57.75000000000000000 ) ;
#25754 = CARTESIAN_POINT ( 'NONE',  ( -17.66077618279999939, -18.50000000000000000, 11.53219880630000205 ) ) ;
#25755 = ORIENTED_EDGE ( 'NONE', *, *, #23432, .T. ) ;
#25756 = CARTESIAN_POINT ( 'NONE',  ( -15.29387583709999809, -101.2458775890000027, 4.542988961549999871 ) ) ;
#25757 = CARTESIAN_POINT ( 'NONE',  ( -16.40085562500000194, -100.7638431670000045, 3.096686113970000154 ) ) ;
#25758 = CARTESIAN_POINT ( 'NONE',  ( 24.42476877459999685, -57.44036991850000362, 1.191907264949999989 ) ) ;
#25759 = CARTESIAN_POINT ( 'NONE',  ( -6.208760515565253435, -101.2404586421421158, 14.53288061996913783 ) ) ;
#25760 = ORIENTED_EDGE ( 'NONE', *, *, #11854, .T. ) ;
#25761 = CARTESIAN_POINT ( 'NONE',  ( 16.08037959500000014, -101.3150700380000018, 2.354223078750000031 ) ) ;
#25762 = LINE ( 'NONE', #5791, #10630 ) ;
#25763 = EDGE_CURVE ( 'NONE', #23842, #25778, #3485, .T. ) ;
#25764 = CARTESIAN_POINT ( 'NONE',  ( -2.714023266239999899, -18.86472494550000079, -23.42183169720000180 ) ) ;
#25765 = CARTESIAN_POINT ( 'NONE',  ( -7.511256938544575767, -101.2021794472616989, 14.51835494349533207 ) ) ;
#25766 = VERTEX_POINT ( 'NONE', #20015 ) ;
#25767 = ADVANCED_FACE ( 'NONE', ( #530 ), #2557, .T. ) ;
#25768 = CIRCLE ( 'NONE', #24834, 7.750000000000000000 ) ;
#25769 = CARTESIAN_POINT ( 'NONE',  ( -41.47847536571098459, -65.13491442162823830, -2.872258511071608567 ) ) ;
#25770 = CARTESIAN_POINT ( 'NONE',  ( 21.79230230059999940, -37.95144147500000287, -8.472395268590000583 ) ) ;
#25771 = CARTESIAN_POINT ( 'NONE',  ( 7.472970580910000216, -74.00000000000000000, 38.65569705749999940 ) ) ;
#25772 = VERTEX_POINT ( 'NONE', #24692 ) ;
#25773 = EDGE_CURVE ( 'NONE', #10772, #4529, #3147, .T. ) ;
#25774 = ADVANCED_FACE ( 'NONE', ( #15488 ), #12306, .T. ) ;
#25775 = CARTESIAN_POINT ( 'NONE',  ( -7.879410208250000380, -111.0000000000000000, 15.46934584979999983 ) ) ;
#25776 = VECTOR ( 'NONE', #22128, 1000.000000000000000 ) ;
#25777 = CARTESIAN_POINT ( 'NONE',  ( -0.3844954875762284785, -79.64723206074855000, 47.24135775273278171 ) ) ;
#25778 = VERTEX_POINT ( 'NONE', #22210 ) ;
#25779 = CARTESIAN_POINT ( 'NONE',  ( -36.05087847149999902, -63.00000000000000000, 2.157414923720000210 ) ) ;
#25780 = CARTESIAN_POINT ( 'NONE',  ( -40.87758256189999884, -66.42264973080000345, -0.4794255386039999456 ) ) ;
#25781 = ORIENTED_EDGE ( 'NONE', *, *, #6174, .T. ) ;
#25782 = CARTESIAN_POINT ( 'NONE',  ( 20.84246830320000043, -57.47571038090000428, 10.69856926729999991 ) ) ;
#25783 = FACE_OUTER_BOUND ( 'NONE', #8649, .T. ) ;
#25784 = ORIENTED_EDGE ( 'NONE', *, *, #5181, .F. ) ;
#25785 = CARTESIAN_POINT ( 'NONE',  ( 11.86373224459999776, -101.2530993010000060, -9.493548918760000177 ) ) ;
#25786 = CARTESIAN_POINT ( 'NONE',  ( 47.25000000000000000, -75.00000000000000000, -1.245115460929999944E-12 ) ) ;
#25787 = VECTOR ( 'NONE', #24768, 1000.000000000000000 ) ;
#25788 = AXIS2_PLACEMENT_3D ( 'NONE', #26962, #25060, #11481 ) ;
#25789 = CARTESIAN_POINT ( 'NONE',  ( -27.40038777100000189, -74.50000000000000000, -36.59277592640000165 ) ) ;
#25790 = CARTESIAN_POINT ( 'NONE',  ( 22.78264860270000014, -94.59276292389999696, -6.873201011689999085 ) ) ;
#25791 = CARTESIAN_POINT ( 'NONE',  ( 25.54297693993040141, -68.05277662258636440, 10.87142178243190038 ) ) ;
#25792 = ORIENTED_EDGE ( 'NONE', *, *, #9296, .T. ) ;
#25793 = CARTESIAN_POINT ( 'NONE',  ( -20.54204567169999862, -95.55433883429999753, -9.451949542510000413 ) ) ;
#25794 = CARTESIAN_POINT ( 'NONE',  ( 15.80921915986327875, -101.6077248516952665, 2.654137683538275727 ) ) ;
#25795 = CARTESIAN_POINT ( 'NONE',  ( -20.72181756220000182, -93.63285492290000889, 14.13430432360000211 ) ) ;
#25796 = B_SPLINE_CURVE_WITH_KNOTS ( 'NONE', 5,
 ( #23077, #22783, #18701, #18552, #21032, #3122 ),
 .UNSPECIFIED., .F., .F.,
 ( 6, 6 ),
 ( 0.000000000000000000, 1.000000000000000000 ),
 .UNSPECIFIED. ) ;
#25797 = CARTESIAN_POINT ( 'NONE',  ( 23.96026145669999607, -92.49999926799999628, -16.90273770479999982 ) ) ;
#25798 = CARTESIAN_POINT ( 'NONE',  ( -2.495716009659999735, -52.58489974430000302, -24.49317771890000017 ) ) ;
#25799 = EDGE_CURVE ( 'NONE', #7849, #6001, #17987, .T. ) ;
#25800 = AXIS2_PLACEMENT_3D ( 'NONE', #20572, #637, #9486 ) ;
#25801 = CARTESIAN_POINT ( 'NONE',  ( 29.76135012335695151, -92.72059904821338705, 6.671735646977375644 ) ) ;
#25802 = CARTESIAN_POINT ( 'NONE',  ( 9.119802927630001221, -98.28914429610000525, 16.69368728350000097 ) ) ;
#25803 = ORIENTED_EDGE ( 'NONE', *, *, #21512, .T. ) ;
#25804 = EDGE_CURVE ( 'NONE', #2204, #3141, #16697, .T. ) ;
#25805 = DIRECTION ( 'NONE',  ( 0.000000000000000000, -1.000000000000000000, 0.000000000000000000 ) ) ;
#25806 = CIRCLE ( 'NONE', #22564, 3.750000000000000000 ) ;
#25807 = DIRECTION ( 'NONE',  ( 0.000000000000000000, 1.000000000000000000, 0.000000000000000000 ) ) ;
#25808 = DIRECTION ( 'NONE',  ( 1.000000000000000000, 0.000000000000000000, 0.000000000000000000 ) ) ;
#25809 = CARTESIAN_POINT ( 'NONE',  ( 30.93662943959999723, -73.65801418129998979, -23.56172310960000260 ) ) ;
#25810 = CARTESIAN_POINT ( 'NONE',  ( -14.15153136323935712, -74.02196623412419285, 36.23089701056277789 ) ) ;
#25811 = EDGE_CURVE ( 'NONE', #5636, #12207, #19742, .T. ) ;
#25812 = TOROIDAL_SURFACE ( 'NONE', #4400, 25.11294200180000047, 0.5000000000000000000 ) ;
#25813 = VERTEX_POINT ( 'NONE', #3416 ) ;
#25814 = CARTESIAN_POINT ( 'NONE',  ( 3.883346862689999845, -9.250000000000000000, 7.108418751309999450 ) ) ;
#25815 = CARTESIAN_POINT ( 'NONE',  ( 21.29302206940000275, -35.50409515829999663, -7.872116142319999454 ) ) ;
#25816 = CARTESIAN_POINT ( 'NONE',  ( 20.93196326829999876, -36.02994400500000438, -8.585833128470001796 ) ) ;
#25817 = CARTESIAN_POINT ( 'NONE',  ( -37.58664795480000009, -63.20096189429999356, 1.318420231159999956 ) ) ;
#25818 = ORIENTED_EDGE ( 'NONE', *, *, #12863, .T. ) ;
#25819 = CARTESIAN_POINT ( 'NONE',  ( -13.12062273610000140, -101.6095085860000040, -9.209289609949999900 ) ) ;
#25820 = CARTESIAN_POINT ( 'NONE',  ( 0.000000000000000000, -11.55246854740000018, 0.000000000000000000 ) ) ;
#25821 = CARTESIAN_POINT ( 'NONE',  ( -7.879410026489999552, -99.92967571559999840, 15.46934602219999988 ) ) ;
#25822 = ORIENTED_EDGE ( 'NONE', *, *, #14056, .F. ) ;
#25823 = TOROIDAL_SURFACE ( 'NONE', #25386, 6.750000000000000000, 0.5000000000000000000 ) ;
#25824 = CARTESIAN_POINT ( 'NONE',  ( -26.77683864449999973, -33.79999999999999716, -49.01467436490000296 ) ) ;
#25825 = DIRECTION ( 'NONE',  ( -0.8775825618903722036, 0.000000000000000000, 0.4794255386042041156 ) ) ;
#25826 = CARTESIAN_POINT ( 'NONE',  ( -20.20543299319999875, -94.98810756820000734, 12.40017484579999874 ) ) ;
#25827 = CARTESIAN_POINT ( 'NONE',  ( 7.332920525790000532, -101.1404853350000081, 13.53079052370000035 ) ) ;
#25828 = ORIENTED_EDGE ( 'NONE', *, *, #21446, .T. ) ;
#25829 = CARTESIAN_POINT ( 'NONE',  ( 13.33933447234251801, -100.8738282928510017, -9.887453640032017432 ) ) ;
#25830 = CARTESIAN_POINT ( 'NONE',  ( -25.54375670880000015, -93.49005502550001268, -5.768728999770000421 ) ) ;
#25831 = CARTESIAN_POINT ( 'NONE',  ( 39.75929607687058365, -73.82871504776804272, 7.246063797165944287 ) ) ;
#25832 = ORIENTED_EDGE ( 'NONE', *, *, #27781, .F. ) ;
#25833 = AXIS2_PLACEMENT_3D ( 'NONE', #14610, #3550, #12405 ) ;
#25834 = CARTESIAN_POINT ( 'NONE',  ( 47.24999999999992184, -74.77408259042933025, -0.4803890690156943921 ) ) ;
#25835 = CARTESIAN_POINT ( 'NONE',  ( -14.43678919070000077, -74.15747494800001505, 36.75078895099999698 ) ) ;
#25836 = CARTESIAN_POINT ( 'NONE',  ( 1.598721155460000041E-15, -84.50000000000000000, -1.998401444329999950E-16 ) ) ;
#25837 = CARTESIAN_POINT ( 'NONE',  ( -17.87039757315234567, -92.59033770622343695, 24.71676568516515715 ) ) ;
#25838 = ORIENTED_EDGE ( 'NONE', *, *, #24301, .F. ) ;
#25839 = EDGE_CURVE ( 'NONE', #7941, #6448, #8107, .T. ) ;
#25840 = CARTESIAN_POINT ( 'NONE',  ( -2.645751311070000167, -74.00000000000000000, 46.75000000000000000 ) ) ;
#25841 = CARTESIAN_POINT ( 'NONE',  ( -0.02519810411110000314, -101.1617736559999940, -15.74199841589999771 ) ) ;
#25842 = CARTESIAN_POINT ( 'NONE',  ( 9.386750785949999454, -63.25416415669999992, -23.64765651129999924 ) ) ;
#25843 = CARTESIAN_POINT ( 'NONE',  ( 16.08037959500000014, -101.3150700380000018, 2.354223078750000031 ) ) ;
#25844 = CARTESIAN_POINT ( 'NONE',  ( 21.08560127379999827, -57.47122586340000083, 10.49905553490000187 ) ) ;
#25845 = DIRECTION ( 'NONE',  ( 0.000000000000000000, 1.000000000000000000, 0.000000000000000000 ) ) ;
#25846 = EDGE_LOOP ( 'NONE', ( #14764, #1415, #23159, #106, #16162, #9562, #2799 ) ) ;
#25847 = ADVANCED_FACE ( 'NONE', ( #3139 ), #14181, .T. ) ;
#25848 = CARTESIAN_POINT ( 'NONE',  ( 6.647943390380000039, -101.0678230150000019, 14.35910459099999947 ) ) ;
#25849 = CARTESIAN_POINT ( 'NONE',  ( 15.53144063390000085, -101.3256027139999986, 3.435397172430000090 ) ) ;
#25850 = CARTESIAN_POINT ( 'NONE',  ( -9.476764215410000247, -74.50000000000000000, -38.08875739639999836 ) ) ;
#25851 = CARTESIAN_POINT ( 'NONE',  ( 23.53639228501841174, -61.46980192603786008, 10.55322908533638859 ) ) ;
#25852 = CARTESIAN_POINT ( 'NONE',  ( -6.761572831579999665, -97.58045781590000445, 18.83461070039999896 ) ) ;
#25853 = CARTESIAN_POINT ( 'NONE',  ( 3.387657239720000213, -92.79907188619999658, -28.90154850299999723 ) ) ;
#25854 = ADVANCED_FACE ( 'NONE', ( #24980 ), #25288, .F. ) ;
#25855 = CARTESIAN_POINT ( 'NONE',  ( 9.564509902230000193, -57.40875702419999982, -23.52622212079999997 ) ) ;
#25856 = CARTESIAN_POINT ( 'NONE',  ( -6.902767321779999854, -101.4121386959999995, 14.40917022280000026 ) ) ;
#25857 = ORIENTED_EDGE ( 'NONE', *, *, #24306, .T. ) ;
#25858 = CARTESIAN_POINT ( 'NONE',  ( 7.426814492070000107, -35.28814190290000141, -21.34788074219999743 ) ) ;
#25859 = CARTESIAN_POINT ( 'NONE',  ( -16.98520236649999759, -99.83167676440000093, 3.436659022809999797 ) ) ;
#25860 = VERTEX_POINT ( 'NONE', #25137 ) ;
#25861 = CARTESIAN_POINT ( 'NONE',  ( -0.8544872754590000508, -101.1411470150000014, -15.36633732259999974 ) ) ;
#25862 = CARTESIAN_POINT ( 'NONE',  ( 6.888451955769999913, -99.53431386179998697, 15.99365555089999802 ) ) ;
#25863 = CIRCLE ( 'NONE', #13275, 10.50000000000000000 ) ;
#25864 = CARTESIAN_POINT ( 'NONE',  ( 13.98842255709134896, -92.52640451557674339, 27.10303198118710455 ) ) ;
#25865 = CARTESIAN_POINT ( 'NONE',  ( 27.75394116159999669, -74.50000000000000000, -27.75394116159999669 ) ) ;
#25866 = EDGE_CURVE ( 'NONE', #25229, #11676, #28117, .T. ) ;
#25867 = CARTESIAN_POINT ( 'NONE',  ( 0.3059185938709999553, -92.50000000000000000, 14.72672055670000013 ) ) ;
#25868 = B_SPLINE_CURVE_WITH_KNOTS ( 'NONE', 3,
 ( #6675, #11455, #15686, #24593 ),
 .UNSPECIFIED., .F., .F.,
 ( 4, 4 ),
 ( 0.000000000000000000, 1.000000000000000000 ),
 .UNSPECIFIED. ) ;
#25869 = CARTESIAN_POINT ( 'NONE',  ( 11.23915397940000105, -100.8869817940000075, -10.91500585829999892 ) ) ;
#25870 = CARTESIAN_POINT ( 'NONE',  ( -19.09898282842726047, -19.48685756512668732, 14.00485772877497048 ) ) ;
#25871 = LINE ( 'NONE', #17114, #3536 ) ;
#25872 =( NAMED_UNIT ( * ) PLANE_ANGLE_UNIT ( ) SI_UNIT ( $, .RADIAN. ) );
#25873 = CIRCLE ( 'NONE', #4458, 0.3500000000000003664 ) ;
#25874 = FACE_OUTER_BOUND ( 'NONE', #17567, .T. ) ;
#25875 = ORIENTED_EDGE ( 'NONE', *, *, #5632, .T. ) ;
#25876 = CARTESIAN_POINT ( 'NONE',  ( 9.450751860034793950, -35.99944170493491669, -19.99269604853717297 ) ) ;
#25877 = ORIENTED_EDGE ( 'NONE', *, *, #6204, .T. ) ;
#25878 = B_SPLINE_CURVE_WITH_KNOTS ( 'NONE', 3,
 ( #26553, #15454, #22481, #7037, #2089, #52 ),
 .UNSPECIFIED., .F., .F.,
 ( 4, 2, 4 ),
 ( 0.000000000000000000, 0.5000000000000000000, 1.000000000000000000 ),
 .UNSPECIFIED. ) ;
#25879 = CARTESIAN_POINT ( 'NONE',  ( -0.6273717453279999967, -62.97603269449999885, -24.27362655359999977 ) ) ;
#25880 = CARTESIAN_POINT ( 'NONE',  ( -29.29590816570000200, -92.50000947299999154, 6.421684369280000304 ) ) ;
#25881 = DIRECTION ( 'NONE',  ( 0.000000000000000000, 0.000000000000000000, 1.000000000000000000 ) ) ;
#25882 = EDGE_CURVE ( 'NONE', #6664, #20661, #5315, .T. ) ;
#25883 = ORIENTED_EDGE ( 'NONE', *, *, #7993, .F. ) ;
#25884 = CARTESIAN_POINT ( 'NONE',  ( -17.88989799939055203, -97.43430234701037307, -10.14936231854670190 ) ) ;
#25885 = ADVANCED_FACE ( 'NONE', ( #12281 ), #19281, .F. ) ;
#25886 = ORIENTED_EDGE ( 'NONE', *, *, #24639, .F. ) ;
#25887 = DIRECTION ( 'NONE',  ( 0.000000000000000000, 1.000000000000000000, 0.000000000000000000 ) ) ;
#25888 = EDGE_LOOP ( 'NONE', ( #12042, #10568, #27898, #23588 ) ) ;
#25889 = EDGE_CURVE ( 'NONE', #13918, #20274, #21905, .T. ) ;
#25890 = LINE ( 'NONE', #13036, #26107 ) ;
#25891 = CARTESIAN_POINT ( 'NONE',  ( 23.36166352360000076, -57.47815920179999694, -0.2645301549009999587 ) ) ;
#25892 = DIRECTION ( 'NONE',  ( 1.000000000000000000, 0.000000000000000000, 0.000000000000000000 ) ) ;
#25893 = B_SPLINE_SURFACE_WITH_KNOTS ( 'NONE', 5, 5, ( 
 ( #12555, #15020, #25979, #6005, #21326, #6293, #16958, #26407, #15160 ),
 ( #15302, #8329, #28585, #25849, #12694, #21608, #10501, #19552, #4109 ),
 ( #3557, #23934, #21467, #3973, #28168, #5870, #24069, #3832, #12980 ),
 ( #1794, #23794, #19415, #1942, #28295, #10783, #12412, #26122, #6150 ),
 ( #23650, #1385, #1522, #28031, #10366, #19280, #8200, #12833, #21745 ),
 ( #10640, #28441, #14498, #23399, #12435, #26150, #6172, #28048, #21770 ),
 ( #16977, #17562, #1841, #21650, #19325, #1565, #26021, #28200, #19598 ),
 ( #28762, #26456, #8234, #8802, #15201, #23831, #10535, #19453, #6489 ),
 ( #15348, #4304, #13177, #22087, #19877, #17714, #4592, #6934, #257 ),
 ( #15800, #9097, #692, #9545, #22670, #20322, #18447, #24994, #2862 ),
 ( #393, #27190, #24707, #9242, #26897, #22530, #15651, #4889, #5029 ),
 ( #27331, #7229, #16094, #16237, #27041, #13621, #20034, #18000, #18299 ) ),
 .UNSPECIFIED., .F., .F., .F.,
 ( 6, 3, 3, 6 ),
 ( 6, 3, 6 ),
 ( 3.852920539479999906, 4.834764074430000669, 6.134713715070000184, 8.383984506260000913 ),
 ( 0.000000000000000000, 0.2500000000000000000, 0.5000000000000000000 ),
 .UNSPECIFIED. ) ;
#25894 = VERTEX_POINT ( 'NONE', #5167 ) ;
#25895 = CARTESIAN_POINT ( 'NONE',  ( 38.08875739639999836, -74.50000000000000000, 9.476764215410000247 ) ) ;
#25896 = CARTESIAN_POINT ( 'NONE',  ( -12.03351515999999855, -100.7833805400000102, -10.41203369199999962 ) ) ;
#25897 = CARTESIAN_POINT ( 'NONE',  ( -0.5853288072829999633, -19.15810970359999743, -22.01520171810000193 ) ) ;
#25898 = CARTESIAN_POINT ( 'NONE',  ( -7.853002983444719476, -100.5798851023766929, 14.89419455703112938 ) ) ;
#25899 = ORIENTED_EDGE ( 'NONE', *, *, #4911, .T. ) ;
#25900 = B_SPLINE_CURVE_WITH_KNOTS ( 'NONE', 5,
 ( #7758, #21279, #3241, #27982, #12098, #21011 ),
 .UNSPECIFIED., .F., .F.,
 ( 6, 6 ),
 ( 0.000000000000000000, 1.000000000000000000 ),
 .UNSPECIFIED. ) ;
#25901 = CARTESIAN_POINT ( 'NONE',  ( -12.24789267329999909, -65.07443093669999712, 21.96586363990000024 ) ) ;
#25902 = CARTESIAN_POINT ( 'NONE',  ( -31.99545665129999961, -74.00000000000000000, -22.01100727640000088 ) ) ;
#25903 = CARTESIAN_POINT ( 'NONE',  ( 47.25000000000000000, -75.00000000000000000, -1.245115460929999944E-12 ) ) ;
#25904 = ORIENTED_EDGE ( 'NONE', *, *, #19562, .F. ) ;
#25905 = CARTESIAN_POINT ( 'NONE',  ( 0.000000000000000000, -26.59999999999999787, 0.000000000000000000 ) ) ;
#25906 = CARTESIAN_POINT ( 'NONE',  ( 6.656280120269700618, -101.0610180774001208, 15.05062505483333979 ) ) ;
#25907 = DIRECTION ( 'NONE',  ( -0.000000000000000000, 1.000000000000000000, 0.000000000000000000 ) ) ;
#25908 = ORIENTED_EDGE ( 'NONE', *, *, #3588, .T. ) ;
#25909 = CARTESIAN_POINT ( 'NONE',  ( -18.28476853637538113, -98.31192523452679666, 5.137975449739348832 ) ) ;
#25910 = ORIENTED_EDGE ( 'NONE', *, *, #8370, .F. ) ;
#25911 = B_SPLINE_CURVE_WITH_KNOTS ( 'NONE', 5,
 ( #11685, #15915, #11535, #24670, #20291, #16061 ),
 .UNSPECIFIED., .F., .F.,
 ( 6, 6 ),
 ( 0.000000000000000000, 1.000000000000000000 ),
 .UNSPECIFIED. ) ;
#25912 = CARTESIAN_POINT ( 'NONE',  ( 26.25674219109999896, -93.16461300810000523, 10.85501170439999896 ) ) ;
#25913 = CARTESIAN_POINT ( 'NONE',  ( 10.20110288159999890, -74.50000000000000000, -41.00000000000000000 ) ) ;
#25914 = CARTESIAN_POINT ( 'NONE',  ( -7.627568735119999666, -74.00000000000000000, -38.62788659690000515 ) ) ;
#25915 = ORIENTED_EDGE ( 'NONE', *, *, #14756, .F. ) ;
#25916 = EDGE_CURVE ( 'NONE', #13332, #3865, #25392, .T. ) ;
#25917 = CARTESIAN_POINT ( 'NONE',  ( 9.644866014229998896, -36.00000000000000000, -20.16453884109999706 ) ) ;
#25918 = CARTESIAN_POINT ( 'NONE',  ( 0.2284267155709999997, -92.50000000000000000, -29.91770779450000362 ) ) ;
#25919 = EDGE_CURVE ( 'NONE', #2354, #26414, #26740, .T. ) ;
#25920 = DIRECTION ( 'NONE',  ( 0.000000000000000000, -1.000000000000000000, 0.000000000000000000 ) ) ;
#25921 = EDGE_CURVE ( 'NONE', #9163, #7997, #23309, .T. ) ;
#25922 = CARTESIAN_POINT ( 'NONE',  ( -38.55000000000000426, -65.14977478849999670, -2.857883832489999776 ) ) ;
#25923 = CARTESIAN_POINT ( 'NONE',  ( -3.610293368829999849, -18.50000000000000000, -24.43613445369999937 ) ) ;
#25924 = VERTEX_POINT ( 'NONE', #24065 ) ;
#25925 = EDGE_CURVE ( 'NONE', #9200, #8106, #24704, .T. ) ;
#25926 = CARTESIAN_POINT ( 'NONE',  ( 25.27264893869653051, -64.89166019501105609, 0.6762966387480369157 ) ) ;
#25927 = CARTESIAN_POINT ( 'NONE',  ( 13.55377673239999936, -100.4650220110000021, -9.985834839249999817 ) ) ;
#25928 = DIRECTION ( 'NONE',  ( 0.4794255386042038936, 0.000000000000000000, 0.8775825618903723147 ) ) ;
#25929 = CARTESIAN_POINT ( 'NONE',  ( 23.88294446200000110, -92.63555401869999173, -18.57671364879999842 ) ) ;
#25930 = CARTESIAN_POINT ( 'NONE',  ( -2.664535259099999805E-15, -72.00000000000000000, -3.552713678799999608E-15 ) ) ;
#25931 = CIRCLE ( 'NONE', #12872, 7.750000000000000000 ) ;
#25932 = CARTESIAN_POINT ( 'NONE',  ( -2.939806355540000027, -80.25752946859999781, 46.70460469590000230 ) ) ;
#25933 = CARTESIAN_POINT ( 'NONE',  ( -19.23405768510000158, -19.49009541670000445, 14.16176834190000022 ) ) ;
#25934 = ORIENTED_EDGE ( 'NONE', *, *, #7215, .T. ) ;
#25935 = FACE_OUTER_BOUND ( 'NONE', #17555, .T. ) ;
#25936 = CARTESIAN_POINT ( 'NONE',  ( -6.665307709260000379, -93.00000000000000000, -13.13558364449999871 ) ) ;
#25937 = DIRECTION ( 'NONE',  ( 1.000000000000000000, 0.000000000000000000, 0.000000000000000000 ) ) ;
#25938 = CARTESIAN_POINT ( 'NONE',  ( 19.42375544529999942, -18.50000000000000000, 8.976408266139999981 ) ) ;
#25939 = DIRECTION ( 'NONE',  ( 0.4794255386042042266, 0.000000000000000000, 0.8775825618903720926 ) ) ;
#25940 = DIRECTION ( 'NONE',  ( 1.000000000000000000, 0.000000000000000000, 0.000000000000000000 ) ) ;
#25941 = PRESENTATION_LAYER_ASSIGNMENT (  '', '', ( #19422 ) ) ;
#25942 = DIRECTION ( 'NONE',  ( 0.8775825618903722036, 0.000000000000000000, -0.4794255386042041156 ) ) ;
#25943 = ORIENTED_EDGE ( 'NONE', *, *, #22086, .F. ) ;
#25944 = CARTESIAN_POINT ( 'NONE',  ( 20.62428382529999737, -35.57628701899999868, -8.744932029230000126 ) ) ;
#25945 = ORIENTED_EDGE ( 'NONE', *, *, #25014, .F. ) ;
#25946 = AXIS2_PLACEMENT_3D ( 'NONE', #6547, #2328, #24619 ) ;
#25947 = CARTESIAN_POINT ( 'NONE',  ( 21.46963261560000191, -36.58933600920000373, -7.659111216379999476 ) ) ;
#25948 = CARTESIAN_POINT ( 'NONE',  ( -43.07153896660000214, -69.00000000000000000, -1.677989385109999843 ) ) ;
#25949 = VERTEX_POINT ( 'NONE', #17373 ) ;
#25950 = CARTESIAN_POINT ( 'NONE',  ( 10.58737011899999914, -97.65299964609999961, 16.87371021290000073 ) ) ;
#25951 = EDGE_CURVE ( 'NONE', #10333, #5430, #10693, .T. ) ;
#25952 = B_SPLINE_CURVE_WITH_KNOTS ( 'NONE', 3,
 ( #13449, #27168, #22355, #20613, #375, #20763, #9219, #7065, #2399, #20161, #16074, #9079, #27314, #18424, #17982, #22799, #6914, #15929 ),
 .UNSPECIFIED., .F., .F.,
 ( 4, 2, 2, 2, 1, 1, 1, 1, 2, 2, 4 ),
 ( 0.000000000000000000, 0.2500000000000573430, 0.3750000000000868194, 0.4375000000001025846, 0.4687500000001104672, 0.4843750000001151856, 0.4921875000001167955, 0.4960937500001167955, 0.4980468750001167955, 0.5000000000001167955, 1.000000000000000000 ),
 .UNSPECIFIED. ) ;
#25953 = DIRECTION ( 'NONE',  ( -1.738658080639908902E-17, 0.000000000000000000, 1.000000000000000000 ) ) ;
#25954 = ORIENTED_EDGE ( 'NONE', *, *, #26851, .T. ) ;
#25955 = CARTESIAN_POINT ( 'NONE',  ( 0.03691039440750000511, -93.36531860680000250, 26.17328399250000004 ) ) ;
#25956 = FACE_OUTER_BOUND ( 'NONE', #5214, .T. ) ;
#25957 = CARTESIAN_POINT ( 'NONE',  ( -39.73620294722308444, -65.71460843033641197, 2.210699957725660525 ) ) ;
#25958 = VERTEX_POINT ( 'NONE', #1790 ) ;
#25959 = EDGE_CURVE ( 'NONE', #26635, #8189, #20024, .T. ) ;
#25960 = VECTOR ( 'NONE', #17305, 1000.000000000000000 ) ;
#25961 = CARTESIAN_POINT ( 'NONE',  ( 9.348798002780000616, -10.50000000000000000, 17.11285995690000306 ) ) ;
#25962 = CARTESIAN_POINT ( 'NONE',  ( -25.53339762659999934, -93.24058218849999946, -5.837366266040000085 ) ) ;
#25963 = CARTESIAN_POINT ( 'NONE',  ( 39.79858521549137151, -73.85166138343194575, 7.247217007256502974 ) ) ;
#25964 = ORIENTED_EDGE ( 'NONE', *, *, #26020, .T. ) ;
#25965 = CARTESIAN_POINT ( 'NONE',  ( -14.52836087100000029, -74.22231530550000400, 36.83217634790000261 ) ) ;
#25966 = CARTESIAN_POINT ( 'NONE',  ( -14.64485457939999868, -74.39167553240000075, 36.47327398630000062 ) ) ;
#25967 = CARTESIAN_POINT ( 'NONE',  ( -18.18547914559999867, -94.42120323109999447, 17.31458345580000113 ) ) ;
#25968 = CARTESIAN_POINT ( 'NONE',  ( -19.92371129995309076, -92.49999999999992895, 21.06559270865390587 ) ) ;
#25969 = ORIENTED_EDGE ( 'NONE', *, *, #14414, .T. ) ;
#25970 = CARTESIAN_POINT ( 'NONE',  ( 26.77683864449999973, -19.40000000000000213, 49.01467436490000296 ) ) ;
#25971 = CIRCLE ( 'NONE', #10557, 24.76278252470000041 ) ;
#25972 = CARTESIAN_POINT ( 'NONE',  ( 0.03568166535660000083, -101.2902355740000075, -15.92847312690000372 ) ) ;
#25973 = CARTESIAN_POINT ( 'NONE',  ( 23.23309162749999857, -57.41957467990000197, -9.464546293550000655 ) ) ;
#25974 = CARTESIAN_POINT ( 'NONE',  ( -4.500000000000000000, -11.00000000000000000, 40.50000000000000000 ) ) ;
#25975 = CARTESIAN_POINT ( 'NONE',  ( 22.57886154579999882, -57.83919435140000331, 10.16307356839999798 ) ) ;
#25976 = CARTESIAN_POINT ( 'NONE',  ( -10.40309664509999976, -19.44965585980000000, -20.22773501060000001 ) ) ;
#25977 = VERTEX_POINT ( 'NONE', #17081 ) ;
#25978 = CARTESIAN_POINT ( 'NONE',  ( 6.186462384450000407, -100.1275643909999928, 15.45527146859999945 ) ) ;
#25979 = CARTESIAN_POINT ( 'NONE',  ( 15.60714071820000015, -101.4254868729999970, 3.380050261510000098 ) ) ;
#25980 = CIRCLE ( 'NONE', #13407, 7.249999999999999112 ) ;
#25981 = CARTESIAN_POINT ( 'NONE',  ( -2.664535259099999805E-15, -72.82938648530000592, -3.552713678799999608E-15 ) ) ;
#25982 = CARTESIAN_POINT ( 'NONE',  ( 21.02965361369999897, -18.50000000000000000, -0.4426258060200000122 ) ) ;
#25983 = ADVANCED_FACE ( 'NONE', ( #1378 ), #20163, .F. ) ;
#25984 = CARTESIAN_POINT ( 'NONE',  ( -0.7205257401540000606, -101.1889999979999999, -15.98376809950000066 ) ) ;
#25985 = ORIENTED_EDGE ( 'NONE', *, *, #4474, .F. ) ;
#25986 = CARTESIAN_POINT ( 'NONE',  ( 8.236226396380001091, -93.85715850789999593, -23.50030299510000020 ) ) ;
#25987 = EDGE_CURVE ( 'NONE', #20862, #10652, #17516, .T. ) ;
#25988 = DIRECTION ( 'NONE',  ( 0.4794255386042040046, 0.000000000000000000, 0.8775825618903722036 ) ) ;
#25989 = DIRECTION ( 'NONE',  ( 1.000000000000000000, 0.000000000000000000, 0.000000000000000000 ) ) ;
#25990 = ORIENTED_EDGE ( 'NONE', *, *, #4696, .F. ) ;
#25991 = CARTESIAN_POINT ( 'NONE',  ( 15.74335372269999844, -111.0000000000000000, 2.854262350119999958 ) ) ;
#25992 = VERTEX_POINT ( 'NONE', #18057 ) ;
#25993 = EDGE_CURVE ( 'NONE', #20928, #4268, #9303, .T. ) ;
#25994 = DIRECTION ( 'NONE',  ( 0.000000000000000000, -1.000000000000000000, 0.000000000000000000 ) ) ;
#25995 = CARTESIAN_POINT ( 'NONE',  ( -11.40415961587557447, -19.46574740001101844, 19.06929969032851346 ) ) ;
#25996 = LINE ( 'NONE', #12164, #5754 ) ;
#25997 = DIRECTION ( 'NONE',  ( 0.000000000000000000, 1.000000000000000000, 0.000000000000000000 ) ) ;
#25998 = CARTESIAN_POINT ( 'NONE',  ( 16.20707181140645758, -94.69873403835963188, 17.23731209724227753 ) ) ;
#25999 = CIRCLE ( 'NONE', #24614, 1.999999999999998002 ) ;
#26000 = CARTESIAN_POINT ( 'NONE',  ( -22.62751353610000393, -71.52549858170000618, 16.81410928309999875 ) ) ;
#26001 = AXIS2_PLACEMENT_3D ( 'NONE', #27830, #7870, #15101 ) ;
#26002 = CARTESIAN_POINT ( 'NONE',  ( 9.885503723209998483, -36.00000000000000000, -20.33566493420000043 ) ) ;
#26003 = CARTESIAN_POINT ( 'NONE',  ( 3.552713678799999608E-15, -18.50000000000000000, 3.552713678799999608E-15 ) ) ;
#26004 = CARTESIAN_POINT ( 'NONE',  ( 7.365644968139999804, -35.41472402500000527, -21.38036730929999862 ) ) ;
#26005 = CARTESIAN_POINT ( 'NONE',  ( 0.000000000000000000, -92.50000000000000000, 0.000000000000000000 ) ) ;
#26006 = ORIENTED_EDGE ( 'NONE', *, *, #4407, .F. ) ;
#26007 = CARTESIAN_POINT ( 'NONE',  ( 8.011707311729999503, -18.50000000000000000, -19.70300569300000149 ) ) ;
#26008 = SHAPE_REPRESENTATION ( 'MAS-679', ( #27406, #11059, #12912, #5515, #27848, #25074, #12467, #23205, #28754, #21782 ), #421 ) ;
#26009 = EDGE_CURVE ( 'NONE', #3254, #20039, #26959, .T. ) ;
#26010 = ORIENTED_EDGE ( 'NONE', *, *, #13273, .F. ) ;
#26011 = DIRECTION ( 'NONE',  ( 0.9704142011833034598, 0.000000000000000000, -0.2414462220490750932 ) ) ;
#26012 = CARTESIAN_POINT ( 'NONE',  ( -2.003725483539999797, -63.79833278959999632, -24.98874254210000245 ) ) ;
#26013 = CIRCLE ( 'NONE', #28336, 18.64285714289999518 ) ;
#26014 = CARTESIAN_POINT ( 'NONE',  ( -29.00049327840000046, -92.49537389370000540, 4.812555014239999096 ) ) ;
#26015 = CARTESIAN_POINT ( 'NONE',  ( -0.7149044700954795273, -101.3051320416606700, -15.85906875946512251 ) ) ;
#26016 = CYLINDRICAL_SURFACE ( 'NONE', #1106, 3.000000000000001332 ) ;
#26017 = VECTOR ( 'NONE', #11948, 1000.000000000000000 ) ;
#26018 = AXIS2_PLACEMENT_3D ( 'NONE', #6275, #15141, #4089 ) ;
#26019 = ADVANCED_FACE ( 'NONE', ( #2481 ), #4193, .T. ) ;
#26020 = EDGE_CURVE ( 'NONE', #24085, #15706, #12124, .T. ) ;
#26021 = CARTESIAN_POINT ( 'NONE',  ( 15.28250192019999965, -100.7707614970000094, 4.221087105419999652 ) ) ;
#26022 = ORIENTED_EDGE ( 'NONE', *, *, #21578, .F. ) ;
#26023 = B_SPLINE_CURVE_WITH_KNOTS ( 'NONE', 3,
 ( #16096, #13321, #2715, #6791, #13625, #20037, #20480, #9394, #4451, #26758, #15654, #11424, #22224, #27044, #18301, #2272, #24555, #11569, #20325, #24856, #2425, #396, #9245, #24996, #25306, #20926, #16675, #14222, #3431, #27766, #3154, #16544 ),
 .UNSPECIFIED., .F., .F.,
 ( 4, 2, 2, 1, 1, 1, 1, 1, 2, 2, 2, 2, 1, 1, 1, 1, 1, 2, 2, 2, 4 ),
 ( 0.000000000000000000, 0.1249999999999014400, 0.1874999999998525624, 0.2187499999998276379, 0.2343749999998150091, 0.2421874999998090416, 0.2460937499998054057, 0.2480468749998035738, 0.2490234374998036015, 0.2499999999998036015, 0.3749999999998803735, 0.4374999999999194533, 0.4687499999999386047, 0.4843749999999479861, 0.4921874999999526490, 0.4960937499999552025, 0.4980468749999555911, 0.4990234374999557576, 0.4999999999999559241, 0.7499999999999779066, 1.000000000000000000 ),
 .UNSPECIFIED. ) ;
#26024 = CARTESIAN_POINT ( 'NONE',  ( -16.55071332594993549, -98.16872836274220049, -10.59832500731132754 ) ) ;
#26025 = CARTESIAN_POINT ( 'NONE',  ( -13.49470513559979956, -57.43018267548258393, 20.74700234779956887 ) ) ;
#26026 = ORIENTED_EDGE ( 'NONE', *, *, #1256, .F. ) ;
#26027 = CARTESIAN_POINT ( 'NONE',  ( 8.782858223105064255, -69.73938810552070322, -25.82417951732658423 ) ) ;
#26028 = CARTESIAN_POINT ( 'NONE',  ( -18.46133609720000024, -18.50000000000000000, 14.80231853080000093 ) ) ;
#26029 = CARTESIAN_POINT ( 'NONE',  ( -15.54889200169999874, -101.4254868860000016, 3.639708781509999991 ) ) ;
#26030 = CARTESIAN_POINT ( 'NONE',  ( -19.73288567159999829, -59.03018501249999872, 12.72771757599999987 ) ) ;
#26031 = ORIENTED_EDGE ( 'NONE', *, *, #10958, .F. ) ;
#26032 = DIRECTION ( 'NONE',  ( 0.000000000000000000, 1.000000000000000000, 0.000000000000000000 ) ) ;
#26033 = CARTESIAN_POINT ( 'NONE',  ( -12.00940321250000054, -100.8772072149999985, -10.26826983859999842 ) ) ;
#26034 = CARTESIAN_POINT ( 'NONE',  ( 24.61545324444739435, -93.04141874247781629, 14.32622737458234496 ) ) ;
#26035 = CARTESIAN_POINT ( 'NONE',  ( -7.533632261058696322, -101.1742791176865097, 14.53131762976900276 ) ) ;
#26036 = ORIENTED_EDGE ( 'NONE', *, *, #15300, .F. ) ;
#26037 = AXIS2_PLACEMENT_3D ( 'NONE', #12007, #12150, #21472 ) ;
#26038 = AXIS2_PLACEMENT_3D ( 'NONE', #11770, #7422, #595 ) ;
#26039 = EDGE_CURVE ( 'NONE', #22634, #8673, #18307, .T. ) ;
#26040 = DIRECTION ( 'NONE',  ( 0.000000000000000000, 1.000000000000000000, 0.000000000000000000 ) ) ;
#26041 = CARTESIAN_POINT ( 'NONE',  ( -32.33633361700000108, -74.08184093439999174, -21.99126984970000365 ) ) ;
#26042 = LINE ( 'NONE', #8254, #9891 ) ;
#26043 = ORIENTED_EDGE ( 'NONE', *, *, #14157, .F. ) ;
#26044 = CARTESIAN_POINT ( 'NONE',  ( 36.90247978408418561, -79.73079169351882456, -14.43263691159852158 ) ) ;
#26045 = CARTESIAN_POINT ( 'NONE',  ( 6.661515206416465773, -100.9570234915945122, 15.13779097725072376 ) ) ;
#26046 = CARTESIAN_POINT ( 'NONE',  ( -1.791418428495746618, -80.15006986280296530, 47.02519385070965541 ) ) ;
#26047 = ORIENTED_EDGE ( 'NONE', *, *, #21490, .F. ) ;
#26048 = CARTESIAN_POINT ( 'NONE',  ( 3.393335959449999838E-15, -69.50000000000000000, 46.75000000000000000 ) ) ;
#26049 = DIRECTION ( 'NONE',  ( 1.000000000000000000, 0.000000000000000000, 0.000000000000000000 ) ) ;
#26050 = ORIENTED_EDGE ( 'NONE', *, *, #24881, .T. ) ;
#26051 = CARTESIAN_POINT ( 'NONE',  ( 29.30603805220000169, -92.54628605920001405, 7.013473232189999962 ) ) ;
#26052 = FACE_OUTER_BOUND ( 'NONE', #1733, .T. ) ;
#26053 = VERTEX_POINT ( 'NONE', #9451 ) ;
#26054 = CARTESIAN_POINT ( 'NONE',  ( 12.38290840660000036, -101.0875971110000080, -9.170880648609999852 ) ) ;
#26055 = CARTESIAN_POINT ( 'NONE',  ( 22.96193664179805793, -37.37167648649992913, -9.452942635469471000 ) ) ;
#26056 = VECTOR ( 'NONE', #9469, 1000.000000000000000 ) ;
#26057 = ORIENTED_EDGE ( 'NONE', *, *, #1753, .F. ) ;
#26058 = LINE ( 'NONE', #12913, #20438 ) ;
#26059 = FACE_OUTER_BOUND ( 'NONE', #27272, .T. ) ;
#26060 = CARTESIAN_POINT ( 'NONE',  ( -22.03947464310000015, -92.99999932709999939, -20.07685987300000008 ) ) ;
#26061 = CARTESIAN_POINT ( 'NONE',  ( -3.588515834300000318, -18.50000000000000000, -23.38914531389999851 ) ) ;
#26062 = VERTEX_POINT ( 'NONE', #12209 ) ;
#26063 = CARTESIAN_POINT ( 'NONE',  ( -14.99089894709999982, -98.53908914310000000, -11.25712186019999983 ) ) ;
#26064 = CARTESIAN_POINT ( 'NONE',  ( 12.92698146070000043, -100.9678331089999972, -9.732993700310000662 ) ) ;
#26065 = DIRECTION ( 'NONE',  ( 1.000000000000000000, 0.000000000000000000, 0.000000000000000000 ) ) ;
#26066 = CARTESIAN_POINT ( 'NONE',  ( 24.04045223339999993, -92.49537389370000540, -16.91880470280000281 ) ) ;
#26067 = CARTESIAN_POINT ( 'NONE',  ( 0.000000000000000000, -110.0000000000000000, 0.000000000000000000 ) ) ;
#26068 = CARTESIAN_POINT ( 'NONE',  ( 10.74178339546501348, -72.55263011558345454, -26.81973417036990526 ) ) ;
#26069 = CARTESIAN_POINT ( 'NONE',  ( -38.25000000000000000, -65.19264941160000149, -2.595760183519999931 ) ) ;
#26070 = ORIENTED_EDGE ( 'NONE', *, *, #25528, .T. ) ;
#26071 = CARTESIAN_POINT ( 'NONE',  ( 0.000000000000000000, -92.50000000000000000, 29.91857981989999971 ) ) ;
#26072 = EDGE_CURVE ( 'NONE', #22767, #3830, #539, .T. ) ;
#26073 = CARTESIAN_POINT ( 'NONE',  ( 10.73867332049999845, -11.85850980319999870, 19.65700966069999822 ) ) ;
#26074 = DIRECTION ( 'NONE',  ( 0.4794255386042040601, 0.000000000000000000, 0.8775825618903720926 ) ) ;
#26075 = DIRECTION ( 'NONE',  ( 0.000000000000000000, 1.000000000000000000, 0.000000000000000000 ) ) ;
#26076 = CARTESIAN_POINT ( 'NONE',  ( -14.05182617927096977, -69.64987745509210981, 23.32999788250410589 ) ) ;
#26077 = AXIS2_PLACEMENT_3D ( 'NONE', #13380, #7285, #19938 ) ;
#26079 = ADVANCED_FACE ( 'NONE', ( #14809 ), #25486, .F. ) ;
#26078 = AXIS2_PLACEMENT_3D ( 'NONE', #3981, #17098, #15462 ) ;
#26080 = VECTOR ( 'NONE', #6432, 1000.000000000000000 ) ;
#26081 = CARTESIAN_POINT ( 'NONE',  ( 26.77683864449999973, -30.20000000000000284, 49.01467436490000296 ) ) ;
#26082 = ADVANCED_FACE ( 'NONE', ( #17014 ), #13510, .T. ) ;
#26083 = EDGE_CURVE ( 'NONE', #26536, #15375, #18795, .T. ) ;
#26084 = ORIENTED_EDGE ( 'NONE', *, *, #27665, .F. ) ;
#26085 = CARTESIAN_POINT ( 'NONE',  ( 21.44286899589999962, -36.30033507760000333, -7.882324037790000126 ) ) ;
#26086 = EDGE_LOOP ( 'NONE', ( #15639, #22048, #16058, #5782 ) ) ;
#26087 = CARTESIAN_POINT ( 'NONE',  ( 21.40156196539999911, -36.43444512949999847, -7.913580641820001205 ) ) ;
#26088 = CARTESIAN_POINT ( 'NONE',  ( -43.08431406180000067, -65.21397798589998729, -0.2399963883299999767 ) ) ;
#26089 = ORIENTED_EDGE ( 'NONE', *, *, #23094, .F. ) ;
#26090 = CARTESIAN_POINT ( 'NONE',  ( 12.15866047070000100, -97.18712516009998126, 17.03251418340000001 ) ) ;
#26091 = CARTESIAN_POINT ( 'NONE',  ( -16.07598155610000035, -92.73227869829999293, -23.64671446510000052 ) ) ;
#26092 = CARTESIAN_POINT ( 'NONE',  ( -8.110006665580000274, -99.58396362730000817, 15.35220468210000178 ) ) ;
#26093 = DIRECTION ( 'NONE',  ( 0.000000000000000000, 1.000000000000000000, 0.000000000000000000 ) ) ;
#26094 = CARTESIAN_POINT ( 'NONE',  ( 7.317502146920000783, -53.29669431050000128, -22.03392159830000097 ) ) ;
#26095 = CARTESIAN_POINT ( 'NONE',  ( -29.71794281087073841, -92.74292563043081827, 6.862529067643276193 ) ) ;
#26096 = AXIS2_PLACEMENT_3D ( 'NONE', #9802, #5716, #14600 ) ;
#26097 = CARTESIAN_POINT ( 'NONE',  ( -40.46358016753210052, -65.65208897057550530, 2.288374076695098402 ) ) ;
#26098 = ORIENTED_EDGE ( 'NONE', *, *, #20468, .F. ) ;
#26099 = AXIS2_PLACEMENT_3D ( 'NONE', #14849, #12379, #12655 ) ;
#26100 = CARTESIAN_POINT ( 'NONE',  ( 13.50420993948647741, -100.6338045025844821, -9.984825884511051797 ) ) ;
#26101 = AXIS2_PLACEMENT_3D ( 'NONE', #20120, #18528, #2657 ) ;
#26102 = CARTESIAN_POINT ( 'NONE',  ( 22.90398887539999961, -42.27112620169999957, 0.07876620758919998522 ) ) ;
#26103 = CARTESIAN_POINT ( 'NONE',  ( 23.75597685949999871, -64.47176800949999631, 10.65806687269999919 ) ) ;
#26104 = CARTESIAN_POINT ( 'NONE',  ( 47.25000000000000000, -74.50000000000000000, 2.433892081919999696E-15 ) ) ;
#26105 = VERTEX_POINT ( 'NONE', #12474 ) ;
#26106 = CARTESIAN_POINT ( 'NONE',  ( -39.03055149349999908, -74.00035141509999903, 7.562763921490000207 ) ) ;
#26107 = VECTOR ( 'NONE', #8665, 1000.000000000000000 ) ;
#26108 = FACE_OUTER_BOUND ( 'NONE', #5106, .T. ) ;
#26109 = CARTESIAN_POINT ( 'NONE',  ( 11.70455088819999823, -111.0000000000000000, 8.942783294160001617 ) ) ;
#26110 = CARTESIAN_POINT ( 'NONE',  ( -20.65988748905770578, -93.37625791770756223, 15.48159536565925798 ) ) ;
#26111 = VERTEX_POINT ( 'NONE', #25356 ) ;
#26112 = CARTESIAN_POINT ( 'NONE',  ( -1.606089563071368298, -74.11252154793176317, 47.07538657613434196 ) ) ;
#26113 = CARTESIAN_POINT ( 'NONE',  ( -0.09837475146920000857, -101.5369810359999860, -15.99989550839999985 ) ) ;
#26114 = CARTESIAN_POINT ( 'NONE',  ( 9.477371851879999198, -58.85143836710000187, -23.27434801040000067 ) ) ;
#26115 = CARTESIAN_POINT ( 'NONE',  ( -12.78424652700000053, -68.56882598480000013, -23.49261584819999982 ) ) ;
#26116 = CARTESIAN_POINT ( 'NONE',  ( 21.64704464699999775, -57.88555731719999642, 10.21083367329999980 ) ) ;
#26117 = CARTESIAN_POINT ( 'NONE',  ( -10.44159655029999989, -19.42972408440000009, -20.93628310600000120 ) ) ;
#26118 = ORIENTED_EDGE ( 'NONE', *, *, #7254, .T. ) ;
#26119 = EDGE_CURVE ( 'NONE', #5636, #10192, #5520, .T. ) ;
#26120 = AXIS2_PLACEMENT_3D ( 'NONE', #1258, #3152, #19014 ) ;
#26121 = CARTESIAN_POINT ( 'NONE',  ( 6.782523189059999957, -100.1981337080000003, 15.56999851120000145 ) ) ;
#26122 = CARTESIAN_POINT ( 'NONE',  ( 14.90817938300000023, -101.1402801299999936, 3.615773941519999646 ) ) ;
#26123 = CARTESIAN_POINT ( 'NONE',  ( -5.868160160552678306, -97.38870237642460381, 19.77461684056510194 ) ) ;
#26124 = CIRCLE ( 'NONE', #15884, 0.5000000000000004441 ) ;
#26125 = AXIS2_PLACEMENT_3D ( 'NONE', #173, #22151, #26668 ) ;
#26126 = EDGE_CURVE ( 'NONE', #8703, #20241, #17241, .T. ) ;
#26127 = CIRCLE ( 'NONE', #4732, 61.35000000000000142 ) ;
#26128 = CARTESIAN_POINT ( 'NONE',  ( 46.25000000000000000, -79.00000000000000000, -13.75000000000000000 ) ) ;
#26129 = CARTESIAN_POINT ( 'NONE',  ( 23.42054537965112715, -60.74944441296194242, 10.50581986722356831 ) ) ;
#26130 = CARTESIAN_POINT ( 'NONE',  ( 7.627568735119999666, -74.00000000000000000, 38.62788659690000515 ) ) ;
#26131 = VERTEX_POINT ( 'NONE', #10288 ) ;
#26132 = CARTESIAN_POINT ( 'NONE',  ( 7.776016120819999600, -93.59856727299998624, -24.15955163539999617 ) ) ;
#26133 = B_SPLINE_SURFACE_WITH_KNOTS ( 'NONE', 5, 5, ( 
 ( #23105, #3423, #9536, #1120, #9823, #7527 ),
 ( #12147, #18875, #14484, #11865, #12288, #18732 ),
 ( #24988, #18439, #832, #12003, #14347, #18291 ),
 ( #9674, #7367, #18585, #27760, #23242, #9388 ),
 ( #7796, #541, #11714, #2855, #22965, #7670 ),
 ( #13911, #27181, #7221, #16384, #20918, #5461 ) ),
 .UNSPECIFIED., .F., .F., .F.,
 ( 6, 6 ),
 ( 6, 6 ),
 ( 0.000000000000000000, 1.134864905219999942 ),
 ( 0.000000000000000000, 2.000000000000000000 ),
 .UNSPECIFIED. ) ;
#26134 = CARTESIAN_POINT ( 'NONE',  ( 21.10194156680000077, -31.56454113959999930, -7.680651150220001000 ) ) ;
#26135 = DIRECTION ( 'NONE',  ( 0.4794255386042041156, 0.000000000000000000, 0.8775825618903720926 ) ) ;
#26136 = CARTESIAN_POINT ( 'NONE',  ( -35.88566914520000495, -79.50000000000000000, -26.69328098980000163 ) ) ;
#26137 = ORIENTED_EDGE ( 'NONE', *, *, #4169, .T. ) ;
#26138 = CARTESIAN_POINT ( 'NONE',  ( 40.00000000000000000, -80.00000000000000000, 5.426760838410000257E-16 ) ) ;
#26139 = CARTESIAN_POINT ( 'NONE',  ( -12.46749392793309319, -101.2637735887273038, -10.49728468171560714 ) ) ;
#26140 = VERTEX_POINT ( 'NONE', #25901 ) ;
#26141 = DIRECTION ( 'NONE',  ( 0.9952295494196653491, 0.000000000000000000, -0.09756097560976997873 ) ) ;
#26142 = CARTESIAN_POINT ( 'NONE',  ( -1.017451505570000192, -101.1130130960000031, -15.39193785830000039 ) ) ;
#26143 = VECTOR ( 'NONE', #3738, 1000.000000000000000 ) ;
#26144 = CARTESIAN_POINT ( 'NONE',  ( 22.19353322110000093, -19.46528100780000159, 0.3620904308219999868 ) ) ;
#26145 = CARTESIAN_POINT ( 'NONE',  ( 0.000000000000000000, -16.50000000000000000, 0.000000000000000000 ) ) ;
#26146 = TOROIDAL_SURFACE ( 'NONE', #27567, 16.50000000000000000, 5.500000000000000000 ) ;
#26147 = CARTESIAN_POINT ( 'NONE',  ( -20.40343802174961496, -92.66972459458344247, -22.67045984017129001 ) ) ;
#26148 = CARTESIAN_POINT ( 'NONE',  ( -14.42556421679999978, -93.00000000000000000, -2.978755036369999942 ) ) ;
#26149 = TOROIDAL_SURFACE ( 'NONE', #24268, 55.85192378860000417, 0.3499999999999999778 ) ;
#26150 = CARTESIAN_POINT ( 'NONE',  ( 15.27533372839999792, -100.8772072149999985, 4.040706681419999668 ) ) ;
#26151 = FACE_OUTER_BOUND ( 'NONE', #22289, .T. ) ;
#26152 = CARTESIAN_POINT ( 'NONE',  ( -22.33897789299999914, -68.90459131420000460, 16.95310341020000067 ) ) ;
#26153 = B_SPLINE_CURVE_WITH_KNOTS ( 'NONE', 3,
 ( #1524, #10368, #1798, #10642, #8480, #19284, #28169, #17381, #6008, #14887, #1665, #26275, #6297, #12698, #21612, #15162, #11233, #24368, #19986, #15758 ),
 .UNSPECIFIED., .F., .F.,
 ( 4, 2, 1, 2, 2, 2, 2, 1, 2, 2, 4 ),
 ( 0.000000000000000000, 0.1249999999999719114, 0.1874999999999518996, 0.2187499999999366618, 0.2499999999999214240, 0.4999999999999079625, 0.6249999999999011902, 0.6874999999998885336, 0.7187499999998855360, 0.7499999999998825384, 1.000000000000000000 ),
 .UNSPECIFIED. ) ;
#26155 = EDGE_CURVE ( 'NONE', #4784, #6187, #8840, .T. ) ;
#26154 = CARTESIAN_POINT ( 'NONE',  ( 29.41275679339999982, -37.50000000000000000, 53.83969017199999740 ) ) ;
#26156 = CARTESIAN_POINT ( 'NONE',  ( -19.11972945367608645, -19.48733830559194047, 14.02465414947584499 ) ) ;
#26157 = CARTESIAN_POINT ( 'NONE',  ( 7.151042947790000603, -36.56947956750000372, -21.49478542010000126 ) ) ;
#26158 = CARTESIAN_POINT ( 'NONE',  ( 26.73328265790000202, -93.00000450890000536, -12.41349335419999989 ) ) ;
#26159 = ORIENTED_EDGE ( 'NONE', *, *, #21609, .T. ) ;
#26160 = EDGE_CURVE ( 'NONE', #28503, #23820, #10147, .T. ) ;
#26161 = FACE_OUTER_BOUND ( 'NONE', #10029, .T. ) ;
#26162 = ORIENTED_EDGE ( 'NONE', *, *, #3612, .F. ) ;
#26163 = CARTESIAN_POINT ( 'NONE',  ( 21.02691855299999801, -36.00000000000000000, -10.65875727889999958 ) ) ;
#26164 = EDGE_CURVE ( 'NONE', #25610, #3079, #17935, .T. ) ;
#26165 = EDGE_LOOP ( 'NONE', ( #8677, #23808 ) ) ;
#26166 = AXIS2_PLACEMENT_3D ( 'NONE', #8376, #17282, #12875 ) ;
#26167 = CARTESIAN_POINT ( 'NONE',  ( -1.469715598349999874, -62.89113864609998927, -24.38506619410000198 ) ) ;
#26168 = CYLINDRICAL_SURFACE ( 'NONE', #11113, 57.74999999999999289 ) ;
#26169 = CARTESIAN_POINT ( 'NONE',  ( -19.52688526260000046, -53.83744478090000030, 12.95367122460000076 ) ) ;
#26170 = LINE ( 'NONE', #26455, #2005 ) ;
#26171 = ORIENTED_EDGE ( 'NONE', *, *, #10586, .F. ) ;
#26172 = FACE_BOUND ( 'NONE', #21499, .T. ) ;
#26173 = ORIENTED_EDGE ( 'NONE', *, *, #5667, .F. ) ;
#26174 = CARTESIAN_POINT ( 'NONE',  ( -14.62247892739999955, -92.50000000000000000, -26.76626813769999913 ) ) ;
#26175 = EDGE_LOOP ( 'NONE', ( #965, #1625, #12740, #10381 ) ) ;
#26176 = CARTESIAN_POINT ( 'NONE',  ( -14.42818049519999946, -79.93744130869998799, 36.87246981650000777 ) ) ;
#26177 = CARTESIAN_POINT ( 'NONE',  ( -17.53900985619999631, -18.50000000000000000, 11.92518103370000127 ) ) ;
#26178 = CARTESIAN_POINT ( 'NONE',  ( 22.47829353779999906, -18.50000000000000000, 9.108151049139999955 ) ) ;
#26179 = CARTESIAN_POINT ( 'NONE',  ( -20.11613068700000184, -58.88287621140000283, 14.48562127070000116 ) ) ;
#26180 = ORIENTED_EDGE ( 'NONE', *, *, #10431, .T. ) ;
#26181 = CARTESIAN_POINT ( 'NONE',  ( 20.17093527805420194, -98.28141828962287718, -1.154278920403048803 ) ) ;
#26182 = CARTESIAN_POINT ( 'NONE',  ( -12.43709190490000083, -101.4829589650000088, -10.26829550889999965 ) ) ;
#26183 = AXIS2_PLACEMENT_3D ( 'NONE', #6336, #13023, #17423 ) ;
#26184 = FACE_OUTER_BOUND ( 'NONE', #5121, .T. ) ;
#26185 = CARTESIAN_POINT ( 'NONE',  ( -7.616929725699291609, -101.0610180770348450, 14.58800058767319463 ) ) ;
#26186 = VERTEX_POINT ( 'NONE', #7851 ) ;
#26187 = EDGE_CURVE ( 'NONE', #19071, #2738, #16453, .T. ) ;
#26188 = ADVANCED_FACE ( 'NONE', ( #3207 ), #6054, .F. ) ;
#26189 = CARTESIAN_POINT ( 'NONE',  ( 10.62674045640880216, -67.15683218464279491, -25.79505860454265687 ) ) ;
#26190 = CARTESIAN_POINT ( 'NONE',  ( -32.70383663730000734, -74.35538279870000622, -22.12063385180000097 ) ) ;
#26191 = CARTESIAN_POINT ( 'NONE',  ( -22.49429811570129445, -79.94329726548942006, -32.72109705105904709 ) ) ;
#26192 = ORIENTED_EDGE ( 'NONE', *, *, #6214, .T. ) ;
#26193 = ADVANCED_FACE ( 'NONE', ( #9881 ), #7936, .T. ) ;
#26194 = PRODUCT ( 'Coolant Impeller Vanes', 'Coolant Impeller Vanes', '', ( #2334 ) ) ;
#26195 = AXIS2_PLACEMENT_3D ( 'NONE', #21566, #14846, #25939 ) ;
#26196 = CARTESIAN_POINT ( 'NONE',  ( 36.83926799238049909, -79.61991127481498154, -14.53746107291068057 ) ) ;
#26197 = CARTESIAN_POINT ( 'NONE',  ( 6.665674591485936773, -101.1884902310438861, 14.93720712614567248 ) ) ;
#26198 = CARTESIAN_POINT ( 'NONE',  ( -0.6973805902349998753, -64.04267428580000399, -24.66993619630000012 ) ) ;
#26199 = ORIENTED_EDGE ( 'NONE', *, *, #25050, .F. ) ;
#26200 = CARTESIAN_POINT ( 'NONE',  ( -14.21627981196383139, -94.10917102368060227, -21.62117019558515452 ) ) ;
#26201 = VERTEX_POINT ( 'NONE', #14680 ) ;
#26202 = CARTESIAN_POINT ( 'NONE',  ( 20.60654921680000129, -56.26681992150000156, 10.91941308990000081 ) ) ;
#26203 = DIRECTION ( 'NONE',  ( 0.1241703988689521337, 0.000000000000000000, -0.9922609092596188507 ) ) ;
#26204 = CARTESIAN_POINT ( 'NONE',  ( 12.77500156440000012, -92.50000000000000000, 27.05403395929999988 ) ) ;
#26205 = ORIENTED_EDGE ( 'NONE', *, *, #16076, .F. ) ;
#26206 = CIRCLE ( 'NONE', #13148, 53.35000000000000142 ) ;
#26207 = DIRECTION ( 'NONE',  ( 0.4794255386042041156, 0.000000000000000000, 0.8775825618903722036 ) ) ;
#26208 = DIRECTION ( 'NONE',  ( 0.000000000000000000, 1.000000000000000000, 0.000000000000000000 ) ) ;
#26209 = EDGE_CURVE ( 'NONE', #24400, #54, #19563, .T. ) ;
#26210 = ORIENTED_EDGE ( 'NONE', *, *, #12606, .F. ) ;
#26211 = DIRECTION ( 'NONE',  ( 0.000000000000000000, -1.000000000000000000, 0.000000000000000000 ) ) ;
#26212 = CARTESIAN_POINT ( 'NONE',  ( -18.75204558950000333, -92.67327634539999792, -20.60858423150000363 ) ) ;
#26213 = CARTESIAN_POINT ( 'NONE',  ( 25.57708872518721677, -68.14490930545984781, 10.86928520380060448 ) ) ;
#26214 = EDGE_LOOP ( 'NONE', ( #15225, #22141, #14802, #10344 ) ) ;
#26215 = DIRECTION ( 'NONE',  ( 0.9952295494196654602, 0.000000000000000000, -0.09756097560976760563 ) ) ;
#26216 = CARTESIAN_POINT ( 'NONE',  ( 13.68203184070000233, -100.2522625769999962, -10.11858478029999908 ) ) ;
#26217 = CARTESIAN_POINT ( 'NONE',  ( 40.00000000000000000, -74.50000000000000000, 2.433892081919999696E-15 ) ) ;
#26218 = DIRECTION ( 'NONE',  ( -1.000000000000000000, 0.000000000000000000, 0.000000000000000000 ) ) ;
#26219 = CARTESIAN_POINT ( 'NONE',  ( 9.809109244645568992, -72.81435126429835236, -26.94740971970348653 ) ) ;
#26220 = CARTESIAN_POINT ( 'NONE',  ( -19.47573917819999778, -18.50000000000000000, 15.05374981759999997 ) ) ;
#26221 = VERTEX_POINT ( 'NONE', #23995 ) ;
#26223 = ADVANCED_FACE ( 'NONE', ( #15086, #21809 ), #6065, .F. ) ;
#26222 = FACE_OUTER_BOUND ( 'NONE', #3627, .T. ) ;
#26224 = FACE_OUTER_BOUND ( 'NONE', #6155, .T. ) ;
#26225 = DIRECTION ( 'NONE',  ( 0.000000000000000000, 1.000000000000000000, 0.000000000000000000 ) ) ;
#26226 = DIRECTION ( 'NONE',  ( 1.000000000000000000, 0.000000000000000000, 0.000000000000000000 ) ) ;
#26227 = CARTESIAN_POINT ( 'NONE',  ( -0.1866349815764706266, -92.68577957618185792, -30.49947259001435995 ) ) ;
#26228 = VECTOR ( 'NONE', #15442, 1000.000000000000000 ) ;
#26229 = CARTESIAN_POINT ( 'NONE',  ( -15.53338745080000116, -84.75000000000000000, -28.43367500519999780 ) ) ;
#26230 = EDGE_CURVE ( 'NONE', #26524, #28514, #16312, .T. ) ;
#26231 = DIRECTION ( 'NONE',  ( 0.4794255386042040601, 0.000000000000000000, 0.8775825618903720926 ) ) ;
#26232 = VERTEX_POINT ( 'NONE', #14946 ) ;
#26233 = CONICAL_SURFACE ( 'NONE', #8541, 13.13304743849999667, 0.9119902906770002149 ) ;
#26234 = CARTESIAN_POINT ( 'NONE',  ( 24.48469364033755369, -18.60777261479816502, 1.929692123232705558 ) ) ;
#26235 = ORIENTED_EDGE ( 'NONE', *, *, #10146, .T. ) ;
#26236 = CIRCLE ( 'NONE', #4849, 38.75000000000000000 ) ;
#26237 = CARTESIAN_POINT ( 'NONE',  ( 19.61885648609999677, -35.93737992959999872, -9.235927176200000588 ) ) ;
#26238 = DIRECTION ( 'NONE',  ( 1.000000000000000000, 0.000000000000000000, 0.000000000000000000 ) ) ;
#26239 = ORIENTED_EDGE ( 'NONE', *, *, #19218, .F. ) ;
#26240 = CARTESIAN_POINT ( 'NONE',  ( -12.66827223139999958, -101.1130130960000031, -8.801240666549999148 ) ) ;
#26241 = ADVANCED_FACE ( 'NONE', ( #24140 ), #25175, .F. ) ;
#26242 = CARTESIAN_POINT ( 'NONE',  ( -13.34153245340000105, -93.00000000000000000, 27.42724032409999779 ) ) ;
#26243 = CARTESIAN_POINT ( 'NONE',  ( 0.000000000000000000, -101.2530993010000060, 0.000000000000000000 ) ) ;
#26244 = CARTESIAN_POINT ( 'NONE',  ( -1.788617204129999916, -93.67869433870001217, 24.94025035040000304 ) ) ;
#26245 = EDGE_CURVE ( 'NONE', #18491, #8501, #5089, .T. ) ;
#26246 = CARTESIAN_POINT ( 'NONE',  ( -13.17060483900000101, -68.28989248250000799, -23.12790341000000183 ) ) ;
#26247 = CARTESIAN_POINT ( 'NONE',  ( 21.05852160049740007, -34.60505674903147622, -8.113043604740113324 ) ) ;
#26248 = AXIS2_PLACEMENT_3D ( 'NONE', #856, #27505, #14238 ) ;
#26249 = CARTESIAN_POINT ( 'NONE',  ( -11.21645807309999832, -18.61794787939999907, -18.51636674970000129 ) ) ;
#26250 = DIRECTION ( 'NONE',  ( 0.4438776720071309079, 0.000000000000000000, 0.8960873909912636659 ) ) ;
#26251 = ORIENTED_EDGE ( 'NONE', *, *, #11601, .F. ) ;
#26252 = DIRECTION ( 'NONE',  ( 0.000000000000000000, 1.000000000000000000, 0.000000000000000000 ) ) ;
#26253 = FACE_OUTER_BOUND ( 'NONE', #19372, .T. ) ;
#26254 = CARTESIAN_POINT ( 'NONE',  ( 22.63432516710000186, -65.53445078089998788, 11.44777113809999847 ) ) ;
#26255 = CARTESIAN_POINT ( 'NONE',  ( -16.40085562500000194, -100.7638431670000045, 3.096686113970000154 ) ) ;
#26256 = EDGE_LOOP ( 'NONE', ( #18001, #4664, #195, #4296 ) ) ;
#26257 = DIRECTION ( 'NONE',  ( 0.000000000000000000, 1.000000000000000000, 0.000000000000000000 ) ) ;
#26258 = EDGE_CURVE ( 'NONE', #842, #14037, #22114, .T. ) ;
#26259 = CARTESIAN_POINT ( 'NONE',  ( -15.12141716809999892, -79.25000000000000000, 36.76146410070000314 ) ) ;
#26260 = CARTESIAN_POINT ( 'NONE',  ( -13.30343089850000027, -92.51541830560000790, 26.96082632650000122 ) ) ;
#26261 = CARTESIAN_POINT ( 'NONE',  ( -50.00000000000000000, -15.00000000000000000, -2.486899575159999765E-14 ) ) ;
#26262 = VERTEX_POINT ( 'NONE', #10556 ) ;
#26263 = CARTESIAN_POINT ( 'NONE',  ( 26.37318901919999803, -93.00000450890000536, 13.16123549989999830 ) ) ;
#26264 = AXIS2_PLACEMENT_3D ( 'NONE', #18556, #25406, #5435 ) ;
#26265 = CARTESIAN_POINT ( 'NONE',  ( 0.9481071690910000127, -99.94549701829998867, -16.87515825230000033 ) ) ;
#26266 = CARTESIAN_POINT ( 'NONE',  ( 15.73111530680000314, -101.4254868690000109, 2.747748852119999974 ) ) ;
#26267 = CARTESIAN_POINT ( 'NONE',  ( 22.59576895060000012, -58.24783479010000065, 10.17368905969999915 ) ) ;
#26268 = CARTESIAN_POINT ( 'NONE',  ( 23.20779262239999596, -63.55510590220001177, -8.328310080079999622 ) ) ;
#26269 = VERTEX_POINT ( 'NONE', #8674 ) ;
#26270 = CARTESIAN_POINT ( 'NONE',  ( 6.377887625069999622, -101.0147083550000104, 14.18006541960000000 ) ) ;
#26271 = CARTESIAN_POINT ( 'NONE',  ( -16.09259912896104439, -92.55138318345946402, -24.01119014493966120 ) ) ;
#26272 = CARTESIAN_POINT ( 'NONE',  ( -3.982536363037985971, -95.75133628813770770, 22.38549364098651395 ) ) ;
#26273 = CIRCLE ( 'NONE', #23935, 5.000000000000000888 ) ;
#26274 = ORIENTED_EDGE ( 'NONE', *, *, #23120, .T. ) ;
#26275 = CARTESIAN_POINT ( 'NONE',  ( -39.90867856081912635, -65.74137084430174127, -2.178535352963598015 ) ) ;
#26276 = DIRECTION ( 'NONE',  ( -1.000000000000000000, 0.000000000000000000, 0.000000000000000000 ) ) ;
#26277 = CIRCLE ( 'NONE', #27221, 7.250000000000000000 ) ;
#26278 = CARTESIAN_POINT ( 'NONE',  ( 26.69293917519999937, -23.30310889129999907, 48.86109741659999628 ) ) ;
#26279 = ORIENTED_EDGE ( 'NONE', *, *, #28542, .T. ) ;
#26280 = CARTESIAN_POINT ( 'NONE',  ( 4.740176215359999112, -93.16461275549998788, -28.01390021799999985 ) ) ;
#26281 = DIRECTION ( 'NONE',  ( 0.000000000000000000, 1.000000000000000000, 0.000000000000000000 ) ) ;
#26282 = CARTESIAN_POINT ( 'NONE',  ( -13.14566783280000095, -99.53431386179998697, -11.42099844400000030 ) ) ;
#26283 = EDGE_LOOP ( 'NONE', ( #8821, #16543, #14571 ) ) ;
#26284 = DIRECTION ( 'NONE',  ( 1.000000000000000000, 0.000000000000000000, 0.000000000000000000 ) ) ;
#26285 = CARTESIAN_POINT ( 'NONE',  ( -12.72085913849602257, -100.6644468681186027, -10.92796509865996235 ) ) ;
#26286 = ORIENTED_EDGE ( 'NONE', *, *, #4342, .T. ) ;
#26287 = PRODUCT_DEFINITION ( 'UNKNOWN', '', #20401, #9458 ) ;
#26288 = CARTESIAN_POINT ( 'NONE',  ( 23.56065605869999757, -94.89197151660000884, -2.367189373290000010 ) ) ;
#26289 = EDGE_CURVE ( 'NONE', #28301, #8830, #19106, .T. ) ;
#26290 = CARTESIAN_POINT ( 'NONE',  ( -0.9479808564000000715, -101.5026188610000020, -15.99452317279999924 ) ) ;
#26291 = CARTESIAN_POINT ( 'NONE',  ( 22.06586088140000257, -18.85531889179999965, 0.4226866750830000075 ) ) ;
#26292 = CARTESIAN_POINT ( 'NONE',  ( 25.26718046270000073, -72.00000000000000000, 6.129403842640000377 ) ) ;
#26293 = CARTESIAN_POINT ( 'NONE',  ( 23.97384489419999909, -61.60336911379999947, -9.719973047129998989 ) ) ;
#26294 = DIRECTION ( 'NONE',  ( 0.000000000000000000, -1.000000000000000000, 0.000000000000000000 ) ) ;
#26295 = ORIENTED_EDGE ( 'NONE', *, *, #13176, .T. ) ;
#26296 = EDGE_CURVE ( 'NONE', #22947, #16053, #21899, .T. ) ;
#26297 = FACE_OUTER_BOUND ( 'NONE', #26982, .T. ) ;
#26298 = CARTESIAN_POINT ( 'NONE',  ( 16.32098426875123209, -94.64445995926946864, 17.22619538277506379 ) ) ;
#26299 = ADVANCED_FACE ( 'NONE', ( #28786, #15373 ), #6662, .T. ) ;
#26300 = CARTESIAN_POINT ( 'NONE',  ( -36.75091666766144982, -65.12255024416079152, 0.1339731005203242398 ) ) ;
#26301 = VECTOR ( 'NONE', #21201, 1000.000000000000000 ) ;
#26302 = DIRECTION ( 'NONE',  ( 0.000000000000000000, -1.000000000000000000, 0.000000000000000000 ) ) ;
#26303 = CARTESIAN_POINT ( 'NONE',  ( -18.48968691509886852, -19.46809228177112772, 12.68623665592749639 ) ) ;
#26304 = CARTESIAN_POINT ( 'NONE',  ( 7.670973119900000192, -34.59820496239999699, -21.21808926869999823 ) ) ;
#26305 = CARTESIAN_POINT ( 'NONE',  ( 43.75000000000000000, -79.00000000000000000, 5.357814579270000097E-15 ) ) ;
#26306 = ORIENTED_EDGE ( 'NONE', *, *, #5966, .F. ) ;
#26307 = CARTESIAN_POINT ( 'NONE',  ( 8.528769598780000294, -19.47487093119999813, -20.20034766559999895 ) ) ;
#26308 = CARTESIAN_POINT ( 'NONE',  ( -38.91454418380845937, -63.17361819573123682, 2.647414149835689567 ) ) ;
#26309 = ORIENTED_EDGE ( 'NONE', *, *, #21609, .F. ) ;
#26310 = CARTESIAN_POINT ( 'NONE',  ( -2.595813266009999953, -59.99252585180000352, -25.40064173880000098 ) ) ;
#26311 = DIRECTION ( 'NONE',  ( 0.000000000000000000, 1.000000000000000000, 0.000000000000000000 ) ) ;
#26312 = CARTESIAN_POINT ( 'NONE',  ( -19.91989157560000123, -56.26715181569999658, 12.12299716169999897 ) ) ;
#26313 = AXIS2_PLACEMENT_3D ( 'NONE', #20114, #4383, #24343 ) ;
#26314 = ORIENTED_EDGE ( 'NONE', *, *, #3341, .F. ) ;
#26315 = CARTESIAN_POINT ( 'NONE',  ( -19.83493014842161273, -96.36359511561902025, -9.389546401069701176 ) ) ;
#26316 = CARTESIAN_POINT ( 'NONE',  ( 7.248115061050000030, -74.24288085039999885, -40.37851622839999521 ) ) ;
#26317 = VERTEX_POINT ( 'NONE', #26623 ) ;
#26318 = DIRECTION ( 'NONE',  ( -0.5000000000009400258, 0.000000000000000000, -0.8660254037838960306 ) ) ;
#26319 = EDGE_CURVE ( 'NONE', #5884, #27002, #20042, .T. ) ;
#26320 = LINE ( 'NONE', #6498, #651 ) ;
#26321 = DIRECTION ( 'NONE',  ( -0.2414462220490753985, 0.000000000000000000, -0.9704142011833032377 ) ) ;
#26322 = EDGE_CURVE ( 'NONE', #4769, #12588, #13038, .T. ) ;
#26323 = DIRECTION ( 'NONE',  ( -0.2689078219309835593, 0.000000000000000000, 0.9631659168099411250 ) ) ;
#26324 = DIRECTION ( 'NONE',  ( 1.000000000000000000, 0.000000000000000000, 0.000000000000000000 ) ) ;
#26325 = CARTESIAN_POINT ( 'NONE',  ( -13.21936873900000009, -100.9405348700000076, -8.915374923630000836 ) ) ;
#26326 = ORIENTED_EDGE ( 'NONE', *, *, #10114, .T. ) ;
#26327 = DIRECTION ( 'NONE',  ( 0.000000000000000000, -1.000000000000000000, 0.000000000000000000 ) ) ;
#26328 = CARTESIAN_POINT ( 'NONE',  ( -12.15795451370000002, -100.5027207520000019, -10.78449129679999885 ) ) ;
#26329 = CARTESIAN_POINT ( 'NONE',  ( -14.65665286289999969, -74.50000000000000000, 36.94583910070000599 ) ) ;
#26330 = DIRECTION ( 'NONE',  ( 0.000000000000000000, 1.000000000000000000, 0.000000000000000000 ) ) ;
#26331 = ORIENTED_EDGE ( 'NONE', *, *, #9774, .T. ) ;
#26332 = CARTESIAN_POINT ( 'NONE',  ( -0.8253211953949340929, -101.6407018583229132, -15.98448082329617392 ) ) ;
#26333 = CARTESIAN_POINT ( 'NONE',  ( -32.09164647010000238, -74.00884812510000188, -22.02207427699999798 ) ) ;
#26334 = EDGE_LOOP ( 'NONE', ( #24602, #27592, #8753, #24587 ) ) ;
#26335 = CARTESIAN_POINT ( 'NONE',  ( 0.000000000000000000, 0.000000000000000000, 0.000000000000000000 ) ) ;
#26336 = AXIS2_PLACEMENT_3D ( 'NONE', #16693, #713, #16558 ) ;
#26337 = CARTESIAN_POINT ( 'NONE',  ( -17.54428855099999751, -94.59276292389999696, 16.07755916609999858 ) ) ;
#26338 = VERTEX_POINT ( 'NONE', #8544 ) ;
#26339 = CARTESIAN_POINT ( 'NONE',  ( -19.95527577780000072, -57.47855601759999900, 12.14622656770000120 ) ) ;
#26340 = CARTESIAN_POINT ( 'NONE',  ( -17.39460856262869370, -93.41743724412515348, -21.38387721846088496 ) ) ;
#26341 = VERTEX_POINT ( 'NONE', #21960 ) ;
#26342 = CARTESIAN_POINT ( 'NONE',  ( 26.00969437890000080, -92.68289734370000588, 10.63460028110000088 ) ) ;
#26343 = FACE_OUTER_BOUND ( 'NONE', #18177, .T. ) ;
#26344 =( REPRESENTATION_RELATIONSHIP ('NONE','NONE', #26008, #24690 ) REPRESENTATION_RELATIONSHIP_WITH_TRANSFORMATION ( #5391 )SHAPE_REPRESENTATION_RELATIONSHIP( ) );
#26345 = ORIENTED_EDGE ( 'NONE', *, *, #12586, .F. ) ;
#26346 = PLANE ( 'NONE',  #26664 ) ;
#26347 = CARTESIAN_POINT ( 'NONE',  ( -21.71458295470000266, -79.50000022099999342, -32.69645407760000211 ) ) ;
#26348 = ADVANCED_FACE ( 'NONE', ( #19759 ), #13342, .T. ) ;
#26349 = CARTESIAN_POINT ( 'NONE',  ( 8.645795245420000441, -37.33710341700000157, -21.88811428650000224 ) ) ;
#26350 = CARTESIAN_POINT ( 'NONE',  ( -18.90873350840000100, -92.90721294769998906, -21.12364821749999777 ) ) ;
#26351 = CARTESIAN_POINT ( 'NONE',  ( -2.125583358770000153, -18.50000000000000000, -21.40767207160000396 ) ) ;
#26352 = ORIENTED_EDGE ( 'NONE', *, *, #26367, .F. ) ;
#26353 = CARTESIAN_POINT ( 'NONE',  ( -6.045889172941522283, -101.5703832412493171, 14.87708822258295882 ) ) ;
#26354 = CARTESIAN_POINT ( 'NONE',  ( 13.78466514429999812, -99.94549701829998867, -9.780229041529999279 ) ) ;
#26355 = CARTESIAN_POINT ( 'NONE',  ( -19.64034669340000150, -92.70565393250001307, 20.70273603029999876 ) ) ;
#26356 = FACE_OUTER_BOUND ( 'NONE', #28020, .T. ) ;
#26357 = DIRECTION ( 'NONE',  ( 0.000000000000000000, 1.000000000000000000, 0.000000000000000000 ) ) ;
#26358 = CARTESIAN_POINT ( 'NONE',  ( 29.83826626095881451, -92.59055325466113118, 6.318856881893660571 ) ) ;
#26359 = DIRECTION ( 'NONE',  ( 1.000000000000000000, 0.000000000000000000, 0.000000000000000000 ) ) ;
#26360 = ORIENTED_EDGE ( 'NONE', *, *, #6207, .T. ) ;
#26361 = CARTESIAN_POINT ( 'NONE',  ( -38.25000000001202238, -63.17171877515667688, 2.272201163154965453 ) ) ;
#26362 = CARTESIAN_POINT ( 'NONE',  ( 7.992697598190521724, -57.47158968945384316, -22.16163068290176952 ) ) ;
#26363 = CARTESIAN_POINT ( 'NONE',  ( -23.92783087366071015, -92.71346081468063005, -18.91319433822785001 ) ) ;
#26364 = CARTESIAN_POINT ( 'NONE',  ( 19.97770600910000027, -18.50000000000000000, 8.668758119890000557 ) ) ;
#26365 = FACE_OUTER_BOUND ( 'NONE', #17057, .T. ) ;
#26366 = B_SPLINE_SURFACE_WITH_KNOTS ( 'NONE', 5, 5, ( 
 ( #11612, #3194, #1030, #25040, #20524, #12052 ),
 ( #20819, #593, #23287, #3060, #9586, #9723 ),
 ( #25472, #9436, #18486, #5074, #20967, #22865 ),
 ( #5227, #18343, #5372, #27796, #16285, #14524 ),
 ( #5507, #16439, #7419, #13959, #25342, #25198 ),
 ( #14255, #10003, #9869, #7270, #18917, #18634 ) ),
 .UNSPECIFIED., .F., .F., .F.,
 ( 6, 6 ),
 ( 6, 6 ),
 ( 38.86449171000000291, 46.02720679840000173 ),
 ( 0.000000000000000000, 2.000000000000000000 ),
 .UNSPECIFIED. ) ;
#26367 = EDGE_CURVE ( 'NONE', #3830, #10205, #5801, .T. ) ;
#26368 = PRODUCT_CONTEXT ( 'NONE', #16492, 'mechanical' ) ;
#26369 = CARTESIAN_POINT ( 'NONE',  ( 32.97008227039999895, -72.00000000000000000, -20.36016146999999776 ) ) ;
#26370 = DIRECTION ( 'NONE',  ( 0.000000000000000000, 1.000000000000000000, 0.000000000000000000 ) ) ;
#26371 = ORIENTED_EDGE ( 'NONE', *, *, #24795, .T. ) ;
#26372 = CARTESIAN_POINT ( 'NONE',  ( 22.63183994989999803, -96.16784750700000473, -4.383698213610000671 ) ) ;
#26373 = ORIENTED_EDGE ( 'NONE', *, *, #28400, .F. ) ;
#26374 = CARTESIAN_POINT ( 'NONE',  ( 20.49450488670000325, -35.98895400249999454, -8.959583261280000599 ) ) ;
#26375 = CARTESIAN_POINT ( 'NONE',  ( 7.730596333266516851, -19.15810973048309052, -20.62158076667584439 ) ) ;
#26376 = EDGE_LOOP ( 'NONE', ( #17941, #8914, #11602, #20252 ) ) ;
#26377 = CARTESIAN_POINT ( 'NONE',  ( 15.54119309900000090, -100.8869817940000075, 1.981729577500000339 ) ) ;
#26378 = EDGE_CURVE ( 'NONE', #20895, #7380, #11641, .T. ) ;
#26379 = EDGE_CURVE ( 'NONE', #9130, #5488, #2598, .T. ) ;
#26380 = DIRECTION ( 'NONE',  ( 1.000000000000000000, 0.000000000000000000, 0.000000000000000000 ) ) ;
#26381 = CARTESIAN_POINT ( 'NONE',  ( -11.27245849040000003, -95.14589738820001230, -21.35309096379999971 ) ) ;
#26382 = B_SPLINE_CURVE_WITH_KNOTS ( 'NONE', 5,
 ( #5374, #16289, #23012, #14257, #2758, #23151 ),
 .UNSPECIFIED., .F., .F.,
 ( 6, 6 ),
 ( 0.000000000000000000, 1.000000000000000000 ),
 .UNSPECIFIED. ) ;
#26383 = CARTESIAN_POINT ( 'NONE',  ( -14.42556421679999978, -111.0000000000000000, -2.978755036369999942 ) ) ;
#26384 = CARTESIAN_POINT ( 'NONE',  ( 9.564509902250000195, -57.40875702419999982, -23.52622212079999997 ) ) ;
#26385 = CARTESIAN_POINT ( 'NONE',  ( -10.96210381709999915, -19.46434222019999893, -19.17795744089999843 ) ) ;
#26386 = CARTESIAN_POINT ( 'NONE',  ( 28.54979082390000045, -36.85000000000000142, 52.26004156059999417 ) ) ;
#26387 = ORIENTED_EDGE ( 'NONE', *, *, #4641, .F. ) ;
#26388 = CARTESIAN_POINT ( 'NONE',  ( 12.90947517493721719, -101.3586211803441159, -9.827147021456303477 ) ) ;
#26389 = CARTESIAN_POINT ( 'NONE',  ( 24.50968349569999916, -49.82767789679999737, 1.331815368300000024 ) ) ;
#26390 = CARTESIAN_POINT ( 'NONE',  ( 23.42457832669999718, -66.42763100729999337, 11.17107935629999993 ) ) ;
#26391 = CARTESIAN_POINT ( 'NONE',  ( -16.14211878319999727, -101.0779259520000011, 3.133147776259999961 ) ) ;
#26392 = ORIENTED_EDGE ( 'NONE', *, *, #15467, .F. ) ;
#26393 = DIRECTION ( 'NONE',  ( 0.000000000000000000, 1.000000000000000000, 0.000000000000000000 ) ) ;
#26394 = CARTESIAN_POINT ( 'NONE',  ( -14.44303431870000054, -92.83816993439999976, 26.18160581060000069 ) ) ;
#26395 = DIRECTION ( 'NONE',  ( -1.887379141859999978E-15, 0.000000000000000000, -1.000000000000000000 ) ) ;
#26396 = ORIENTED_EDGE ( 'NONE', *, *, #8190, .T. ) ;
#26397 = TOROIDAL_SURFACE ( 'NONE', #6878, 10.00000000000000000, 1.000000000000000000 ) ;
#26398 = LINE ( 'NONE', #6427, #24896 ) ;
#26399 = CARTESIAN_POINT ( 'NONE',  ( 0.3642957135809999913, -101.1412505549999992, -16.16346332520000217 ) ) ;
#26400 = CARTESIAN_POINT ( 'NONE',  ( -40.65853658540000026, -84.00000000000000000, 6.717799458580000049 ) ) ;
#26401 = CARTESIAN_POINT ( 'NONE',  ( -13.17786140689999819, -69.76368794990000310, -23.89400643789999990 ) ) ;
#26402 = CARTESIAN_POINT ( 'NONE',  ( -9.476764215410000247, -82.25000000000000000, 38.08875739639999836 ) ) ;
#26403 = TOROIDAL_SURFACE ( 'NONE', #13845, 39.75000000000000000, 0.5000000000000000000 ) ;
#26404 = CARTESIAN_POINT ( 'NONE',  ( 22.72361805330000095, -62.11544144339999463, -7.859435617799999996 ) ) ;
#26405 = ORIENTED_EDGE ( 'NONE', *, *, #16120, .F. ) ;
#26406 = CARTESIAN_POINT ( 'NONE',  ( -40.00000000000000000, -69.00000000000000000, 5.717648576820000312E-16 ) ) ;
#26407 = CARTESIAN_POINT ( 'NONE',  ( 14.93581056110000027, -101.1848541609999899, 3.234659781990000038 ) ) ;
#26408 = CONICAL_SURFACE ( 'NONE', #21746, 55.67692378859999280, 1.047197551199999799 ) ;
#26409 = CARTESIAN_POINT ( 'NONE',  ( -6.649722661318385519, -98.16872833778059260, 18.49410160609588871 ) ) ;
#26410 = ORIENTED_EDGE ( 'NONE', *, *, #10370, .F. ) ;
#26411 = CARTESIAN_POINT ( 'NONE',  ( 27.93493094108533015, -92.53708507728566701, 12.24300196966718168 ) ) ;
#26412 = CARTESIAN_POINT ( 'NONE',  ( 4.659867367963298257, -92.75430643208848380, -30.14196855148737342 ) ) ;
#26413 = CARTESIAN_POINT ( 'NONE',  ( -5.273680924649999824, -107.3487944130000074, -9.653408180790000515 ) ) ;
#26414 = VERTEX_POINT ( 'NONE', #11444 ) ;
#26415 = CARTESIAN_POINT ( 'NONE',  ( 20.47275178710000176, -93.13207089429998575, 16.42312355550000191 ) ) ;
#26416 = CIRCLE ( 'NONE', #13383, 5.500000000000000000 ) ;
#26417 = CARTESIAN_POINT ( 'NONE',  ( 19.39107742150000036, -19.48263940080000012, -8.982220567580000647 ) ) ;
#26418 = CARTESIAN_POINT ( 'NONE',  ( -9.476764215410000247, -82.25000000000000000, -38.08875739639999836 ) ) ;
#26419 = CARTESIAN_POINT ( 'NONE',  ( -6.736536556819999966, -101.1716782170000073, 14.21895496870000031 ) ) ;
#26420 = ORIENTED_EDGE ( 'NONE', *, *, #28680, .F. ) ;
#26421 = CIRCLE ( 'NONE', #17579, 34.89999999999999858 ) ;
#26422 = CARTESIAN_POINT ( 'NONE',  ( 2.042810365310000056E-12, -74.50000000000000000, -2.458477865729999957E-12 ) ) ;
#26423 = CARTESIAN_POINT ( 'NONE',  ( -12.57887770961745844, -100.9364580245582488, -10.76270985140424052 ) ) ;
#26424 = ORIENTED_EDGE ( 'NONE', *, *, #26126, .F. ) ;
#26425 = FACE_OUTER_BOUND ( 'NONE', #11695, .T. ) ;
#26426 = CARTESIAN_POINT ( 'NONE',  ( 24.80237488970000115, -93.63284696290000397, -3.743705429929999884 ) ) ;
#26427 = ORIENTED_EDGE ( 'NONE', *, *, #23979, .T. ) ;
#26428 = CARTESIAN_POINT ( 'NONE',  ( -1.262698870129999928, -100.9763228559999959, -15.63141515150000238 ) ) ;
#26429 = CARTESIAN_POINT ( 'NONE',  ( 28.97576656849999566, -36.00000000000000000, -19.97576656850000987 ) ) ;
#26430 = CARTESIAN_POINT ( 'NONE',  ( -12.00629479391328225, -19.46993812760626952, 19.10789507585830194 ) ) ;
#26431 = CARTESIAN_POINT ( 'NONE',  ( 25.26718046270000073, -18.50000000000000000, 6.129403842640000377 ) ) ;
#26432 = CARTESIAN_POINT ( 'NONE',  ( -19.51268635637469373, -92.50000000000000000, -23.44173519759771906 ) ) ;
#26433 = AXIS2_PLACEMENT_3D ( 'NONE', #27589, #5562, #25255 ) ;
#26434 = ORIENTED_EDGE ( 'NONE', *, *, #4942, .F. ) ;
#26435 = CARTESIAN_POINT ( 'NONE',  ( -16.67828388959999941, -80.00000000000000000, 44.75374114529999758 ) ) ;
#26436 = CARTESIAN_POINT ( 'NONE',  ( 19.66445149499999800, -18.50000000000000000, -7.467233996350000069 ) ) ;
#26437 = CARTESIAN_POINT ( 'NONE',  ( -36.70000763062214588, -65.09474816373202088, -0.01998728352818625667 ) ) ;
#26438 = PRODUCT ( 'Water Pump Main Cast Housing', 'Water Pump Main Cast Housing', '', ( #18064 ) ) ;
#26439 = CARTESIAN_POINT ( 'NONE',  ( 13.68659840514571613, -100.3041487038156134, -10.18120984587954503 ) ) ;
#26440 = CARTESIAN_POINT ( 'NONE',  ( -17.80822692750000158, -101.1889999979999999, -18.25149456069999943 ) ) ;
#26441 = CARTESIAN_POINT ( 'NONE',  ( 7.857545609690000710, -34.84004015499999696, -21.18059969839999823 ) ) ;
#26442 = DIRECTION ( 'NONE',  ( 0.000000000000000000, 1.000000000000000000, 0.000000000000000000 ) ) ;
#26443 = ORIENTED_EDGE ( 'NONE', *, *, #19304, .F. ) ;
#26444 = CARTESIAN_POINT ( 'NONE',  ( 9.024081076579999916, -19.18584067659999803, -18.94592230760000007 ) ) ;
#26445 = CIRCLE ( 'NONE', #14795, 0.4999999999999988343 ) ;
#26446 = VECTOR ( 'NONE', #27802, 1000.000000000000000 ) ;
#26447 = DIRECTION ( 'NONE',  ( 0.000000000000000000, 1.000000000000000000, 0.000000000000000000 ) ) ;
#26448 = EDGE_CURVE ( 'NONE', #1187, #400, #20500, .T. ) ;
#26449 = CARTESIAN_POINT ( 'NONE',  ( -12.06159505309999957, -57.47122572379999639, 20.23241877790000132 ) ) ;
#26450 = B_SPLINE_CURVE_WITH_KNOTS ( 'NONE', 3,
 ( #7175, #27279, #7314, #24800, #11512, #11367 ),
 .UNSPECIFIED., .F., .F.,
 ( 4, 2, 4 ),
 ( 0.000000000000000000, 0.5000000000000000000, 1.000000000000000000 ),
 .UNSPECIFIED. ) ;
#26451 = EDGE_CURVE ( 'NONE', #5596, #17070, #18662, .T. ) ;
#26452 = CARTESIAN_POINT ( 'NONE',  ( -24.74383412450000108, -93.85715850789999593, -2.800417634270000011 ) ) ;
#26453 = CARTESIAN_POINT ( 'NONE',  ( -19.61988232110000041, -56.24740423709999249, 13.61851891309999907 ) ) ;
#26454 = ADVANCED_FACE ( 'NONE', ( #7111 ), #2448, .T. ) ;
#26455 = CARTESIAN_POINT ( 'NONE',  ( 27.68682485439999752, -24.80000000000000071, 50.68039294919999804 ) ) ;
#26456 = CARTESIAN_POINT ( 'NONE',  ( 15.98896817450000007, -100.8088109309999965, 4.269801629269999843 ) ) ;
#26457 = VERTEX_POINT ( 'NONE', #27067 ) ;
#26458 = LINE ( 'NONE', #28344, #16288 ) ;
#26459 = CARTESIAN_POINT ( 'NONE',  ( 7.305188533800000883, -74.19145175580000284, -39.89376887110000069 ) ) ;
#26460 = ORIENTED_EDGE ( 'NONE', *, *, #18441, .F. ) ;
#26461 = CARTESIAN_POINT ( 'NONE',  ( -7.627568735119999666, -74.00000000000000000, 38.62788659690000515 ) ) ;
#26462 = AXIS2_PLACEMENT_3D ( 'NONE', #24131, #13486, #17580 ) ;
#26463 = DIRECTION ( 'NONE',  ( 0.000000000000000000, -1.000000000000000000, 0.000000000000000000 ) ) ;
#26464 = VECTOR ( 'NONE', #15919, 1000.000000000000114 ) ;
#26465 = CARTESIAN_POINT ( 'NONE',  ( 22.48256761629999900, -26.02764329579999725, 9.981120560429999955 ) ) ;
#26466 = FACE_BOUND ( 'NONE', #3227, .T. ) ;
#26467 = CARTESIAN_POINT ( 'NONE',  ( 10.10280028159999866, -66.03737782630000197, -24.89219399830000157 ) ) ;
#26468 = ORIENTED_EDGE ( 'NONE', *, *, #27498, .F. ) ;
#26469 = CARTESIAN_POINT ( 'NONE',  ( -15.08135542264446016, -67.66819112664462921, 22.63088101126209040 ) ) ;
#26470 = CARTESIAN_POINT ( 'NONE',  ( -12.17069681629999955, -101.1292389600000092, -9.608835620689999857 ) ) ;
#26471 = CARTESIAN_POINT ( 'NONE',  ( -7.226919149556380262, -73.65985332689392351, 39.42193790014463417 ) ) ;
#26472 = CARTESIAN_POINT ( 'NONE',  ( 23.27528716992228297, -63.28488723400939620, -7.442304005261173749 ) ) ;
#26473 = VERTEX_POINT ( 'NONE', #1813 ) ;
#26474 = AXIS2_PLACEMENT_3D ( 'NONE', #28801, #4187, #24155 ) ;
#26475 = DIRECTION ( 'NONE',  ( 1.000000000000000000, 0.000000000000000000, 0.000000000000000000 ) ) ;
#26476 = CARTESIAN_POINT ( 'NONE',  ( -32.66462566889999408, -74.35538279870000622, -21.73251009970000069 ) ) ;
#26477 = CARTESIAN_POINT ( 'NONE',  ( -22.37091525677837467, -79.85009384193479320, -32.77535131886410369 ) ) ;
#26478 = ORIENTED_EDGE ( 'NONE', *, *, #234, .F. ) ;
#26480 = EDGE_CURVE ( 'NONE', #1234, #12823, #15343, .T. ) ;
#26479 = AXIS2_PLACEMENT_3D ( 'NONE', #28109, #14290, #21000 ) ;
#26481 = VECTOR ( 'NONE', #21983, 1000.000000000000000 ) ;
#26482 = AXIS2_PLACEMENT_3D ( 'NONE', #3155, #21479, #19296 ) ;
#26483 = DIRECTION ( 'NONE',  ( 0.000000000000000000, 1.000000000000000000, 0.000000000000000000 ) ) ;
#26484 = B_SPLINE_CURVE_WITH_KNOTS ( 'NONE', 5,
 ( #17028, #12228, #25917, #21136, #19359, #21824 ),
 .UNSPECIFIED., .F., .F.,
 ( 6, 6 ),
 ( -3.225498864409999999, -2.709627234730000112 ),
 .UNSPECIFIED. ) ;
#26485 = EDGE_CURVE ( 'NONE', #18453, #15088, #6615, .T. ) ;
#26486 = ORIENTED_EDGE ( 'NONE', *, *, #26826, .T. ) ;
#26487 = CARTESIAN_POINT ( 'NONE',  ( 41.00000000000000000, -80.00000000000000000, -10.20110288159999890 ) ) ;
#26488 = VERTEX_POINT ( 'NONE', #24241 ) ;
#26489 = CARTESIAN_POINT ( 'NONE',  ( 19.94073578940000147, -94.89419905519999077, 14.19046457500000002 ) ) ;
#26490 = DIRECTION ( 'NONE',  ( 1.000000000000000000, 0.000000000000000000, 0.000000000000000000 ) ) ;
#26491 = EDGE_LOOP ( 'NONE', ( #23602, #15696, #7886, #14113 ) ) ;
#26492 = CARTESIAN_POINT ( 'NONE',  ( -42.17917380793182502, -65.66662781299496032, 0.7655265227419015828 ) ) ;
#26493 = CARTESIAN_POINT ( 'NONE',  ( 31.00000000000000000, -13.00000000000000000, 4.500000000000000000 ) ) ;
#26494 = AXIS2_PLACEMENT_3D ( 'NONE', #23061, #22618, #3607 ) ;
#26495 = CARTESIAN_POINT ( 'NONE',  ( 11.92167937070000150, -101.1848541609999899, -9.561966123969998677 ) ) ;
#26496 = CARTESIAN_POINT ( 'NONE',  ( 7.215414233289999757, -77.00000000000000000, -40.70731707320000226 ) ) ;
#26497 = ORIENTED_EDGE ( 'NONE', *, *, #11712, .F. ) ;
#26498 = CIRCLE ( 'NONE', #1400, 7.250000000000000000 ) ;
#26499 = TOROIDAL_SURFACE ( 'NONE', #23273, 39.75000000000000000, 0.5000000000000000000 ) ;
#26500 = CARTESIAN_POINT ( 'NONE',  ( -1.247133441849999969, -101.2306315440000049, -16.16540283980000225 ) ) ;
#26501 = CARTESIAN_POINT ( 'NONE',  ( 12.59582948049999906, -101.5964542560000012, -9.931670464719999813 ) ) ;
#26502 = DIRECTION ( 'NONE',  ( 0.000000000000000000, 1.000000000000000000, 0.000000000000000000 ) ) ;
#26503 = CARTESIAN_POINT ( 'NONE',  ( -0.5388777241750000169, -56.26715181569999658, -23.31263072600000186 ) ) ;
#26504 = CARTESIAN_POINT ( 'NONE',  ( 21.32348952719999957, -36.24018116390000444, -9.136262768950000890 ) ) ;
#26505 = DIRECTION ( 'NONE',  ( 0.4692400087391608854, 0.000000000000000000, -0.8830706733883039172 ) ) ;
#26506 = EDGE_LOOP ( 'NONE', ( #7586, #28654, #16747, #27768 ) ) ;
#26507 = CARTESIAN_POINT ( 'NONE',  ( -21.99985828019999801, -74.00000000000000000, -31.89935321680000158 ) ) ;
#26508 = CARTESIAN_POINT ( 'NONE',  ( -7.615241770509999806E-12, -84.50000000000000000, -9.798384326129999571E-12 ) ) ;
#26509 = DIRECTION ( 'NONE',  ( 0.4794255386042000078, 0.000000000000000000, 0.8775825618903743131 ) ) ;
#26510 = CARTESIAN_POINT ( 'NONE',  ( 22.62497689329999773, -18.50000000000000000, 8.848724866619999574 ) ) ;
#26511 = CARTESIAN_POINT ( 'NONE',  ( -1.044063374772672637, -92.50630337894764921, -30.48240144424680409 ) ) ;
#26512 = EDGE_CURVE ( 'NONE', #4763, #24745, #1435, .T. ) ;
#26513 = CARTESIAN_POINT ( 'NONE',  ( 0.000000000000000000, 0.000000000000000000, 0.000000000000000000 ) ) ;
#26514 = CARTESIAN_POINT ( 'NONE',  ( -11.51095449373275237, -94.71798490447446284, -20.64293826046422353 ) ) ;
#26515 = FACE_OUTER_BOUND ( 'NONE', #17295, .T. ) ;
#26516 = CIRCLE ( 'NONE', #12122, 3.749999999999996447 ) ;
#26517 = ADVANCED_FACE ( 'NONE', ( #17540 ), #46, .F. ) ;
#26518 = AXIS2_PLACEMENT_3D ( 'NONE', #11119, #18147, #13770 ) ;
#26519 = EDGE_LOOP ( 'NONE', ( #9089, #532, #21537, #13278 ) ) ;
#26520 = CARTESIAN_POINT ( 'NONE',  ( 23.48647108369999614, -94.80026829410000744, -6.710788097320000034 ) ) ;
#26521 = ORIENTED_EDGE ( 'NONE', *, *, #20226, .F. ) ;
#26522 = DIRECTION ( 'NONE',  ( 1.000000000000000000, 0.000000000000000000, 0.000000000000000000 ) ) ;
#26523 = DIRECTION ( 'NONE',  ( 0.000000000000000000, -1.000000000000000000, 0.000000000000000000 ) ) ;
#26524 = VERTEX_POINT ( 'NONE', #26429 ) ;
#26525 = ORIENTED_EDGE ( 'NONE', *, *, #4603, .T. ) ;
#26526 = DIRECTION ( 'NONE',  ( 1.000000000000000000, 0.000000000000000000, 0.000000000000000000 ) ) ;
#26527 = CARTESIAN_POINT ( 'NONE',  ( 40.00000000000000000, -74.00000000000000000, 2.009834509230000106E-15 ) ) ;
#26528 = CARTESIAN_POINT ( 'NONE',  ( -17.00245937369999893, -99.64579666810000447, 3.307441295489999877 ) ) ;
#26529 = CARTESIAN_POINT ( 'NONE',  ( -29.52258421500394547, -92.52048598158022230, 7.659457213237817363 ) ) ;
#26530 = CARTESIAN_POINT ( 'NONE',  ( -40.09372830037592195, -65.74402527486655856, 2.175418052786639134 ) ) ;
#26531 = ORIENTED_EDGE ( 'NONE', *, *, #1186, .T. ) ;
#26532 = CARTESIAN_POINT ( 'NONE',  ( 8.712840316590000356, -92.70565333729999224, -27.17408075339999840 ) ) ;
#26533 = CARTESIAN_POINT ( 'NONE',  ( 23.19209251300000219, -34.65282384500000035, 0.9632692026179999756 ) ) ;
#26534 = CARTESIAN_POINT ( 'NONE',  ( -14.75020709650109474, -80.11189707592339460, 36.37309920249453654 ) ) ;
#26535 = CARTESIAN_POINT ( 'NONE',  ( 40.26982517594145605, -74.16605908717274076, 7.244980372392263668 ) ) ;
#26536 = VERTEX_POINT ( 'NONE', #10807 ) ;
#26537 = CIRCLE ( 'NONE', #4189, 8.000000000000000000 ) ;
#26538 = CYLINDRICAL_SURFACE ( 'NONE', #13664, 7.249999999999999112 ) ;
#26539 = CARTESIAN_POINT ( 'NONE',  ( -16.91317841180000059, -92.93841875540000785, 21.66141092870000051 ) ) ;
#26540 = DIRECTION ( 'NONE',  ( 1.000000000000000000, 0.000000000000000000, 0.000000000000000000 ) ) ;
#26541 = ORIENTED_EDGE ( 'NONE', *, *, #742, .F. ) ;
#26542 = AXIS2_PLACEMENT_3D ( 'NONE', #19291, #6158, #26135 ) ;
#26543 = CARTESIAN_POINT ( 'NONE',  ( 28.18645782309999959, -71.82886645399999281, 1.608671017380000068 ) ) ;
#26544 = VECTOR ( 'NONE', #12067, 999.9999999999998863 ) ;
#26545 = B_SPLINE_CURVE_WITH_KNOTS ( 'NONE', 5,
 ( #28288, #5592, #23370, #12406, #3965, #12826 ),
 .UNSPECIFIED., .F., .F.,
 ( 6, 6 ),
 ( 0.000000000000000000, 1.000000000000000000 ),
 .UNSPECIFIED. ) ;
#26546 = CARTESIAN_POINT ( 'NONE',  ( 0.2736767326270000411, -101.4829589650000088, -16.12588753389999852 ) ) ;
#26547 = CARTESIAN_POINT ( 'NONE',  ( 7.992697598190001251, -57.47158968939999824, -22.16163068290000027 ) ) ;
#26548 = CARTESIAN_POINT ( 'NONE',  ( -25.98617420859999783, -74.50000000000000000, -36.59277592640000165 ) ) ;
#26549 = CARTESIAN_POINT ( 'NONE',  ( -11.90992095799999895, -57.47815921199999423, -20.09952916750000185 ) ) ;
#26550 = ORIENTED_EDGE ( 'NONE', *, *, #4914, .T. ) ;
#26551 = ADVANCED_FACE ( 'NONE', ( #15626 ), #12563, .T. ) ;
#26552 = ADVANCED_FACE ( 'NONE', ( #15474 ), #4562, .F. ) ;
#26553 = CARTESIAN_POINT ( 'NONE',  ( 28.63360765790000073, -72.82938648530000592, 1.697648101029999967 ) ) ;
#26554 = ADVANCED_FACE ( 'NONE', ( #19851 ), #23623, .T. ) ;
#26555 = ORIENTED_EDGE ( 'NONE', *, *, #25362, .F. ) ;
#26556 = CARTESIAN_POINT ( 'NONE',  ( 28.21594761775847715, -92.66777315148628702, 11.58060234458442395 ) ) ;
#26557 = CARTESIAN_POINT ( 'NONE',  ( 27.68682485439999752, -35.29999999999999716, 50.68039294919999804 ) ) ;
#26558 = CARTESIAN_POINT ( 'NONE',  ( -42.12502810473512227, -65.68892072177348496, -0.8034381443789905264 ) ) ;
#26559 = CIRCLE ( 'NONE', #60, 16.00000000000000000 ) ;
#26560 = DIRECTION ( 'NONE',  ( 0.000000000000000000, 1.000000000000000000, 0.000000000000000000 ) ) ;
#26561 = AXIS2_PLACEMENT_3D ( 'NONE', #14, #6557, #26665 ) ;
#26562 = VECTOR ( 'NONE', #22595, 1000.000000000000000 ) ;
#26563 = CARTESIAN_POINT ( 'NONE',  ( 20.47344018690000311, -19.43778597749999903, -8.153551334750000379 ) ) ;
#26564 = DIRECTION ( 'NONE',  ( 0.000000000000000000, -1.000000000000000000, 0.000000000000000000 ) ) ;
#26565 = EDGE_LOOP ( 'NONE', ( #11524, #27575, #7252, #24480 ) ) ;
#26566 = DIRECTION ( 'NONE',  ( 0.000000000000000000, 0.000000000000000000, -1.000000000000000000 ) ) ;
#26567 = CARTESIAN_POINT ( 'NONE',  ( -12.86054043281202830, -100.4507315467552928, -11.02681200338788337 ) ) ;
#26568 = ORIENTED_EDGE ( 'NONE', *, *, #20681, .T. ) ;
#26569 = CARTESIAN_POINT ( 'NONE',  ( 7.659450882289999818, -36.59067043469999447, -21.46971212389999906 ) ) ;
#26570 = CARTESIAN_POINT ( 'NONE',  ( 24.59609816880000110, -94.07620464469999888, -4.012350405089999406 ) ) ;
#26571 = CARTESIAN_POINT ( 'NONE',  ( -12.09704001540000107, -74.00000000000000000, 47.10905722069999513 ) ) ;
#26572 = EDGE_CURVE ( 'NONE', #20017, #3141, #11250, .T. ) ;
#26573 = CARTESIAN_POINT ( 'NONE',  ( -40.00000000000000000, -63.40192378860000133, 0.000000000000000000 ) ) ;
#26574 = CARTESIAN_POINT ( 'NONE',  ( -0.8216735279219999910, -65.07443093669999712, -25.13632616349999793 ) ) ;
#26575 = DIRECTION ( 'NONE',  ( 1.000000000000000000, 0.000000000000000000, 0.000000000000000000 ) ) ;
#26576 = CARTESIAN_POINT ( 'NONE',  ( -15.29367271319999766, -101.2995961670000042, 4.428833737689999772 ) ) ;
#26577 = CARTESIAN_POINT ( 'NONE',  ( -12.76410956269999986, -19.16887614239999849, 19.36424863110000061 ) ) ;
#26578 = CARTESIAN_POINT ( 'NONE',  ( 0.000000000000000000, -39.32601556110000018, 0.000000000000000000 ) ) ;
#26579 = CARTESIAN_POINT ( 'NONE',  ( -36.79999999999999716, -65.14977478849999670, -0.1732050807570000017 ) ) ;
#26580 = CARTESIAN_POINT ( 'NONE',  ( 36.24656966590000451, -75.00000018780001199, -15.05817676390000059 ) ) ;
#26581 = CARTESIAN_POINT ( 'NONE',  ( 25.74462086831581686, -61.40640411929997100, 1.403327536049160607 ) ) ;
#26582 = CARTESIAN_POINT ( 'NONE',  ( -38.26719868119548806, -65.11500191527169079, -2.767150539682058152 ) ) ;
#26583 = CARTESIAN_POINT ( 'NONE',  ( -4.500000000000000000, 0.000000000000000000, 31.00000000000000000 ) ) ;
#26584 = CARTESIAN_POINT ( 'NONE',  ( -14.40572000550000098, -18.50000000000000000, 20.06574520719999910 ) ) ;
#26585 = VECTOR ( 'NONE', #1238, 1000.000000000000000 ) ;
#26586 = VERTEX_POINT ( 'NONE', #522 ) ;
#26587 = VECTOR ( 'NONE', #23614, 999.9999999999998863 ) ;
#26588 = CARTESIAN_POINT ( 'NONE',  ( 8.979483994470001562, -19.17889721279999904, -19.39105717750000224 ) ) ;
#26589 = EDGE_CURVE ( 'NONE', #23041, #16053, #16816, .T. ) ;
#26590 = CIRCLE ( 'NONE', #22345, 0.5000000000000027756 ) ;
#26591 = B_SPLINE_CURVE_WITH_KNOTS ( 'NONE', 5,
 ( #14857, #24, #22296, #11645, #27119, #11798, #20256, #13843, #20403 ),
 .UNSPECIFIED., .F., .F.,
 ( 6, 3, 6 ),
 ( 0.000000000000000000, 0.5538417791012780755, 1.000000000000000000 ),
 .UNSPECIFIED. ) ;
#26592 = CARTESIAN_POINT ( 'NONE',  ( 22.70474501079999641, -37.36473932629999695, -9.382534168720001233 ) ) ;
#26593 = CARTESIAN_POINT ( 'NONE',  ( -11.45174903020000023, -57.47815880419999957, 20.36405811959999923 ) ) ;
#26594 = CARTESIAN_POINT ( 'NONE',  ( 7.230685509108649711, -74.36482065571902922, 40.53346806358988630 ) ) ;
#26595 = CARTESIAN_POINT ( 'NONE',  ( -24.11720358960000254, -94.18458606759999441, -3.273744814500000100 ) ) ;
#26596 = CARTESIAN_POINT ( 'NONE',  ( -19.65023616090000047, -56.26441942339999969, 12.67997976360000045 ) ) ;
#26597 = DIRECTION ( 'NONE',  ( 0.000000000000000000, 1.000000000000000000, 0.000000000000000000 ) ) ;
#26598 = VERTEX_POINT ( 'NONE', #13595 ) ;
#26599 = PRESENTATION_STYLE_ASSIGNMENT (( #24710 ) ) ;
#26600 = CARTESIAN_POINT ( 'NONE',  ( -13.46646099420000020, -101.3150700380000018, -9.098099534850002001 ) ) ;
#26601 = ORIENTED_EDGE ( 'NONE', *, *, #25050, .T. ) ;
#26602 = TOROIDAL_SURFACE ( 'NONE', #21488, 55.85192378860000417, 0.3499999999999999778 ) ;
#26603 = CARTESIAN_POINT ( 'NONE',  ( 7.748442867550313196, -92.52498922770500656, 29.49944529545556904 ) ) ;
#26604 = AXIS2_PLACEMENT_3D ( 'NONE', #23483, #19104, #15259 ) ;
#26605 = CARTESIAN_POINT ( 'NONE',  ( 0.4666096705872683770, -99.76647888976904710, -17.31214626689192215 ) ) ;
#26606 = EDGE_CURVE ( 'NONE', #2986, #28714, #22862, .T. ) ;
#26607 = CARTESIAN_POINT ( 'NONE',  ( 22.31047812949999809, -45.95149559400000072, 9.984808736899998038 ) ) ;
#26608 = DIRECTION ( 'NONE',  ( 0.000000000000000000, 1.000000000000000000, 0.000000000000000000 ) ) ;
#26609 = CARTESIAN_POINT ( 'NONE',  ( 24.73793100160000336, -93.48569568790000517, -11.30322088119999968 ) ) ;
#26610 = EDGE_CURVE ( 'NONE', #14702, #2354, #22646, .T. ) ;
#26611 = CARTESIAN_POINT ( 'NONE',  ( -13.82310862910000004, -74.00000000000000000, 36.20061004779999791 ) ) ;
#26612 = CARTESIAN_POINT ( 'NONE',  ( 9.264974235690001336, -69.68028691090000848, -25.63136490189999961 ) ) ;
#26613 = CARTESIAN_POINT ( 'NONE',  ( -16.69422297484464934, -98.32621669506406192, 9.018748007586593118 ) ) ;
#26614 = ORIENTED_EDGE ( 'NONE', *, *, #14651, .F. ) ;
#26615 = CARTESIAN_POINT ( 'NONE',  ( -41.00000000000000000, -74.50000000000000000, -10.20110288159999890 ) ) ;
#26616 = DIRECTION ( 'NONE',  ( 0.2414462220490750377, 0.000000000000000000, -0.9704142011833034598 ) ) ;
#26617 = CARTESIAN_POINT ( 'NONE',  ( -16.78865735879999832, -72.00000000000000000, 25.46808810279999946 ) ) ;
#26618 = EDGE_CURVE ( 'NONE', #18811, #2130, #7347, .T. ) ;
#26619 = CARTESIAN_POINT ( 'NONE',  ( 15.63748056140000209, -111.0000000000000000, 3.386620984279999913 ) ) ;
#26620 = CARTESIAN_POINT ( 'NONE',  ( 22.78912717118120668, -61.50656701021978279, -7.252352442454050419 ) ) ;
#26621 = ORIENTED_EDGE ( 'NONE', *, *, #12006, .T. ) ;
#26622 = AXIS2_PLACEMENT_3D ( 'NONE', #14072, #16099, #9248 ) ;
#26623 = CARTESIAN_POINT ( 'NONE',  ( -32.39999999999999858, -89.50000000000000000, 0.000000000000000000 ) ) ;
#26624 = CARTESIAN_POINT ( 'NONE',  ( -32.32698596700000593, -74.07302383969998516, -21.86563713199999981 ) ) ;
#26625 = ORIENTED_EDGE ( 'NONE', *, *, #19347, .F. ) ;
#26626 = AXIS2_PLACEMENT_3D ( 'NONE', #22370, #24847, #11562 ) ;
#26627 = DIRECTION ( 'NONE',  ( 0.000000000000000000, -1.000000000000000000, 0.000000000000000000 ) ) ;
#26628 = CARTESIAN_POINT ( 'NONE',  ( 0.000000000000000000, -90.50000000000000000, 10.00000000000000000 ) ) ;
#26629 = CARTESIAN_POINT ( 'NONE',  ( -0.5578430832430000263, -60.34941021230000047, -23.62008496760000043 ) ) ;
#26630 = EDGE_LOOP ( 'NONE', ( #26026, #24163, #19336, #23679 ) ) ;
#26631 = DIRECTION ( 'NONE',  ( 0.4794255386042041156, 0.000000000000000000, 0.8775825618903719816 ) ) ;
#26632 = ORIENTED_EDGE ( 'NONE', *, *, #12267, .F. ) ;
#26633 = CARTESIAN_POINT ( 'NONE',  ( -36.79999999999999716, -64.11445222650000630, -0.1732050807570000017 ) ) ;
#26634 = DIRECTION ( 'NONE',  ( 0.9723926833689966465, 0.000000000000000000, -0.2333505288839995140 ) ) ;
#26635 = VERTEX_POINT ( 'NONE', #13891 ) ;
#26636 = FACE_OUTER_BOUND ( 'NONE', #24053, .T. ) ;
#26637 = CARTESIAN_POINT ( 'NONE',  ( 21.63571023749972255, -57.45864773928945368, 10.20337500119981300 ) ) ;
#26638 = ORIENTED_EDGE ( 'NONE', *, *, #27912, .T. ) ;
#26639 = CARTESIAN_POINT ( 'NONE',  ( 12.07601763839999975, -101.1284992150000051, -9.565697433850001374 ) ) ;
#26640 = EDGE_CURVE ( 'NONE', #7572, #27321, #27056, .T. ) ;
#26641 = CARTESIAN_POINT ( 'NONE',  ( -16.36797140879999901, -92.98481302150000261, -21.06274368449999912 ) ) ;
#26642 = AXIS2_PLACEMENT_3D ( 'NONE', #11419, #11112, #20321 ) ;
#26643 = DIRECTION ( 'NONE',  ( 0.000000000000000000, -1.000000000000000000, 0.000000000000000000 ) ) ;
#26644 = ORIENTED_EDGE ( 'NONE', *, *, #15583, .T. ) ;
#26645 = ADVANCED_FACE ( 'NONE', ( #5304 ), #18688, .F. ) ;
#26646 = CARTESIAN_POINT ( 'NONE',  ( -5.873418876839999747, -101.3150700380000018, 15.15334698740000086 ) ) ;
#26647 = DIRECTION ( 'NONE',  ( 0.000000000000000000, 1.000000000000000000, 0.000000000000000000 ) ) ;
#26648 = CARTESIAN_POINT ( 'NONE',  ( -21.94076895599999943, -74.04938808419998963, -32.26063837559999570 ) ) ;
#26649 = CARTESIAN_POINT ( 'NONE',  ( -2.488381629190000055, -57.43018266639999325, -24.62423963640000224 ) ) ;
#26650 = DIRECTION ( 'NONE',  ( 1.000000000000000000, 0.000000000000000000, 0.000000000000000000 ) ) ;
#26651 = EDGE_CURVE ( 'NONE', #14266, #20079, #19323, .T. ) ;
#26652 = CARTESIAN_POINT ( 'NONE',  ( 11.38886874731390542, -72.26599441443077865, -27.01882936454276063 ) ) ;
#26653 = CARTESIAN_POINT ( 'NONE',  ( 7.561767224756156480, -74.02518375726356226, -38.96762186395582006 ) ) ;
#26654 = ORIENTED_EDGE ( 'NONE', *, *, #3347, .F. ) ;
#26655 = EDGE_CURVE ( 'NONE', #21714, #300, #1925, .T. ) ;
#26656 = DIRECTION ( 'NONE',  ( 0.000000000000000000, 1.000000000000000000, 0.000000000000000000 ) ) ;
#26657 = CIRCLE ( 'NONE', #10815, 0.5000000000000027756 ) ;
#26658 = DIRECTION ( 'NONE',  ( 0.000000000000000000, 1.000000000000000000, 0.000000000000000000 ) ) ;
#26659 = CARTESIAN_POINT ( 'NONE',  ( 8.472249407519999664, -94.22763312370000222, -22.74885336210000020 ) ) ;
#26660 = FACE_OUTER_BOUND ( 'NONE', #15130, .T. ) ;
#26661 = CARTESIAN_POINT ( 'NONE',  ( -38.85038231309999901, -65.31510159580000163, 2.684458023169999930 ) ) ;
#26662 = CARTESIAN_POINT ( 'NONE',  ( -14.79537251110000007, -100.9197086940000077, 5.022279785309999411 ) ) ;
#26663 = APPLICATION_PROTOCOL_DEFINITION ( 'draft international standard', 'automotive_design', 1998, #11440 ) ;
#26664 = AXIS2_PLACEMENT_3D ( 'NONE', #2464, #12909, #10719 ) ;
#26665 = DIRECTION ( 'NONE',  ( 1.000000000000000000, 0.000000000000000000, 0.000000000000000000 ) ) ;
#26666 = CARTESIAN_POINT ( 'NONE',  ( -7.325370793560000315, -18.50000000000000000, -24.94672208400000102 ) ) ;
#26667 = ORIENTED_EDGE ( 'NONE', *, *, #11763, .F. ) ;
#26668 = DIRECTION ( 'NONE',  ( 1.000000000000000000, 0.000000000000000000, 0.000000000000000000 ) ) ;
#26669 = CARTESIAN_POINT ( 'NONE',  ( 23.42164076090000080, -94.71481430550001335, -6.692246347430000242 ) ) ;
#26670 = EDGE_LOOP ( 'NONE', ( #16137, #20200, #19789, #24353 ) ) ;
#26671 = CARTESIAN_POINT ( 'NONE',  ( -40.00000000000000000, -63.50000000000000000, 0.000000000000000000 ) ) ;
#26672 = DIRECTION ( 'NONE',  ( 0.3928703629870108349, 0.000000000000000000, -0.9195938657290262386 ) ) ;
#26673 = VERTEX_POINT ( 'NONE', #25124 ) ;
#26674 = DIRECTION ( 'NONE',  ( 0.000000000000000000, 1.000000000000000000, 0.000000000000000000 ) ) ;
#26675 = VERTEX_POINT ( 'NONE', #2984 ) ;
#26676 = CARTESIAN_POINT ( 'NONE',  ( -3.067686975420000017, -99.66156977119999283, -17.02465262619999820 ) ) ;
#26677 = AXIS2_PLACEMENT_3D ( 'NONE', #14768, #16683, #14364 ) ;
#26678 = CARTESIAN_POINT ( 'NONE',  ( 6.462050373635647382, -93.55106866495810891, -26.37547718614715109 ) ) ;
#26679 = ADVANCED_FACE ( 'NONE', ( #815 ), #11039, .F. ) ;
#26680 = DIRECTION ( 'NONE',  ( 1.000000000000000000, 0.000000000000000000, 0.000000000000000000 ) ) ;
#26681 = CARTESIAN_POINT ( 'NONE',  ( 26.74759209541820226, -72.18155182615700483, -9.512885920061126654 ) ) ;
#26682 = CARTESIAN_POINT ( 'NONE',  ( -10.20538995839999785, -18.50000000000000000, -19.00160311810000024 ) ) ;
#26683 = CARTESIAN_POINT ( 'NONE',  ( 47.19235072946354137, -79.33463070164246744, -1.154528427232027310 ) ) ;
#26684 = ORIENTED_EDGE ( 'NONE', *, *, #12967, .F. ) ;
#26685 = EDGE_CURVE ( 'NONE', #16440, #2786, #5174, .T. ) ;
#26686 = CARTESIAN_POINT ( 'NONE',  ( 10.12141009259999969, -93.14733690340000294, -25.45251484410000131 ) ) ;
#26687 = CARTESIAN_POINT ( 'NONE',  ( 23.35215130579999965, -19.42972408449999833, 1.425453684350000083 ) ) ;
#26688 = CARTESIAN_POINT ( 'NONE',  ( -14.93114631064312547, -79.63213912887773915, 36.29908221780583943 ) ) ;
#26689 = CARTESIAN_POINT ( 'NONE',  ( -13.06507290026208956, -92.68577957609070950, 27.56005317477162109 ) ) ;
#26690 = ORIENTED_EDGE ( 'NONE', *, *, #3244, .T. ) ;
#26691 = AXIS2_PLACEMENT_3D ( 'NONE', #27413, #25235, #3230 ) ;
#26692 = FACE_OUTER_BOUND ( 'NONE', #16176, .T. ) ;
#26693 = CARTESIAN_POINT ( 'NONE',  ( -15.68860394770000077, -92.62749637799998936, 23.81420858470000113 ) ) ;
#26694 = CYLINDRICAL_SURFACE ( 'NONE', #21942, 20.64285714289998808 ) ;
#26695 = VERTEX_POINT ( 'NONE', #8182 ) ;
#26696 = EDGE_CURVE ( 'NONE', #28503, #20661, #10070, .T. ) ;
#26697 = CARTESIAN_POINT ( 'NONE',  ( 26.84355716949999859, -67.87585789450000107, 1.442240390609999867 ) ) ;
#26698 = CARTESIAN_POINT ( 'NONE',  ( 0.4519837481779999666, -101.1191090859999946, -16.29812186430000054 ) ) ;
#26699 = CARTESIAN_POINT ( 'NONE',  ( 20.36016146999999776, -74.00000000000000000, -32.97008227039999895 ) ) ;
#26700 = CARTESIAN_POINT ( 'NONE',  ( -41.91080735079999897, -65.74290444429999525, -1.043878813350000101 ) ) ;
#26701 = CARTESIAN_POINT ( 'NONE',  ( -10.97403643530000039, -42.22519323619999909, -21.72972191419999888 ) ) ;
#26702 = AXIS2_PLACEMENT_3D ( 'NONE', #23890, #26656, #21843 ) ;
#26703 = DIRECTION ( 'NONE',  ( 0.000000000000000000, 1.000000000000000000, 0.000000000000000000 ) ) ;
#26704 = CARTESIAN_POINT ( 'NONE',  ( -11.74919335509972207, -57.47571039348258637, 20.26880008289946034 ) ) ;
#26705 = CIRCLE ( 'NONE', #20663, 9.500000000000001776 ) ;
#26706 = ORIENTED_EDGE ( 'NONE', *, *, #25325, .T. ) ;
#26707 = CARTESIAN_POINT ( 'NONE',  ( 28.44011693845432376, -92.82044061124386758, 11.01861317931760453 ) ) ;
#26708 = CARTESIAN_POINT ( 'NONE',  ( 22.58609710640000046, -18.50000000000000000, 2.144703970959999761 ) ) ;
#26709 = CARTESIAN_POINT ( 'NONE',  ( -5.525815865670000271, -96.93384555590000673, 20.55834025889999950 ) ) ;
#26710 = ORIENTED_EDGE ( 'NONE', *, *, #18579, .T. ) ;
#26711 = AXIS2_PLACEMENT_3D ( 'NONE', #9147, #17914, #6839 ) ;
#26712 = FACE_OUTER_BOUND ( 'NONE', #6769, .T. ) ;
#26713 = FACE_OUTER_BOUND ( 'NONE', #18218, .T. ) ;
#26714 = CARTESIAN_POINT ( 'NONE',  ( 19.04514928800000106, -22.53353387550000164, -9.014749987960000155 ) ) ;
#26715 = CARTESIAN_POINT ( 'NONE',  ( 22.03186001407977201, -19.46468284061640475, -0.3186543872829983859 ) ) ;
#26716 = CARTESIAN_POINT ( 'NONE',  ( -7.476488366829999954, -100.9137139110000021, 13.72916197330000010 ) ) ;
#26717 = ORIENTED_EDGE ( 'NONE', *, *, #862, .T. ) ;
#26718 = DIRECTION ( 'NONE',  ( 1.000000000000000000, 0.000000000000000000, 0.000000000000000000 ) ) ;
#26719 = CARTESIAN_POINT ( 'NONE',  ( -12.56815284899212770, -100.9609609850154754, -10.74558065766072268 ) ) ;
#26720 = ORIENTED_EDGE ( 'NONE', *, *, #19109, .F. ) ;
#26721 = CARTESIAN_POINT ( 'NONE',  ( 9.122466984649999944, -36.00948308300000633, -20.42228432030000107 ) ) ;
#26722 = CARTESIAN_POINT ( 'NONE',  ( 8.458704334359074650, -19.47547933409599352, -20.16190868471589326 ) ) ;
#26723 = ADVANCED_FACE ( 'NONE', ( #14326 ), #21178, .F. ) ;
#26724 = EDGE_CURVE ( 'NONE', #26341, #1349, #8400, .T. ) ;
#26725 = CARTESIAN_POINT ( 'NONE',  ( 8.485272409089999357, -99.18305472260000499, 16.24294048750000030 ) ) ;
#26726 = AXIS2_PLACEMENT_3D ( 'NONE', #10671, #19584, #6029 ) ;
#26727 = DIRECTION ( 'NONE',  ( 0.000000000000000000, 1.000000000000000000, 0.000000000000000000 ) ) ;
#26728 = CARTESIAN_POINT ( 'NONE',  ( -0.7106571652759999802, -98.65110728940000229, -18.63800496320000022 ) ) ;
#26729 = AXIS2_PLACEMENT_3D ( 'NONE', #6322, #26736, #13453 ) ;
#26730 = CARTESIAN_POINT ( 'NONE',  ( -20.39705533554743866, -92.66777315149587935, -22.67620303909143686 ) ) ;
#26731 = VERTEX_POINT ( 'NONE', #11984 ) ;
#26732 = CARTESIAN_POINT ( 'NONE',  ( 11.89800671740000126, -101.6095085860000040, -10.74240160559999957 ) ) ;
#26733 = CARTESIAN_POINT ( 'NONE',  ( -13.43613129169999887, -18.86819671679999999, 19.94230158159999888 ) ) ;
#26734 = CARTESIAN_POINT ( 'NONE',  ( 14.55779679992241071, -95.49497466763517650, 17.32786613936890419 ) ) ;
#26735 = EDGE_CURVE ( 'NONE', #77, #28180, #21308, .T. ) ;
#26736 = DIRECTION ( 'NONE',  ( -0.09756097560976716154, 0.000000000000000000, 0.9952295494196655712 ) ) ;
#26737 = DIRECTION ( 'NONE',  ( 0.000000000000000000, 1.000000000000000000, 0.000000000000000000 ) ) ;
#26738 = DIRECTION ( 'NONE',  ( 0.000000000000000000, 1.000000000000000000, 0.000000000000000000 ) ) ;
#26739 = CARTESIAN_POINT ( 'NONE',  ( -38.45241897108094520, -65.10974319588028436, -2.885177897951406223 ) ) ;
#26740 = CIRCLE ( 'NONE', #21611, 3.000000000000002665 ) ;
#26741 = CARTESIAN_POINT ( 'NONE',  ( 24.72994412613420678, -93.38817447845305253, -12.39839833700887972 ) ) ;
#26742 = CARTESIAN_POINT ( 'NONE',  ( 27.40661084094997690, -93.08996811606418476, 9.672291729878732980 ) ) ;
#26743 = ORIENTED_EDGE ( 'NONE', *, *, #13024, .T. ) ;
#26744 = CARTESIAN_POINT ( 'NONE',  ( 36.49273837329999992, -74.69502841160000628, -14.74290838079999943 ) ) ;
#26745 = AXIS2_PLACEMENT_3D ( 'NONE', #25981, #10230, #1388 ) ;
#26746 = CARTESIAN_POINT ( 'NONE',  ( 8.097647218569999694, -101.1461874760000086, 13.98396581760000146 ) ) ;
#26747 = ORIENTED_EDGE ( 'NONE', *, *, #21387, .T. ) ;
#26748 = ADVANCED_FACE ( 'NONE', ( #27865 ), #1506, .F. ) ;
#26749 = CARTESIAN_POINT ( 'NONE',  ( -11.75563520630000092, -62.12690044249999488, 20.90240914950000217 ) ) ;
#26750 = CARTESIAN_POINT ( 'NONE',  ( 7.241427273140969234, -74.22736093651798228, 40.35276762256386718 ) ) ;
#26751 = CIRCLE ( 'NONE', #6738, 2.999999999999998224 ) ;
#26752 = CARTESIAN_POINT ( 'NONE',  ( -24.67188499770000121, -93.87552273910000622, -2.728012672819999818 ) ) ;
#26753 = CARTESIAN_POINT ( 'NONE',  ( -41.75000000000000000, -63.30468293320000583, -1.587713240270000048 ) ) ;
#26754 = B_SPLINE_CURVE_WITH_KNOTS ( 'NONE', 3,
 ( #3167, #25316, #20651, #18752, #9846, #20938, #5618, #850, #14234, #16555, #18460, #25452, #27344, #5198, #22981, #13736, #61, #22335, #27298, #8908, #6751, #24961, #16059, #11238, #355, #13582, #20593, #7334, #2381, #13431, #17819, #17964, #13877 ),
 .UNSPECIFIED., .F., .F.,
 ( 4, 2, 1, 1, 2, 2, 1, 1, 1, 2, 2, 2, 1, 1, 2, 2, 1, 1, 2, 2, 4 ),
 ( 0.000000000000000000, 0.06250000000008817946, 0.09375000000014409307, 0.1093750000001827011, 0.1171875000001962736, 0.1250000000002098599, 0.1875000000002195744, 0.2187500000002333134, 0.2343750000002418343, 0.2421875000002425005, 0.2500000000002431388, 0.3750000000002057798, 0.4375000000001912359, 0.4687500000001821876, 0.4843750000001772471, 0.5000000000001723066, 0.6250000000001494360, 0.6875000000001377787, 0.7187500000001278977, 0.7500000000001180167, 1.000000000000000000 ),
 .UNSPECIFIED. ) ;
#26755 = CARTESIAN_POINT ( 'NONE',  ( -11.22183587504343016, -57.45864774162057387, -21.12541641655958813 ) ) ;
#26756 = VERTEX_POINT ( 'NONE', #28011 ) ;
#26757 = CARTESIAN_POINT ( 'NONE',  ( 12.02192718879999944, -92.50000321470000131, 27.08489650960000006 ) ) ;
#26758 = CARTESIAN_POINT ( 'NONE',  ( 29.27175831897154978, -74.33129955521587817, -26.10413971565343516 ) ) ;
#26759 = CARTESIAN_POINT ( 'NONE',  ( 7.472969336320000266, -74.00000023179998720, -38.65569830309999588 ) ) ;
#26760 = ORIENTED_EDGE ( 'NONE', *, *, #7325, .F. ) ;
#26761 = DIRECTION ( 'NONE',  ( 0.000000000000000000, -1.000000000000000000, 0.000000000000000000 ) ) ;
#26762 = EDGE_CURVE ( 'NONE', #18376, #842, #5643, .T. ) ;
#26763 = ADVANCED_FACE ( 'NONE', ( #16939 ), #4573, .T. ) ;
#26764 = DIRECTION ( 'NONE',  ( 0.4794255386042036715, 0.000000000000000000, 0.8775825618903724257 ) ) ;
#26765 = DIRECTION ( 'NONE',  ( 0.4794255386042041156, 0.000000000000000000, 0.8775825618903722036 ) ) ;
#26766 = CIRCLE ( 'NONE', #1639, 39.25000000000000000 ) ;
#26767 = CARTESIAN_POINT ( 'NONE',  ( 20.05203108810000145, -19.46163090469999801, 9.717827753279999925 ) ) ;
#26768 = CARTESIAN_POINT ( 'NONE',  ( 29.41275679339999982, -25.00000000000000000, 53.83969017199999740 ) ) ;
#26769 = CARTESIAN_POINT ( 'NONE',  ( 24.75930092260000137, -93.04780269100000112, -15.39069302210000068 ) ) ;
#26770 = DIRECTION ( 'NONE',  ( 1.000000000000000000, 0.000000000000000000, 0.000000000000000000 ) ) ;
#26771 = CARTESIAN_POINT ( 'NONE',  ( 9.136684621949999752, -66.46876714790001017, -24.36621523620000218 ) ) ;
#26772 = CARTESIAN_POINT ( 'NONE',  ( -17.26556418046517294, -97.08920889912290875, 11.18720961792155499 ) ) ;
#26773 = ORIENTED_EDGE ( 'NONE', *, *, #23398, .F. ) ;
#26774 = CIRCLE ( 'NONE', #25833, 18.64285714289999873 ) ;
#26775 = CARTESIAN_POINT ( 'NONE',  ( -15.42363691649999957, -67.46051717960000360, 22.84488648889999851 ) ) ;
#26776 = DIRECTION ( 'NONE',  ( 1.000000000000000000, 0.000000000000000000, 0.000000000000000000 ) ) ;
#26777 = CARTESIAN_POINT ( 'NONE',  ( -12.42802429090000160, -100.1785804069999983, -11.07820824309999885 ) ) ;
#26778 = CARTESIAN_POINT ( 'NONE',  ( 20.73262506157600882, -19.47322495657922303, 9.499032454948467930 ) ) ;
#26779 = CARTESIAN_POINT ( 'NONE',  ( 23.53321159739309820, -64.04625792510528015, -7.550089874302127413 ) ) ;
#26780 = ORIENTED_EDGE ( 'NONE', *, *, #14756, .T. ) ;
#26781 = CARTESIAN_POINT ( 'NONE',  ( 26.98910893724515958, -92.53708507728568122, -14.20702159799850861 ) ) ;
#26782 = ORIENTED_EDGE ( 'NONE', *, *, #28067, .F. ) ;
#26783 = ADVANCED_FACE ( 'NONE', ( #26253 ), #1926, .F. ) ;
#26784 = CIRCLE ( 'NONE', #3526, 57.75000000000000000 ) ;
#26785 = CARTESIAN_POINT ( 'NONE',  ( -10.72105426646302817, -19.49371706970953610, -21.56716125212794566 ) ) ;
#26786 = CARTESIAN_POINT ( 'NONE',  ( 25.32712259480000228, -57.40875702469999453, 1.379782074460000230 ) ) ;
#26787 = CARTESIAN_POINT ( 'NONE',  ( -17.74112986619786625, -94.52292883268154355, 16.06143330243891043 ) ) ;
#26788 = ORIENTED_EDGE ( 'NONE', *, *, #27600, .T. ) ;
#26789 = VERTEX_POINT ( 'NONE', #24350 ) ;
#26790 = CARTESIAN_POINT ( 'NONE',  ( -22.48840494017567693, -69.02525063278224593, 14.85218333891801734 ) ) ;
#26791 = CARTESIAN_POINT ( 'NONE',  ( 19.60651196810000130, -94.52293239719999463, 13.72231888900000030 ) ) ;
#26792 = CARTESIAN_POINT ( 'NONE',  ( -15.48259164459999937, -101.2306293330000102, 4.813005033020000489 ) ) ;
#26793 = EDGE_CURVE ( 'NONE', #27440, #14137, #7525, .T. ) ;
#26794 = VERTEX_POINT ( 'NONE', #19677 ) ;
#26795 = LINE ( 'NONE', #22262, #20128 ) ;
#26796 = CARTESIAN_POINT ( 'NONE',  ( -23.48465370626706772, -94.36683344921115690, -7.277453751676699056 ) ) ;
#26797 = CARTESIAN_POINT ( 'NONE',  ( 11.77298154309999845, -101.2530993010000060, -9.604785791470000333 ) ) ;
#26798 = DIRECTION ( 'NONE',  ( 0.000000000000000000, 1.000000000000000000, 0.000000000000000000 ) ) ;
#26799 = DIRECTION ( 'NONE',  ( 0.000000000000000000, 1.000000000000000000, 0.000000000000000000 ) ) ;
#26800 = ORIENTED_EDGE ( 'NONE', *, *, #10822, .T. ) ;
#26801 = CARTESIAN_POINT ( 'NONE',  ( 0.000000000000000000, -91.50000000000000000, 0.000000000000000000 ) ) ;
#26802 = CARTESIAN_POINT ( 'NONE',  ( 13.96793549529999900, -99.58396362730000817, -10.31305845590000025 ) ) ;
#26803 = CARTESIAN_POINT ( 'NONE',  ( 7.105427357599999217E-15, -74.50000000000000000, 3.552713678799999608E-15 ) ) ;
#26804 = CARTESIAN_POINT ( 'NONE',  ( -21.90514033510000047, -74.14434415679998835, -32.45847700809999736 ) ) ;
#26805 = CARTESIAN_POINT ( 'NONE',  ( -4.781896297090870718, -98.79895878316551716, -18.93514192741941571 ) ) ;
#26806 = DIRECTION ( 'NONE',  ( 0.000000000000000000, 1.000000000000000000, 0.000000000000000000 ) ) ;
#26807 = DIRECTION ( 'NONE',  ( 0.000000000000000000, 1.000000000000000000, 0.000000000000000000 ) ) ;
#26808 = CARTESIAN_POINT ( 'NONE',  ( -18.74560011510000024, -18.62107711730000048, 14.23481631049999940 ) ) ;
#26809 = VERTEX_POINT ( 'NONE', #28695 ) ;
#26810 = CARTESIAN_POINT ( 'NONE',  ( -7.325370793560000315, -18.50000000000000000, -24.94672208400000102 ) ) ;
#26811 = CARTESIAN_POINT ( 'NONE',  ( 9.393614001710000494, -38.00000000000000000, -22.97877290430000130 ) ) ;
#26812 = CARTESIAN_POINT ( 'NONE',  ( -23.81103214300399173, -92.84927079008255646, -19.06003205102011222 ) ) ;
#26813 = CARTESIAN_POINT ( 'NONE',  ( -7.325370793560000315, -45.73899999920000425, -24.94672208400000102 ) ) ;
#26814 = CARTESIAN_POINT ( 'NONE',  ( 18.39062685420683252, -98.53908159012071621, 3.638000403930131021 ) ) ;
#26815 = AXIS2_PLACEMENT_3D ( 'NONE', #9632, #7761, #14304 ) ;
#26816 = CARTESIAN_POINT ( 'NONE',  ( 0.000000000000000000, 0.000000000000000000, 0.000000000000000000 ) ) ;
#26817 = DIRECTION ( 'NONE',  ( 1.000000000000000000, 0.000000000000000000, 0.000000000000000000 ) ) ;
#26818 = CARTESIAN_POINT ( 'NONE',  ( -11.49099193059999813, -57.47122622279999860, -20.56185111770000162 ) ) ;
#26819 = EDGE_CURVE ( 'NONE', #23453, #15463, #1636, .T. ) ;
#26820 = EDGE_LOOP ( 'NONE', ( #16721, #19613, #15995 ) ) ;
#26821 = CARTESIAN_POINT ( 'NONE',  ( 26.69293917519999937, -15.49689110870000164, 48.86109741659999628 ) ) ;
#26822 = CARTESIAN_POINT ( 'NONE',  ( 24.58030493329999899, -18.50000000000000000, 2.442848308399999890 ) ) ;
#26823 = ORIENTED_EDGE ( 'NONE', *, *, #24213, .T. ) ;
#26824 = CARTESIAN_POINT ( 'NONE',  ( 22.70347112454390626, -37.13515264715037034, 10.14607557079202138 ) ) ;
#26825 = CARTESIAN_POINT ( 'NONE',  ( -36.92846103339999786, -69.00000000000000000, 1.677989385109999843 ) ) ;
#26826 = EDGE_CURVE ( 'NONE', #4674, #22328, #20545, .T. ) ;
#26827 = ORIENTED_EDGE ( 'NONE', *, *, #27466, .T. ) ;
#26828 = CARTESIAN_POINT ( 'NONE',  ( -26.60903970598167589, -33.79999999999999716, -48.70752046822583736 ) ) ;
#26829 = EDGE_CURVE ( 'NONE', #3916, #9687, #13057, .T. ) ;
#26830 = CARTESIAN_POINT ( 'NONE',  ( 5.873227382016245279, -93.41743724444744146, -26.93228196801963392 ) ) ;
#26831 = B_SPLINE_CURVE_WITH_KNOTS ( 'NONE', 3,
 ( #28382, #8412, #21829, #28110, #28527, #17033, #16901, #8147, #25791, #17319, #26213, #14701, #6239, #23593, #24016, #19779, #8692 ),
 .UNSPECIFIED., .F., .F.,
 ( 4, 2, 2, 1, 1, 1, 1, 1, 2, 2, 4 ),
 ( 0.000000000000000000, 0.2500000000002183254, 0.3750000000003250733, 0.4375000000003810285, 0.4687500000004065637, 0.4843750000004191092, 0.4921875000004253820, 0.4960937500004258260, 0.4980468750004235501, 0.5000000000004213296, 1.000000000000000000 ),
 .UNSPECIFIED. ) ;
#26832 = CARTESIAN_POINT ( 'NONE',  ( 0.000000000000000000, -18.50000000000000000, 0.000000000000000000 ) ) ;
#26833 = CARTESIAN_POINT ( 'NONE',  ( -40.00000000000000000, -63.00000000000000000, 0.000000000000000000 ) ) ;
#26834 = CARTESIAN_POINT ( 'NONE',  ( -10.34918404329999930, -18.86473257140000115, -21.20072926229999766 ) ) ;
#26835 = CARTESIAN_POINT ( 'NONE',  ( 10.38935269913133830, -95.90275867109022556, -20.92386860843906504 ) ) ;
#26836 = ORIENTED_EDGE ( 'NONE', *, *, #2528, .F. ) ;
#26837 = CARTESIAN_POINT ( 'NONE',  ( 0.000000000000000000, -39.50000000000000000, 0.000000000000000000 ) ) ;
#26838 = DIRECTION ( 'NONE',  ( 0.4999999999997570277, 0.000000000000000000, 0.8660254037845789288 ) ) ;
#26839 = CARTESIAN_POINT ( 'NONE',  ( -12.46836486461607940, -92.52640451556476364, 27.83505318500035841 ) ) ;
#26840 = ORIENTED_EDGE ( 'NONE', *, *, #10555, .T. ) ;
#26841 = DIRECTION ( 'NONE',  ( 0.000000000000000000, -1.000000000000000000, 0.000000000000000000 ) ) ;
#26842 = CARTESIAN_POINT ( 'NONE',  ( -17.04762123990000333, -93.16621335700000373, 21.75328878690000423 ) ) ;
#26843 = LINE ( 'NONE', #22619, #14516 ) ;
#26844 = VERTEX_POINT ( 'NONE', #18084 ) ;
#26845 = CARTESIAN_POINT ( 'NONE',  ( -15.96476880600000037, -99.60585778459999062, 6.856918404960000046 ) ) ;
#26846 = CARTESIAN_POINT ( 'NONE',  ( 0.5238881141819999865, -100.0994409990000094, -17.21532606639999941 ) ) ;
#26847 = FACE_OUTER_BOUND ( 'NONE', #16902, .T. ) ;
#26848 = CARTESIAN_POINT ( 'NONE',  ( -19.63525383122224710, -57.47122601392510433, 13.01113855736701197 ) ) ;
#26849 = CARTESIAN_POINT ( 'NONE',  ( -11.46712328369999945, -34.67035637050000219, -19.43657039250000196 ) ) ;
#26850 = CARTESIAN_POINT ( 'NONE',  ( -26.69328098980000163, -77.00000000000000000, -35.88566914520000495 ) ) ;
#26851 = EDGE_CURVE ( 'NONE', #10652, #19426, #64, .T. ) ;
#26852 = EDGE_LOOP ( 'NONE', ( #7910, #22882, #19081, #5495, #21539 ) ) ;
#26853 = CARTESIAN_POINT ( 'NONE',  ( 28.41344044897496701, -92.80045754835145999, 11.08727913710079527 ) ) ;
#26854 = DIRECTION ( 'NONE',  ( 0.000000000000000000, 1.000000000000000000, 0.000000000000000000 ) ) ;
#26855 = VERTEX_POINT ( 'NONE', #16178 ) ;
#26856 = CARTESIAN_POINT ( 'NONE',  ( 7.318372426699999878, -73.93831497249999529, 38.68350751799999898 ) ) ;
#26857 = CARTESIAN_POINT ( 'NONE',  ( 0.000000000000000000, -80.50000000000000000, 0.000000000000000000 ) ) ;
#26858 = EDGE_CURVE ( 'NONE', #15395, #13005, #24647, .T. ) ;
#26859 = B_SPLINE_SURFACE_WITH_KNOTS ( 'NONE', 5, 5, ( 
 ( #11951, #23054, #11654, #3236, #20863, #18677 ),
 ( #12093, #923, #27577, #2800, #9623, #2947 ),
 ( #3369, #16479, #25381, #12234, #7749, #1069 ),
 ( #16177, #9908, #16615, #25509, #25088, #14003 ),
 ( #5547, #23323, #21147, #22910, #10037, #18951 ),
 ( #22759, #11810, #20722, #781, #21834, #19090 ) ),
 .UNSPECIFIED., .F., .F., .F.,
 ( 6, 6 ),
 ( 6, 6 ),
 ( 2.659855565630000029, 4.432291325320000475 ),
 ( 0.000000000000000000, 0.5000000000000000000 ),
 .UNSPECIFIED. ) ;
#26860 = CARTESIAN_POINT ( 'NONE',  ( 22.12248824515891243, -19.46487770188272393, 0.1046948809405091052 ) ) ;
#26861 = CARTESIAN_POINT ( 'NONE',  ( -7.039259910420000210, -101.5964542560000012, 14.41325148729999839 ) ) ;
#26862 = EDGE_LOOP ( 'NONE', ( #10450, #20565, #23129, #28072 ) ) ;
#26863 = CARTESIAN_POINT ( 'NONE',  ( 26.97099430927276487, -72.31255207680982267, -11.30091564182526653 ) ) ;
#26864 = CARTESIAN_POINT ( 'NONE',  ( -21.14183719079999690, -62.95300605010000083, 15.28077941859999989 ) ) ;
#26865 = CARTESIAN_POINT ( 'NONE',  ( 8.245988246530000509, -37.92543680059999645, -21.67015450270000088 ) ) ;
#26866 = CARTESIAN_POINT ( 'NONE',  ( 8.492728600515889070, -19.47622732623166542, -20.12650533279332876 ) ) ;
#26867 = CARTESIAN_POINT ( 'NONE',  ( -9.506169627659998511, -74.00000000000000000, 42.57810630240000194 ) ) ;
#26868 = CARTESIAN_POINT ( 'NONE',  ( 23.53496214160000122, -18.86473257140000115, 1.637708341159999970 ) ) ;
#26869 = CARTESIAN_POINT ( 'NONE',  ( -5.417924262829999726, -95.55433883420000996, -21.95361216799999937 ) ) ;
#26870 = DIRECTION ( 'NONE',  ( -0.9639181000863472626, 0.000000000000000000, 0.2661989788220960884 ) ) ;
#26871 = ORIENTED_EDGE ( 'NONE', *, *, #26923, .T. ) ;
#26872 = DIRECTION ( 'NONE',  ( 0.000000000000000000, -1.000000000000000000, 0.000000000000000000 ) ) ;
#26873 = CARTESIAN_POINT ( 'NONE',  ( 28.00537423697155148, -69.05891618901559070, 2.237991812796679802 ) ) ;
#26874 = CARTESIAN_POINT ( 'NONE',  ( 15.48475574042589287, -95.04500097814597837, 17.29312253357641183 ) ) ;
#26875 = CARTESIAN_POINT ( 'NONE',  ( 7.181689689069999716, -111.0000000000000000, 15.80535034289999885 ) ) ;
#26876 = CIRCLE ( 'NONE', #18027, 18.14285714289999873 ) ;
#26877 = CARTESIAN_POINT ( 'NONE',  ( 21.89902306919999830, -37.95659433950000050, -8.637924301090000867 ) ) ;
#26878 = DIRECTION ( 'NONE',  ( -0.6983618402939030245, 0.000000000000000000, -0.7157448847329006547 ) ) ;
#26879 = CARTESIAN_POINT ( 'NONE',  ( -11.32307664120000013, -101.1889999979999999, 9.421136869679999748 ) ) ;
#26880 = LINE ( 'NONE', #8785, #1613 ) ;
#26881 = CARTESIAN_POINT ( 'NONE',  ( 22.02115912736433145, -94.16483583581477035, 13.38915878678963622 ) ) ;
#26882 = ORIENTED_EDGE ( 'NONE', *, *, #27087, .T. ) ;
#26883 = CARTESIAN_POINT ( 'NONE',  ( -29.76178938840000043, -93.00000000000000000, 6.669774538800000485 ) ) ;
#26884 = ADVANCED_FACE ( 'NONE', ( #27274 ), #11666, .F. ) ;
#26885 = CARTESIAN_POINT ( 'NONE',  ( -13.94341442410000020, -60.21477618889999661, 21.38633822419999930 ) ) ;
#26886 = EDGE_CURVE ( 'NONE', #1234, #1856, #15594, .T. ) ;
#26887 = CIRCLE ( 'NONE', #25018, 6.750000000000000000 ) ;
#26888 = EDGE_LOOP ( 'NONE', ( #22156, #21155, #23978, #27309 ) ) ;
#26889 = CARTESIAN_POINT ( 'NONE',  ( -12.45758713059999856, -65.72077506549999271, 22.18618133640000067 ) ) ;
#26890 = CARTESIAN_POINT ( 'NONE',  ( -11.74919631470000070, -57.47570992170000181, 20.26880469069999791 ) ) ;
#26891 = CARTESIAN_POINT ( 'NONE',  ( 0.000000000000000000, -2.000000000000000000, 0.000000000000000000 ) ) ;
#26892 = CARTESIAN_POINT ( 'NONE',  ( 27.16500929229999883, -92.56290635029999692, 9.195763470240001070 ) ) ;
#26893 = ADVANCED_FACE ( 'NONE', ( #4527 ), #22465, .T. ) ;
#26894 = CARTESIAN_POINT ( 'NONE',  ( 26.75649127029999619, -101.1889999979999999, -13.26822602009999841 ) ) ;
#26895 = EDGE_CURVE ( 'NONE', #19618, #17027, #9253, .T. ) ;
#26896 = DIRECTION ( 'NONE',  ( 0.000000000000000000, -1.000000000000000000, 0.000000000000000000 ) ) ;
#26897 = CARTESIAN_POINT ( 'NONE',  ( 16.54149060430000162, -99.85455315880000171, 4.477554858519999570 ) ) ;
#26898 = ORIENTED_EDGE ( 'NONE', *, *, #27903, .F. ) ;
#26899 = PLANE ( 'NONE',  #6035 ) ;
#26900 = CARTESIAN_POINT ( 'NONE',  ( 21.48302419030000010, -36.56890884650000118, -7.253824583220000122 ) ) ;
#26901 = CARTESIAN_POINT ( 'NONE',  ( -15.31628404939999832, -99.57131247680000286, -8.300247877169999455 ) ) ;
#26902 = ORIENTED_EDGE ( 'NONE', *, *, #11843, .T. ) ;
#26903 = CARTESIAN_POINT ( 'NONE',  ( 8.524613012669300716, -92.66455718075849290, 29.28448434949323342 ) ) ;
#26904 = EDGE_LOOP ( 'NONE', ( #12789, #13109, #8359, #19201 ) ) ;
#26905 = CARTESIAN_POINT ( 'NONE',  ( 20.69873715099999956, -52.63055504179948230, 10.61298605969999187 ) ) ;
#26906 = CARTESIAN_POINT ( 'NONE',  ( 15.53338745080000116, -83.75000000000000000, 28.43367500519999780 ) ) ;
#26907 = CARTESIAN_POINT ( 'NONE',  ( 21.54650012300000128, -26.06274386009999944, 9.572267663609999033 ) ) ;
#26908 = DIRECTION ( 'NONE',  ( 0.000000000000000000, 1.000000000000000000, 0.000000000000000000 ) ) ;
#26909 = DIRECTION ( 'NONE',  ( 0.000000000000000000, 1.000000000000000000, 0.000000000000000000 ) ) ;
#26910 = AXIS2_PLACEMENT_3D ( 'NONE', #21363, #19177, #14383 ) ;
#26911 = CARTESIAN_POINT ( 'NONE',  ( 19.22218838680000275, -18.50000000000000000, 9.014732214529999510 ) ) ;
#26912 = CARTESIAN_POINT ( 'NONE',  ( -32.72868145578198096, -79.93462708495536617, -22.47659135972876143 ) ) ;
#26913 = CARTESIAN_POINT ( 'NONE',  ( -16.98338203059941520, -97.76568412893885807, 9.980451257739110460 ) ) ;
#26914 = ORIENTED_EDGE ( 'NONE', *, *, #28760, .F. ) ;
#26915 = DIRECTION ( 'NONE',  ( 0.000000000000000000, 1.000000000000000000, 0.000000000000000000 ) ) ;
#26916 = CARTESIAN_POINT ( 'NONE',  ( -3.243952255836194176, -98.17436949751105146, 20.08298429705580901 ) ) ;
#26917 = CARTESIAN_POINT ( 'NONE',  ( -13.09874939020000006, -100.0482783049999966, -11.14007078999999933 ) ) ;
#26918 = CARTESIAN_POINT ( 'NONE',  ( 21.67805398002857586, -19.48685756505367905, 9.537775450224595275 ) ) ;
#26919 = CARTESIAN_POINT ( 'NONE',  ( -39.92825895920000079, -74.14144493790000467, -7.283540598980000169 ) ) ;
#26920 = ORIENTED_EDGE ( 'NONE', *, *, #28215, .T. ) ;
#26921 = CARTESIAN_POINT ( 'NONE',  ( 0.000000000000000000, -33.49689110869999809, 0.000000000000000000 ) ) ;
#26922 = ORIENTED_EDGE ( 'NONE', *, *, #18475, .F. ) ;
#26923 = EDGE_CURVE ( 'NONE', #6001, #13803, #21929, .T. ) ;
#26924 = EDGE_CURVE ( 'NONE', #10539, #24995, #27578, .T. ) ;
#26925 = FACE_OUTER_BOUND ( 'NONE', #15390, .T. ) ;
#26926 = DIRECTION ( 'NONE',  ( 0.000000000000000000, -1.000000000000000000, 0.000000000000000000 ) ) ;
#26927 = CARTESIAN_POINT ( 'NONE',  ( 10.52519477159999894, -92.53453854219999641, 27.02797911619999738 ) ) ;
#26928 = ORIENTED_EDGE ( 'NONE', *, *, #13993, .T. ) ;
#26929 = VECTOR ( 'NONE', #5380, 1000.000000000000000 ) ;
#26930 = AXIS2_PLACEMENT_3D ( 'NONE', #21661, #21376, #12609 ) ;
#26931 = EDGE_LOOP ( 'NONE', ( #15551, #19464, #5306, #13772 ) ) ;
#26932 = CARTESIAN_POINT ( 'NONE',  ( -27.56394947256076122, -93.41743724413561267, 0.2670232293074757957 ) ) ;
#26933 = CARTESIAN_POINT ( 'NONE',  ( 20.46603143229999944, -94.22485786839999378, 13.79395319179999824 ) ) ;
#26934 = CARTESIAN_POINT ( 'NONE',  ( 46.25000000000000000, -74.00000000000000000, -4.582575694960000057 ) ) ;
#26935 = ORIENTED_EDGE ( 'NONE', *, *, #10151, .F. ) ;
#26936 = CARTESIAN_POINT ( 'NONE',  ( -15.42268960139999834, -111.0000000000000000, 4.259183661149999800 ) ) ;
#26937 = CARTESIAN_POINT ( 'NONE',  ( -22.43272078519999724, -80.34292036729999609, -32.20769377289999369 ) ) ;
#26938 = CARTESIAN_POINT ( 'NONE',  ( 12.47108311319999885, -101.4121386959999995, -9.987215287249998852 ) ) ;
#26939 = CARTESIAN_POINT ( 'NONE',  ( -14.05781381009999897, -93.65023553250000532, -20.95136237079999830 ) ) ;
#26940 = CARTESIAN_POINT ( 'NONE',  ( -23.50862727400000196, -94.59276292389999696, -3.692480628369999796 ) ) ;
#26941 = ORIENTED_EDGE ( 'NONE', *, *, #6518, .F. ) ;
#26942 = CARTESIAN_POINT ( 'NONE',  ( -6.238095109968847751, -101.6484611540000031, 14.73393615897204079 ) ) ;
#26943 = B_SPLINE_CURVE_WITH_KNOTS ( 'NONE', 3,
 ( #8462, #17365, #28573, #8608, #26110, #15010, #21594, #1653, #10626, #24057, #3961, #4097, #22030, #23923, #21879, #10771, #25968, #2078 ),
 .UNSPECIFIED., .F., .F.,
 ( 4, 2, 2, 2, 1, 1, 1, 1, 2, 2, 4 ),
 ( 0.000000000000000000, 0.2499999999999300004, 0.3749999999998957501, 0.4374999999998792632, 0.4687499999998714362, 0.4843749999998674949, 0.4921874999998651634, 0.4960937499998637756, 0.4980468749998633871, 0.4999999999998629985, 1.000000000000000000 ),
 .UNSPECIFIED. ) ;
#26944 = CARTESIAN_POINT ( 'NONE',  ( -16.98520236649999759, -99.83167676440000093, 3.436659022809999797 ) ) ;
#26945 = DIRECTION ( 'NONE',  ( 1.000000000000000000, 0.000000000000000000, 0.000000000000000000 ) ) ;
#26946 = CARTESIAN_POINT ( 'NONE',  ( -21.71458329359999695, -74.50000000000000000, -32.69645379630000548 ) ) ;
#26947 = EDGE_CURVE ( 'NONE', #8106, #134, #6467, .T. ) ;
#26948 = CARTESIAN_POINT ( 'NONE',  ( 28.66244647610000129, -111.0000000000000000, 10.42660836539999991 ) ) ;
#26949 = CIRCLE ( 'NONE', #4129, 52.35000000000000142 ) ;
#26950 = DIRECTION ( 'NONE',  ( 1.000000000000000000, 0.000000000000000000, 0.000000000000000000 ) ) ;
#26951 = CARTESIAN_POINT ( 'NONE',  ( -16.14562817639999892, -101.1889999979999999, 4.458832895280000486 ) ) ;
#26952 = DIRECTION ( 'NONE',  ( 0.000000000000000000, 1.000000000000000000, 0.000000000000000000 ) ) ;
#26953 = ORIENTED_EDGE ( 'NONE', *, *, #18989, .T. ) ;
#26954 = CIRCLE ( 'NONE', #26479, 0.9999999999999980016 ) ;
#26955 = AXIS2_PLACEMENT_3D ( 'NONE', #27206, #11438, #27348 ) ;
#26956 = DIRECTION ( 'NONE',  ( 0.000000000000000000, -1.000000000000000000, 0.000000000000000000 ) ) ;
#26957 = VECTOR ( 'NONE', #28237, 1000.000000000000000 ) ;
#26958 = AXIS2_PLACEMENT_3D ( 'NONE', #10202, #25825, #10611 ) ;
#26959 = LINE ( 'NONE', #16151, #14465 ) ;
#26960 = CARTESIAN_POINT ( 'NONE',  ( 8.963945925320000896, -35.29521789780000063, -19.99082963590000261 ) ) ;
#26961 = CARTESIAN_POINT ( 'NONE',  ( -23.82156939022300435, -92.83160374580931773, -19.04685915412109409 ) ) ;
#26962 = CARTESIAN_POINT ( 'NONE',  ( 0.000000000000000000, -2.000000000000000000, 0.000000000000000000 ) ) ;
#26963 = CARTESIAN_POINT ( 'NONE',  ( 46.42255779199999921, -80.25272389239999882, -3.562991745209999728 ) ) ;
#26964 = DIRECTION ( 'NONE',  ( 1.000000000000000000, 0.000000000000000000, 0.000000000000000000 ) ) ;
#26965 = CONTEXT_DEPENDENT_SHAPE_REPRESENTATION ( #13310, #28509 ) ;
#26966 = CARTESIAN_POINT ( 'NONE',  ( -12.22420097160000019, -62.12717499380000419, -20.63207585329999816 ) ) ;
#26967 = CARTESIAN_POINT ( 'NONE',  ( 26.02259374959999860, -91.50000000000000000, -15.90831903569999994 ) ) ;
#26968 = ORIENTED_EDGE ( 'NONE', *, *, #10325, .T. ) ;
#26969 = CARTESIAN_POINT ( 'NONE',  ( -27.68147801010000109, -38.34400911419999858, -50.67060561630000137 ) ) ;
#26971 = VERTEX_POINT ( 'NONE', #19092 ) ;
#26970 = CONICAL_SURFACE ( 'NONE', #739, 55.67692378859999280, 1.047197551199999799 ) ;
#26972 = CARTESIAN_POINT ( 'NONE',  ( 0.000000000000000000, -13.50000000000000000, 0.000000000000000000 ) ) ;
#26973 = CARTESIAN_POINT ( 'NONE',  ( 0.000000000000000000, -16.00000000000000000, 0.000000000000000000 ) ) ;
#26974 = ORIENTED_EDGE ( 'NONE', *, *, #18810, .F. ) ;
#26975 = CARTESIAN_POINT ( 'NONE',  ( 50.00000000000000000, -11.00000000000000000, 4.500000000000000000 ) ) ;
#26976 = AXIS2_PLACEMENT_3D ( 'NONE', #6154, #12837, #21749 ) ;
#26977 = CARTESIAN_POINT ( 'NONE',  ( 1.678657213230000024E-14, -74.00000000000000000, 7.838174553849999450E-15 ) ) ;
#26978 = CARTESIAN_POINT ( 'NONE',  ( 1.436102896439999999, -94.52419709919999491, 23.97566704719999819 ) ) ;
#26979 = DIRECTION ( 'NONE',  ( 1.000000000000000000, 0.000000000000000000, 0.000000000000000000 ) ) ;
#26980 = CARTESIAN_POINT ( 'NONE',  ( 0.7331063123750001242, -99.53431386179998697, -17.39857302659999760 ) ) ;
#26981 = CARTESIAN_POINT ( 'NONE',  ( 11.59887401429227438, -98.07255008377731542, -16.87401357543511438 ) ) ;
#26982 = EDGE_LOOP ( 'NONE', ( #3388, #12221, #22790, #16238 ) ) ;
#26983 = CARTESIAN_POINT ( 'NONE',  ( -17.94180966909999597, -45.73899999920000425, 18.81731824139999887 ) ) ;
#26984 = CARTESIAN_POINT ( 'NONE',  ( -20.04435942636430923, -59.05300800389983351, 12.20496567544505062 ) ) ;
#26985 = CARTESIAN_POINT ( 'NONE',  ( -13.34153245340000105, -93.00000000000000000, 27.42724032409999779 ) ) ;
#26986 = ORIENTED_EDGE ( 'NONE', *, *, #17771, .F. ) ;
#26987 = CARTESIAN_POINT ( 'NONE',  ( -37.89761526037040795, -63.33348905331877177, -0.8208133671573618617 ) ) ;
#26988 = DIRECTION ( 'NONE',  ( 0.000000000000000000, 1.000000000000000000, 0.000000000000000000 ) ) ;
#26989 = CARTESIAN_POINT ( 'NONE',  ( -22.58183123469999742, -70.96441436690000160, 17.76382364619999876 ) ) ;
#26990 = VERTEX_POINT ( 'NONE', #25511 ) ;
#26991 = ADVANCED_FACE ( 'NONE', ( #8014 ), #23771, .F. ) ;
#26992 = CARTESIAN_POINT ( 'NONE',  ( -2.986711171310000079, -94.79581646409999962, 23.48470800579999818 ) ) ;
#26993 = CARTESIAN_POINT ( 'NONE',  ( 0.6035559297369998966, -99.61736775859999682, -17.33444585840000229 ) ) ;
#26994 = CARTESIAN_POINT ( 'NONE',  ( 26.07303258718441086, -74.32832717789354149, -29.29802673409578517 ) ) ;
#26995 = CARTESIAN_POINT ( 'NONE',  ( 20.56993010089999885, -36.00000000000000000, -10.19436680729999978 ) ) ;
#26996 = EDGE_CURVE ( 'NONE', #23820, #7778, #2384, .T. ) ;
#26997 = FACE_OUTER_BOUND ( 'NONE', #3321, .T. ) ;
#26998 = EDGE_CURVE ( 'NONE', #5288, #25651, #4723, .T. ) ;
#26999 = VECTOR ( 'NONE', #25531, 1000.000000000000000 ) ;
#27000 = AXIS2_PLACEMENT_3D ( 'NONE', #25548, #11988, #10213 ) ;
#27001 = CARTESIAN_POINT ( 'NONE',  ( 6.916458556970000338, -99.55609327400000552, 15.95096318659999746 ) ) ;
#27002 = VERTEX_POINT ( 'NONE', #5548 ) ;
#27003 = B_SPLINE_CURVE_WITH_KNOTS ( 'NONE', 5,
 ( #15181, #8640, #6173, #15048, #6025, #19579, #3855, #26436, #10813 ),
 .UNSPECIFIED., .F., .F.,
 ( 6, 3, 6 ),
 ( 0.000000000000000000, 1.377214429579999955, 2.292501860869999852 ),
 .UNSPECIFIED. ) ;
#27004 = CARTESIAN_POINT ( 'NONE',  ( -17.54428855099999751, -94.59276292389999696, 16.07755916609999858 ) ) ;
#27005 = CARTESIAN_POINT ( 'NONE',  ( 12.52242149219999945, -98.51737542899999767, 15.18253812500000066 ) ) ;
#27006 = CARTESIAN_POINT ( 'NONE',  ( 7.260248548399999891, -73.97917265380000629, 40.03821526680000176 ) ) ;
#27007 = CARTESIAN_POINT ( 'NONE',  ( 9.015412349990000962, -94.52293239719999463, -22.16843899350000058 ) ) ;
#27008 = CARTESIAN_POINT ( 'NONE',  ( 23.40535227632090098, -19.48298526462809122, 1.394588373438266693 ) ) ;
#27009 = CARTESIAN_POINT ( 'NONE',  ( 27.11562635247914699, -72.17813883581031575, -11.54692017584613772 ) ) ;
#27010 = CARTESIAN_POINT ( 'NONE',  ( -12.46823725472511590, -101.5409490181953487, -10.15889664027061734 ) ) ;
#27011 = CARTESIAN_POINT ( 'NONE',  ( 9.227003638719999401, -35.93081093159999995, -19.61343128729999918 ) ) ;
#27012 = TOROIDAL_SURFACE ( 'NONE', #8836, 19.50000000000000000, 7.000000000000000000 ) ;
#27013 = CARTESIAN_POINT ( 'NONE',  ( 8.617475452619551390, -19.47931211704219479, -19.97879563106347334 ) ) ;
#27014 = ORIENTED_EDGE ( 'NONE', *, *, #8897, .F. ) ;
#27015 = AXIS2_PLACEMENT_3D ( 'NONE', #16642, #11976, #25535 ) ;
#27016 = FACE_OUTER_BOUND ( 'NONE', #4903, .T. ) ;
#27017 = CARTESIAN_POINT ( 'NONE',  ( -36.71038433799841982, -63.05619511567397950, 0.07254510122748375478 ) ) ;
#27018 = CARTESIAN_POINT ( 'NONE',  ( 0.3872225632639999526, -99.92967428129999519, -17.35613189629999908 ) ) ;
#27019 = CARTESIAN_POINT ( 'NONE',  ( -2.150719047535482709, -19.47341637985288187, -22.71689757131826326 ) ) ;
#27020 = CARTESIAN_POINT ( 'NONE',  ( 0.000000000000000000, -2.000000000000000000, 0.000000000000000000 ) ) ;
#27021 = CARTESIAN_POINT ( 'NONE',  ( 28.23243646506086790, -69.78284652344737538, 2.418637941536898150 ) ) ;
#27022 = CARTESIAN_POINT ( 'NONE',  ( 15.62957910242984383, -94.97526614585484594, 17.28402939849175013 ) ) ;
#27023 = EDGE_CURVE ( 'NONE', #21528, #22228, #11992, .T. ) ;
#27024 = CARTESIAN_POINT ( 'NONE',  ( -38.04193375797715504, -65.73717265118393982, 0.9755880792773293786 ) ) ;
#27025 = CARTESIAN_POINT ( 'NONE',  ( -13.17062163620000170, -68.28989939179999169, -23.12788393509999807 ) ) ;
#27026 = CYLINDRICAL_SURFACE ( 'NONE', #10934, 20.64285714290000584 ) ;
#27027 = ADVANCED_FACE ( 'NONE', ( #12235 ), #10336, .T. ) ;
#27028 = CARTESIAN_POINT ( 'NONE',  ( 24.64042015088250182, -93.08494709825269808, -15.48202326831530407 ) ) ;
#27029 = CARTESIAN_POINT ( 'NONE',  ( -10.13149966729999818, -18.50000000000000000, 18.43352823549999897 ) ) ;
#27030 = ORIENTED_EDGE ( 'NONE', *, *, #6313, .T. ) ;
#27031 = EDGE_CURVE ( 'NONE', #4012, #2845, #3764, .T. ) ;
#27032 = CARTESIAN_POINT ( 'NONE',  ( 36.48289528369999601, -74.76922865969999066, -14.76362601449999801 ) ) ;
#27033 = AXIS2_PLACEMENT_3D ( 'NONE', #24972, #372, #4866 ) ;
#27034 = VECTOR ( 'NONE', #23340, 1000.000000000000000 ) ;
#27035 = AXIS2_PLACEMENT_3D ( 'NONE', #28087, #23445, #21388 ) ;
#27036 = CARTESIAN_POINT ( 'NONE',  ( 21.33283665240000104, -96.53848370399998657, 1.142368493430000020 ) ) ;
#27037 = DIRECTION ( 'NONE',  ( 1.000000000000000000, 0.000000000000000000, 0.000000000000000000 ) ) ;
#27038 = LINE ( 'NONE', #2567, #601 ) ;
#27039 = DIRECTION ( 'NONE',  ( 1.000000000000000000, 0.000000000000000000, 0.000000000000000000 ) ) ;
#27040 = CARTESIAN_POINT ( 'NONE',  ( 21.83114860719999939, -37.33500412619999764, -8.564557754590000016 ) ) ;
#27041 = CARTESIAN_POINT ( 'NONE',  ( 16.76297209009999989, -99.69348480060000384, 4.363466760120000565 ) ) ;
#27042 = ORIENTED_EDGE ( 'NONE', *, *, #9583, .F. ) ;
#27043 = CARTESIAN_POINT ( 'NONE',  ( -7.250123090889999844, -74.26791556519999915, -40.35962647450000418 ) ) ;
#27044 = CARTESIAN_POINT ( 'NONE',  ( 29.28732071508218837, -74.32953776423283898, -26.08572060009336724 ) ) ;
#27045 = CARTESIAN_POINT ( 'NONE',  ( -21.73574830329999941, -95.72998414210000817, -5.474907084429999848 ) ) ;
#27046 = VERTEX_POINT ( 'NONE', #540 ) ;
#27047 = CARTESIAN_POINT ( 'NONE',  ( -30.44581475448487140, -92.66972459461456424, 1.817249682291065538 ) ) ;
#27048 = DIRECTION ( 'NONE',  ( 0.9295286103719511139, 0.000000000000000000, 0.3687499999999862554 ) ) ;
#27049 = CARTESIAN_POINT ( 'NONE',  ( -5.860725082736318647, -96.53847999719242523, 20.54378296970569906 ) ) ;
#27050 = CARTESIAN_POINT ( 'NONE',  ( -11.82347332360000003, -101.2358105800000061, -9.579693020240000578 ) ) ;
#27051 = AXIS2_PLACEMENT_3D ( 'NONE', #20457, #22509, #11402 ) ;
#27052 = FACE_OUTER_BOUND ( 'NONE', #26175, .T. ) ;
#27053 = CARTESIAN_POINT ( 'NONE',  ( 23.48645807289999965, -94.80026553589999594, -6.710790866570000013 ) ) ;
#27054 = AXIS2_PLACEMENT_3D ( 'NONE', #5906, #3734, #19324 ) ;
#27055 = EDGE_CURVE ( 'NONE', #22777, #11422, #205, .T. ) ;
#27056 = CIRCLE ( 'NONE', #18214, 21.03431122519999974 ) ;
#27057 = CARTESIAN_POINT ( 'NONE',  ( 19.56503591259999908, -19.46390881170000142, 10.14212564559999841 ) ) ;
#27058 = CARTESIAN_POINT ( 'NONE',  ( -22.00722825609999944, -67.14423135289999323, 14.02040059770000191 ) ) ;
#27059 = CARTESIAN_POINT ( 'NONE',  ( -17.49077503611597351, -96.32082629555334563, 12.61788199362829488 ) ) ;
#27060 = ORIENTED_EDGE ( 'NONE', *, *, #24082, .T. ) ;
#27061 = CARTESIAN_POINT ( 'NONE',  ( -12.04566629249999998, -72.37490051890000586, -26.07979331039999948 ) ) ;
#27062 = CARTESIAN_POINT ( 'NONE',  ( -4.423592041350528525, -99.33527509803080591, 18.30618831894034670 ) ) ;
#27063 = CARTESIAN_POINT ( 'NONE',  ( 21.59803991680463042, -19.48549492419365237, 9.516754966957947204 ) ) ;
#27064 = CARTESIAN_POINT ( 'NONE',  ( -37.75000000000000000, -63.30468293320000583, 0.7216878364859999895 ) ) ;
#27065 = ORIENTED_EDGE ( 'NONE', *, *, #8540, .F. ) ;
#27066 = ADVANCED_FACE ( 'NONE', ( #7220 ), #12666, .T. ) ;
#27067 = CARTESIAN_POINT ( 'NONE',  ( 36.25000000000000000, -84.50000000000000000, 2.314797894279999601E-15 ) ) ;
#27068 = ORIENTED_EDGE ( 'NONE', *, *, #21796, .F. ) ;
#27069 = FACE_OUTER_BOUND ( 'NONE', #6503, .T. ) ;
#27070 = DIRECTION ( 'NONE',  ( 0.000000000000000000, 1.000000000000000000, 0.000000000000000000 ) ) ;
#27071 = DIRECTION ( 'NONE',  ( 1.000000000000000000, 0.000000000000000000, -6.106226635439993914E-16 ) ) ;
#27072 = AXIS2_PLACEMENT_3D ( 'NONE', #27716, #16764, #7476 ) ;
#27073 = CARTESIAN_POINT ( 'NONE',  ( 2.683228843229999772, -93.81034071199999858, 24.85754899019999797 ) ) ;
#27074 = AXIS2_PLACEMENT_3D ( 'NONE', #3013, #18591, #12153 ) ;
#27075 = ORIENTED_EDGE ( 'NONE', *, *, #12273, .F. ) ;
#27076 = ORIENTED_EDGE ( 'NONE', *, *, #22012, .F. ) ;
#27077 = CARTESIAN_POINT ( 'NONE',  ( -22.77778991426668043, -70.31271151318118484, 15.47469272077778335 ) ) ;
#27078 = CARTESIAN_POINT ( 'NONE',  ( -11.77049175740000209, -94.59276292389999696, -20.68200892780000189 ) ) ;
#27079 = CARTESIAN_POINT ( 'NONE',  ( 47.06797221370000273, -74.41279298919998553, -1.870483754820000177 ) ) ;
#27080 = VERTEX_POINT ( 'NONE', #17993 ) ;
#27081 = LINE ( 'NONE', #23140, #9433 ) ;
#27082 = CARTESIAN_POINT ( 'NONE',  ( -38.25000000000000000, -64.47022873560000278, -1.587713240270000048 ) ) ;
#27083 = CARTESIAN_POINT ( 'NONE',  ( 8.607506958290001009, -36.72040101139999990, -21.55953475569999966 ) ) ;
#27084 = CARTESIAN_POINT ( 'NONE',  ( -11.73664949370000166, -94.54719310899999130, -20.76899502859999913 ) ) ;
#27085 = FACE_OUTER_BOUND ( 'NONE', #19908, .T. ) ;
#27086 = ORIENTED_EDGE ( 'NONE', *, *, #6468, .T. ) ;
#27087 = EDGE_CURVE ( 'NONE', #8439, #18617, #21016, .T. ) ;
#27088 = CARTESIAN_POINT ( 'NONE',  ( 36.29003938660000017, -73.99962328729999683, -14.01560472500000110 ) ) ;
#27089 = ADVANCED_FACE ( 'NONE', ( #8071 ), #17591, .F. ) ;
#27090 = CARTESIAN_POINT ( 'NONE',  ( -16.97397862119999701, -99.68179698959998802, 2.927883187840000012 ) ) ;
#27091 = CARTESIAN_POINT ( 'NONE',  ( -40.70731707320000226, -74.50000000000000000, 7.215414233289999757 ) ) ;
#27092 = CARTESIAN_POINT ( 'NONE',  ( -21.82150020430000126, -74.12815218200000800, -32.45709266180000441 ) ) ;
#27093 = AXIS2_PLACEMENT_3D ( 'NONE', #10128, #12599, #3593 ) ;
#27094 = ORIENTED_EDGE ( 'NONE', *, *, #21643, .F. ) ;
#27095 = LINE ( 'NONE', #20826, #25681 ) ;
#27096 = ADVANCED_FACE ( 'NONE', ( #17340 ), #17727, .F. ) ;
#27097 = DIRECTION ( 'NONE',  ( 0.000000000000000000, 1.000000000000000000, 0.000000000000000000 ) ) ;
#27098 = AXIS2_PLACEMENT_3D ( 'NONE', #27287, #9191, #13569 ) ;
#27099 = DIRECTION ( 'NONE',  ( 0.5000000000001900702, 0.000000000000000000, -0.8660254037843290176 ) ) ;
#27100 = DIRECTION ( 'NONE',  ( -1.000000000000000000, 0.000000000000000000, 0.000000000000000000 ) ) ;
#27101 = ORIENTED_EDGE ( 'NONE', *, *, #26378, .T. ) ;
#27102 = CARTESIAN_POINT ( 'NONE',  ( -1.598721155459999804E-14, -11.00000000000000000, 50.00000000000000000 ) ) ;
#27103 = DIRECTION ( 'NONE',  ( 0.9704142011833033488, 0.000000000000000000, 0.2414462220490755373 ) ) ;
#27104 = DIRECTION ( 'NONE',  ( 0.000000000000000000, 1.000000000000000000, 0.000000000000000000 ) ) ;
#27105 = CARTESIAN_POINT ( 'NONE',  ( 15.62925250406422428, -101.5740747342780139, 3.683045828202760497 ) ) ;
#27106 = CARTESIAN_POINT ( 'NONE',  ( -11.35954001540000036, -74.00000000000000000, 47.25000000000000000 ) ) ;
#27107 = ORIENTED_EDGE ( 'NONE', *, *, #16722, .T. ) ;
#27108 = CARTESIAN_POINT ( 'NONE',  ( 46.66864852690000021, -79.99872154319999140, -3.727018626880000074 ) ) ;
#27109 = B_SPLINE_SURFACE_WITH_KNOTS ( 'NONE', 5, 5, ( 
 ( #10437, #5671, #21399, #28229, #23584, #26051, #6081, #3904, #14957 ),
 ( #21680, #16745, #25642, #5938, #23867, #14551, #16893, #23456, #3495 ),
 ( #21263, #1317, #27963, #5810, #14689, #3628, #1458, #10299, #17024 ),
 ( #25912, #14820, #4631, #8554, #2163, #26342, #137, #4186, #28800 ),
 ( #6368, #17457, #13061, #15235, #13214, #19771, #22122, #15836, #21970 ),
 ( #24447, #24154, #2021, #10860, #2461, #13355, #15541, #28652, #13502 ),
 ( #20074, #2607, #22414, #22259, #4482, #8683, #10999, #4340, #24747 ),
 ( #17894, #2306, #4782, #20219, #26933, #13661, #11315, #6973, #9132 ),
 ( #17601, #26489, #6526, #8986, #290, #11156, #26791, #15385, #18035 ) ),
 .UNSPECIFIED., .F., .F., .F.,
 ( 6, 3, 6 ),
 ( 6, 3, 6 ),
 ( 7.186332008800000004, 18.82033377109999961, 25.08217526889999860 ),
 ( 0.000000000000000000, 0.2500000000000000000, 0.5000000000000000000 ),
 .UNSPECIFIED. ) ;
#27110 = CARTESIAN_POINT ( 'NONE',  ( -11.35747017449999952, -60.48499519860000362, -21.31231279229999842 ) ) ;
#27111 = CARTESIAN_POINT ( 'NONE',  ( 24.57984581210000030, -66.63210100880000653, -8.034882954890001372 ) ) ;
#27112 = CARTESIAN_POINT ( 'NONE',  ( 10.20110288159999890, -84.50000000000000000, 41.00000000000000000 ) ) ;
#27113 = ORIENTED_EDGE ( 'NONE', *, *, #16222, .T. ) ;
#27114 = B_SPLINE_CURVE_WITH_KNOTS ( 'NONE', 5,
 ( #24104, #13013, #21924, #28747, #1975, #10819, #8648, #17550, #18284 ),
 .UNSPECIFIED., .F., .F.,
 ( 6, 3, 6 ),
 ( 43.40831274110000493, 61.94013117540000479, 64.87293781380000723 ),
 .UNSPECIFIED. ) ;
#27115 = VECTOR ( 'NONE', #25581, 1000.000000000000000 ) ;
#27116 = EDGE_CURVE ( 'NONE', #23532, #1349, #17266, .T. ) ;
#27117 = VERTEX_POINT ( 'NONE', #23380 ) ;
#27118 = CARTESIAN_POINT ( 'NONE',  ( -13.49470513559999851, -57.43018267549999933, 20.74700234780000230 ) ) ;
#27119 = CARTESIAN_POINT ( 'NONE',  ( -21.74262969930000011, -74.09723562380000317, -32.46276855370000192 ) ) ;
#27120 = ORIENTED_EDGE ( 'NONE', *, *, #364, .T. ) ;
#27121 = TOROIDAL_SURFACE ( 'NONE', #23390, 21.03431122519999974, 1.000000000000000000 ) ;
#27122 = DIRECTION ( 'NONE',  ( 1.000000000000000000, 0.000000000000000000, 0.000000000000000000 ) ) ;
#27123 = CARTESIAN_POINT ( 'NONE',  ( 3.242442617403691330, -93.08384138313282108, -28.92776005519338511 ) ) ;
#27124 = CARTESIAN_POINT ( 'NONE',  ( -29.13203926110000097, -92.50000647099999185, 5.968911360329999916 ) ) ;
#27125 = CARTESIAN_POINT ( 'NONE',  ( -40.65756524500000069, -65.56519245710001087, -2.400371413390000264 ) ) ;
#27126 = CARTESIAN_POINT ( 'NONE',  ( 24.48314189319999912, -69.76823842119999597, 12.05682714019999935 ) ) ;
#27127 = ORIENTED_EDGE ( 'NONE', *, *, #21252, .F. ) ;
#27128 = CARTESIAN_POINT ( 'NONE',  ( -7.120447010050000358, -111.0000000000000000, 15.21641332169999927 ) ) ;
#27129 = EDGE_CURVE ( 'NONE', #22982, #16224, #10260, .T. ) ;
#27130 = CARTESIAN_POINT ( 'NONE',  ( -38.23941415995982851, -65.68647126656233581, -1.441145490000594442 ) ) ;
#27131 = CARTESIAN_POINT ( 'NONE',  ( 37.29611236860000645, -80.00000000000000000, -13.75000000000000000 ) ) ;
#27132 = CARTESIAN_POINT ( 'NONE',  ( 40.27753662827743142, -74.17170883776950063, 7.244686332501536263 ) ) ;
#27133 = ORIENTED_EDGE ( 'NONE', *, *, #12765, .F. ) ;
#27134 = DIRECTION ( 'NONE',  ( 0.000000000000000000, 1.000000000000000000, 0.000000000000000000 ) ) ;
#27135 = FACE_OUTER_BOUND ( 'NONE', #18560, .T. ) ;
#27136 = EDGE_LOOP ( 'NONE', ( #2903, #11860, #20888, #21880 ) ) ;
#27137 = CARTESIAN_POINT ( 'NONE',  ( -18.24993397329999922, -95.76581571470001109, 13.57658235369999922 ) ) ;
#27138 = VECTOR ( 'NONE', #23521, 1000.000000000000000 ) ;
#27139 = AXIS2_PLACEMENT_3D ( 'NONE', #2196, #9027, #15272 ) ;
#27140 = CARTESIAN_POINT ( 'NONE',  ( -19.46796618480000163, -32.68478243029999675, 14.19297777630000112 ) ) ;
#27141 = CARTESIAN_POINT ( 'NONE',  ( -3.562216332169999777, -80.49999996399999702, 46.31451619710000500 ) ) ;
#27142 = CARTESIAN_POINT ( 'NONE',  ( -2.053743188970000031E-15, -82.25000000000000000, 47.25000000000000000 ) ) ;
#27143 = CARTESIAN_POINT ( 'NONE',  ( 23.43108223770000009, -60.27873802119999880, -9.526351984520001537 ) ) ;
#27144 = AXIS2_PLACEMENT_3D ( 'NONE', #13136, #14755, #10507 ) ;
#27145 = CARTESIAN_POINT ( 'NONE',  ( -12.06159284909973906, -57.47122623868258984, 20.23241278189946257 ) ) ;
#27146 = VERTEX_POINT ( 'NONE', #16383 ) ;
#27147 = EDGE_CURVE ( 'NONE', #321, #22026, #3287, .T. ) ;
#27148 = CARTESIAN_POINT ( 'NONE',  ( 28.66244647610000129, -93.00000000000000000, 10.42660836539999991 ) ) ;
#27149 = CARTESIAN_POINT ( 'NONE',  ( -1.314504061159999897E-13, -19.46510050329999686, -1.119104808819999722E-13 ) ) ;
#27150 = AXIS2_PLACEMENT_3D ( 'NONE', #23482, #3248, #19237 ) ;
#27151 = CARTESIAN_POINT ( 'NONE',  ( 12.42071132350000084, -98.30615006589998472, 14.97838199649999957 ) ) ;
#27152 = ORIENTED_EDGE ( 'NONE', *, *, #669, .F. ) ;
#27153 = CARTESIAN_POINT ( 'NONE',  ( 7.250123090889999844, -74.26791556519999915, 40.35962647450000418 ) ) ;
#27154 = CARTESIAN_POINT ( 'NONE',  ( -11.49546490490405048, -95.15473665344634924, -21.39080332819893471 ) ) ;
#27155 = CARTESIAN_POINT ( 'NONE',  ( -20.43932202180000246, -94.59276292389999696, 12.18704577789999988 ) ) ;
#27156 = CARTESIAN_POINT ( 'NONE',  ( 6.061325012380000210, -92.50000460620000808, 29.15556959710000129 ) ) ;
#27157 = CARTESIAN_POINT ( 'NONE',  ( -20.56018235820000228, -57.40875686090000585, 14.85415984670000000 ) ) ;
#27158 = CARTESIAN_POINT ( 'NONE',  ( 8.476165110749999343, -37.64222909819999785, -21.78580730850000080 ) ) ;
#27159 = EDGE_CURVE ( 'NONE', #12707, #13695, #21196, .T. ) ;
#27160 = AXIS2_PLACEMENT_3D ( 'NONE', #1601, #1878, #14556 ) ;
#27161 = CARTESIAN_POINT ( 'NONE',  ( -36.79999999999999716, -65.14977478849999670, -0.1732050807570000017 ) ) ;
#27162 = ORIENTED_EDGE ( 'NONE', *, *, #22553, .T. ) ;
#27163 = CARTESIAN_POINT ( 'NONE',  ( -0.7163235813839999855, -101.3256027139999986, -15.89054958740000068 ) ) ;
#27164 = CARTESIAN_POINT ( 'NONE',  ( 9.356041104380000917, -84.00000000000000000, -37.60355029590000697 ) ) ;
#27165 = DIRECTION ( 'NONE',  ( 0.000000000000000000, 1.000000000000000000, 0.000000000000000000 ) ) ;
#27166 = CARTESIAN_POINT ( 'NONE',  ( -2.554621587543492556, -19.48534489990609231, -23.45393302294781535 ) ) ;
#27167 = CARTESIAN_POINT ( 'NONE',  ( -15.32074598660000042, -101.1659465879999971, 4.659563583299999756 ) ) ;
#27168 = CARTESIAN_POINT ( 'NONE',  ( -14.48558484980151206, -100.7167551675964603, -8.980145358784431764 ) ) ;
#27169 = CARTESIAN_POINT ( 'NONE',  ( 40.70731707320000226, -82.25000000000000000, 7.215414233289999757 ) ) ;
#27170 = AXIS2_PLACEMENT_3D ( 'NONE', #22065, #17253, #76 ) ;
#27171 = CARTESIAN_POINT ( 'NONE',  ( 11.85491415629929968, -101.4218099525233470, -10.99807908417638380 ) ) ;
#27172 = CARTESIAN_POINT ( 'NONE',  ( 22.33592606139999859, -44.89607405940000007, -8.998660423470001390 ) ) ;
#27173 = CARTESIAN_POINT ( 'NONE',  ( 24.66243531188380089, -93.09721478938284633, -15.27777790653344958 ) ) ;
#27174 = DIRECTION ( 'NONE',  ( -0.3438555744121192803, 0.06995790998172438102, 0.9364129616663261491 ) ) ;
#27175 = ORIENTED_EDGE ( 'NONE', *, *, #22963, .F. ) ;
#27176 = DIRECTION ( 'NONE',  ( 0.000000000000000000, 1.000000000000000000, 0.000000000000000000 ) ) ;
#27177 = CARTESIAN_POINT ( 'NONE',  ( -32.67527180710000323, -74.50000000430000568, -22.00249031559999935 ) ) ;
#27178 = CARTESIAN_POINT ( 'NONE',  ( -22.45768892722265164, -79.92187437579165987, -32.73741433150124180 ) ) ;
#27179 = CIRCLE ( 'NONE', #9485, 9.499999999999998224 ) ;
#27180 = CARTESIAN_POINT ( 'NONE',  ( -15.42363573210000105, -67.46051717960000360, 22.84488635619999997 ) ) ;
#27181 = CARTESIAN_POINT ( 'NONE',  ( 20.01429421219999938, -35.44265673480000345, -8.963580811669999093 ) ) ;
#27182 = CARTESIAN_POINT ( 'NONE',  ( -18.87095359252083782, -92.56168502752186100, 22.85581819520699653 ) ) ;
#27183 = CARTESIAN_POINT ( 'NONE',  ( -18.99756495820000168, -92.50000000000000000, -23.62136188200000220 ) ) ;
#27184 = CARTESIAN_POINT ( 'NONE',  ( 21.13310776459999829, -36.23917065820000261, -8.855030636489999551 ) ) ;
#27185 = CARTESIAN_POINT ( 'NONE',  ( -14.59383839804472416, -94.00303307107726880, -21.62085948234513211 ) ) ;
#27186 = CARTESIAN_POINT ( 'NONE',  ( -40.70731707320000226, -74.50000000000000000, 7.215414233289999757 ) ) ;
#27187 = EDGE_CURVE ( 'NONE', #11758, #22088, #4352, .T. ) ;
#27188 = CIRCLE ( 'NONE', #28548, 30.50000000000000000 ) ;
#27189 = CARTESIAN_POINT ( 'NONE',  ( -38.00919334667170091, -63.35144866725882196, 0.9204318061653798955 ) ) ;
#27190 = CARTESIAN_POINT ( 'NONE',  ( 16.63506097750000023, -100.0482783049999966, 4.353522604860000200 ) ) ;
#27191 = EDGE_LOOP ( 'NONE', ( #11691, #16891, #16744, #1578, #20854, #19015, #18416, #26360, #1648, #12497, #21025, #11959, #649, #23109, #6687, #27823, #19741, #23567, #23954, #9519, #1520, #25, #16391, #19232, #18451, #5524, #23126, #12184 ) ) ;
#27192 = CARTESIAN_POINT ( 'NONE',  ( -19.78028125209999999, -96.96081043319999537, -6.989363499150000436 ) ) ;
#27193 = ORIENTED_EDGE ( 'NONE', *, *, #14536, .T. ) ;
#27194 = EDGE_CURVE ( 'NONE', #27454, #6381, #9019, .T. ) ;
#27195 = CARTESIAN_POINT ( 'NONE',  ( 20.34628061889999984, -52.63293862049999916, 11.13082833170000008 ) ) ;
#27196 = ADVANCED_FACE ( 'NONE', ( #22149 ), #7048, .T. ) ;
#27197 = FACE_OUTER_BOUND ( 'NONE', #23114, .T. ) ;
#27198 = CARTESIAN_POINT ( 'NONE',  ( -43.07153896660000214, -63.00000000000000000, -1.677989385109999843 ) ) ;
#27199 = DIRECTION ( 'NONE',  ( 0.8775825618903722036, 0.000000000000000000, -0.4794255386042041156 ) ) ;
#27200 = DIRECTION ( 'NONE',  ( 0.000000000000000000, 1.000000000000000000, 0.000000000000000000 ) ) ;
#27201 = CARTESIAN_POINT ( 'NONE',  ( 18.78522494180000280, -18.50000000000000000, 9.483810324729999408 ) ) ;
#27202 = CARTESIAN_POINT ( 'NONE',  ( -3.067686975420000017, -99.66156977119999283, -17.02465262619999820 ) ) ;
#27203 = CARTESIAN_POINT ( 'NONE',  ( -17.14077040652199813, -97.41018742068575875, 10.60857521878771870 ) ) ;
#27204 = ORIENTED_EDGE ( 'NONE', *, *, #24466, .F. ) ;
#27205 = AXIS2_PLACEMENT_3D ( 'NONE', #11597, #9419, #20505 ) ;
#27206 = CARTESIAN_POINT ( 'NONE',  ( -26.69328098980000163, -74.50000000000000000, -35.88566914520000495 ) ) ;
#27207 = CARTESIAN_POINT ( 'NONE',  ( 9.014750546150001043, -22.53353178400000445, -19.04514867530000188 ) ) ;
#27208 = CARTESIAN_POINT ( 'NONE',  ( 7.905782043786379276, -101.5455496411810259, 13.99933444791012072 ) ) ;
#27209 = CARTESIAN_POINT ( 'NONE',  ( -5.298192075760000286, -100.9197081840000010, 14.69882727599999939 ) ) ;
#27210 = DIRECTION ( 'NONE',  ( 1.000000000000000000, 0.000000000000000000, 0.000000000000000000 ) ) ;
#27211 = VERTEX_POINT ( 'NONE', #20103 ) ;
#27212 = VECTOR ( 'NONE', #6907, 1000.000000000000000 ) ;
#27213 = CARTESIAN_POINT ( 'NONE',  ( 26.33530480068390744, -92.82668962668526547, -15.38511375170930862 ) ) ;
#27214 = ORIENTED_EDGE ( 'NONE', *, *, #2417, .T. ) ;
#27215 = DIRECTION ( 'NONE',  ( 1.000000000000000000, 0.000000000000000000, 0.000000000000000000 ) ) ;
#27216 = CARTESIAN_POINT ( 'NONE',  ( -0.7975586053140000242, -96.07623048680000011, 23.00905320750000271 ) ) ;
#27217 = CARTESIAN_POINT ( 'NONE',  ( 8.056208598280001354, -92.64865434429998459, 26.82756782219999891 ) ) ;
#27218 = ORIENTED_EDGE ( 'NONE', *, *, #16888, .F. ) ;
#27219 = EDGE_CURVE ( 'NONE', #2458, #10205, #15716, .T. ) ;
#27220 = CARTESIAN_POINT ( 'NONE',  ( -4.710490229966223907, -99.82487968069240480, 16.41387846790747673 ) ) ;
#27221 = AXIS2_PLACEMENT_3D ( 'NONE', #23936, #8330, #25711 ) ;
#27222 = CARTESIAN_POINT ( 'NONE',  ( -24.78124722104226763, -94.60934249595302958, -3.488298834054989861 ) ) ;
#27223 = DIRECTION ( 'NONE',  ( 0.000000000000000000, 1.000000000000000000, 0.000000000000000000 ) ) ;
#27224 = CARTESIAN_POINT ( 'NONE',  ( 10.18473603500000024, -36.00000000000000000, -20.58226785680000148 ) ) ;
#27225 = VERTEX_POINT ( 'NONE', #19941 ) ;
#27226 = CARTESIAN_POINT ( 'NONE',  ( 7.248098695798295132, -73.87273571702228026, -39.83391879123477963 ) ) ;
#27227 = DIRECTION ( 'NONE',  ( 0.4794255386042036715, 0.000000000000000000, 0.8775825618903724257 ) ) ;
#27228 = EDGE_CURVE ( 'NONE', #20825, #19738, #10711, .T. ) ;
#27229 = VERTEX_POINT ( 'NONE', #2337 ) ;
#27230 = CARTESIAN_POINT ( 'NONE',  ( -4.608126179330000127, -98.80330295420000652, -19.06616812880000111 ) ) ;
#27231 = AXIS2_PLACEMENT_3D ( 'NONE', #12244, #16623, #21156 ) ;
#27232 = CARTESIAN_POINT ( 'NONE',  ( 9.038647564319999717, -35.72724395809999720, -19.55068592700000352 ) ) ;
#27233 = DIRECTION ( 'NONE',  ( 0.000000000000000000, 1.000000000000000000, 0.000000000000000000 ) ) ;
#27234 = ORIENTED_EDGE ( 'NONE', *, *, #12072, .F. ) ;
#27235 = DIRECTION ( 'NONE',  ( 0.000000000000000000, 1.000000000000000000, 0.000000000000000000 ) ) ;
#27236 = CARTESIAN_POINT ( 'NONE',  ( -2.783420023329999715, -64.17227325300000018, -26.33714589019999863 ) ) ;
#27237 = CARTESIAN_POINT ( 'NONE',  ( -21.99985828019999801, -74.00000000000000000, -31.89935321680000158 ) ) ;
#27238 = ORIENTED_EDGE ( 'NONE', *, *, #1529, .F. ) ;
#27239 = CARTESIAN_POINT ( 'NONE',  ( -0.5372032561875097478, -32.73217874168935992, -22.49059537401083375 ) ) ;
#27240 = CARTESIAN_POINT ( 'NONE',  ( -43.20000000000000284, -63.00000000000000000, 0.1732050807559999961 ) ) ;
#27241 = CARTESIAN_POINT ( 'NONE',  ( 36.74280283558181992, -74.40473351797265877, -14.55378675820746892 ) ) ;
#27242 = ORIENTED_EDGE ( 'NONE', *, *, #11749, .F. ) ;
#27243 = DIRECTION ( 'NONE',  ( 0.000000000000000000, 1.000000000000000000, 0.000000000000000000 ) ) ;
#27244 = CIRCLE ( 'NONE', #4411, 1.999999999999999556 ) ;
#27245 = CARTESIAN_POINT ( 'NONE',  ( 23.42373825549999822, -62.44588796569999545, 10.52566358100000166 ) ) ;
#27246 = CARTESIAN_POINT ( 'NONE',  ( 8.427784894169999319, -35.19242348989999414, -20.91698756690000138 ) ) ;
#27247 = CARTESIAN_POINT ( 'NONE',  ( 15.83435892164885139, -101.1884902310803795, 4.101762063882318010 ) ) ;
#27248 = CARTESIAN_POINT ( 'NONE',  ( -13.32816333360000094, -99.92967571559999840, -11.12411022969999941 ) ) ;
#27249 = EDGE_LOOP ( 'NONE', ( #25494, #14817, #7309, #2573 ) ) ;
#27250 = FACE_OUTER_BOUND ( 'NONE', #22170, .T. ) ;
#27251 = CARTESIAN_POINT ( 'NONE',  ( -11.37864349189999835, -18.61797544070000043, 18.64968536590000170 ) ) ;
#27252 = CARTESIAN_POINT ( 'NONE',  ( -11.54937042210000087, -60.21420103860000239, -22.76847067690000159 ) ) ;
#27253 = EDGE_CURVE ( 'NONE', #14280, #25949, #26127, .T. ) ;
#27254 = DIRECTION ( 'NONE',  ( -0.9387128607161810967, 0.000000000000000000, -0.3447001089730664103 ) ) ;
#27255 = CARTESIAN_POINT ( 'NONE',  ( 26.41739731730000074, -71.28695100890000447, -9.226526782039998764 ) ) ;
#27256 = CARTESIAN_POINT ( 'NONE',  ( 4.685572449352821245, -93.74883191391012360, 26.22100713583913034 ) ) ;
#27257 = ORIENTED_EDGE ( 'NONE', *, *, #25673, .F. ) ;
#27258 = EDGE_CURVE ( 'NONE', #7956, #9479, #2639, .T. ) ;
#27259 = CARTESIAN_POINT ( 'NONE',  ( -14.81112187414681003, -74.50000000000001421, 36.34845292753433199 ) ) ;
#27260 = CARTESIAN_POINT ( 'NONE',  ( -41.75000000000000000, -65.63577453799999262, -1.587713240270000048 ) ) ;
#27261 = EDGE_LOOP ( 'NONE', ( #7748, #16996, #27994, #17427 ) ) ;
#27262 = FACE_OUTER_BOUND ( 'NONE', #3800, .T. ) ;
#27263 = ORIENTED_EDGE ( 'NONE', *, *, #16851, .T. ) ;
#27264 = EDGE_CURVE ( 'NONE', #14226, #11312, #2336, .T. ) ;
#27265 = CARTESIAN_POINT ( 'NONE',  ( -2.578307999469999778, -52.56313962710000709, -25.11373953509999879 ) ) ;
#27266 = ADVANCED_FACE ( 'NONE', ( #13242 ), #4509, .T. ) ;
#27267 = CARTESIAN_POINT ( 'NONE',  ( 7.202169761539999548, -101.2530994060000040, 13.37848089600000101 ) ) ;
#27268 = CARTESIAN_POINT ( 'NONE',  ( -11.41594931139999858, -19.46510050329999686, -18.84569254350000023 ) ) ;
#27269 = CARTESIAN_POINT ( 'NONE',  ( -16.78865735879999832, -72.00000000000000000, 25.46808810279999946 ) ) ;
#27270 = CARTESIAN_POINT ( 'NONE',  ( -10.05111287380000107, -18.50000000000000000, -21.88335580340000064 ) ) ;
#27271 = CARTESIAN_POINT ( 'NONE',  ( 9.708867067583597077, -61.04180997458320945, -23.92438532451274114 ) ) ;
#27272 = EDGE_LOOP ( 'NONE', ( #10748, #3215, #26478, #4220 ) ) ;
#27273 = DIRECTION ( 'NONE',  ( 1.000000000000000000, 0.000000000000000000, 0.000000000000000000 ) ) ;
#27274 = FACE_OUTER_BOUND ( 'NONE', #92, .T. ) ;
#27275 = DIRECTION ( 'NONE',  ( -1.000000000000000000, 0.000000000000000000, 0.000000000000000000 ) ) ;
#27276 = ORIENTED_EDGE ( 'NONE', *, *, #22557, .F. ) ;
#27277 = B_SPLINE_CURVE_WITH_KNOTS ( 'NONE', 3,
 ( #4221, #7156, #6713, #13095, #6562, #15876 ),
 .UNSPECIFIED., .F., .F.,
 ( 4, 2, 4 ),
 ( 0.000000000000000000, 0.5000000000000000000, 1.000000000000000000 ),
 .UNSPECIFIED. ) ;
#27278 = VECTOR ( 'NONE', #21601, 1000.000000000000000 ) ;
#27279 = CARTESIAN_POINT ( 'NONE',  ( 20.62325427951632051, -19.20927481666025827, -7.731222864529065930 ) ) ;
#27280 = CARTESIAN_POINT ( 'NONE',  ( 0.000000000000000000, -10.50000000000000000, 0.000000000000000000 ) ) ;
#27281 = DIRECTION ( 'NONE',  ( 0.9057388881967942673, 0.000000000000000000, 0.4238361315509041050 ) ) ;
#27282 = ORIENTED_EDGE ( 'NONE', *, *, #14394, .F. ) ;
#27283 = CARTESIAN_POINT ( 'NONE',  ( -3.134349037060000231, -94.63960343439998724, 23.52861282910000185 ) ) ;
#27284 = EDGE_CURVE ( 'NONE', #12242, #8854, #4657, .T. ) ;
#27285 = DIRECTION ( 'NONE',  ( 1.000000000000000000, 0.000000000000000000, 0.000000000000000000 ) ) ;
#27286 = CARTESIAN_POINT ( 'NONE',  ( -7.893157158527718487, -99.84800943042134236, 15.42810193944218788 ) ) ;
#27287 = CARTESIAN_POINT ( 'NONE',  ( -40.00000000000000000, -66.00000000000000000, 0.000000000000000000 ) ) ;
#27288 = DIRECTION ( 'NONE',  ( 0.4794255386042040046, 0.000000000000000000, 0.8775825618903722036 ) ) ;
#27289 =( NAMED_UNIT ( * ) SI_UNIT ( $, .STERADIAN. ) SOLID_ANGLE_UNIT ( ) );
#27290 = CARTESIAN_POINT ( 'NONE',  ( 6.888451955769999913, -99.53431386179998697, 15.99365555089999802 ) ) ;
#27292 = VERTEX_POINT ( 'NONE', #7002 ) ;
#27291 = EDGE_CURVE ( 'NONE', #17070, #2258, #21035, .T. ) ;
#27293 = ADVANCED_FACE ( 'NONE', ( #22002, #17779 ), #24330, .F. ) ;
#27294 = CARTESIAN_POINT ( 'NONE',  ( -19.59431174800317521, -18.62337006874626155, 14.76282611549721402 ) ) ;
#27295 = CARTESIAN_POINT ( 'NONE',  ( 20.45177504849999650, -36.01773751660000045, -9.130641075480001589 ) ) ;
#27296 = CARTESIAN_POINT ( 'NONE',  ( 15.04850482649999854, -97.41042756519999557, 15.29532899870000229 ) ) ;
#27297 = VERTEX_POINT ( 'NONE', #24776 ) ;
#27298 = CARTESIAN_POINT ( 'NONE',  ( 23.63266585800719355, -92.62938374233351624, -19.28077060567576240 ) ) ;
#27299 = DIRECTION ( 'NONE',  ( 0.7071067811865492381, 0.000000000000000000, -0.7071067811865457964 ) ) ;
#27300 = CARTESIAN_POINT ( 'NONE',  ( -8.034958860690000648, -100.1785804069999983, 14.58156101930000048 ) ) ;
#27301 = DIRECTION ( 'NONE',  ( 0.000000000000000000, -1.000000000000000000, 0.000000000000000000 ) ) ;
#27302 = CARTESIAN_POINT ( 'NONE',  ( -20.88544710529999904, -61.59957509759999539, 15.07454172879999987 ) ) ;
#27303 = CARTESIAN_POINT ( 'NONE',  ( 7.999160519940001102, -37.31099427210000385, -21.56623231000000374 ) ) ;
#27304 = CARTESIAN_POINT ( 'NONE',  ( 8.783950479490158614, -19.48412239595453599, -19.74263315380339989 ) ) ;
#27305 = EDGE_LOOP ( 'NONE', ( #6309, #22075, #23192, #4679 ) ) ;
#27306 = CARTESIAN_POINT ( 'NONE',  ( -39.84323359140208254, -73.87844996482343163, 7.248307137522745691 ) ) ;
#27307 = CARTESIAN_POINT ( 'NONE',  ( 24.46521773039999914, -18.62337009750000050, 1.825159675170000106 ) ) ;
#27308 = CARTESIAN_POINT ( 'NONE',  ( 21.47791241899999903, -36.56811125080000835, -7.356933755090000027 ) ) ;
#27309 = ORIENTED_EDGE ( 'NONE', *, *, #7227, .F. ) ;
#27310 = CARTESIAN_POINT ( 'NONE',  ( -2.605118868831385104, -19.48886652629414229, -23.65890925434035452 ) ) ;
#27311 = B_SPLINE_CURVE_WITH_KNOTS ( 'NONE', 3,
 ( #6788, #13917, #11566, #25151, #13768, #20637, #2713, #20182, #24552, #20478, #13318 ),
 .UNSPECIFIED., .F., .F.,
 ( 4, 1, 1, 1, 2, 2, 4 ),
 ( 0.000000000000000000, 0.2499999999999971689, 0.3749999999999957812, 0.4374999999999950595, 0.4687499999999949485, 0.4999999999999948930, 1.000000000000000000 ),
 .UNSPECIFIED. ) ;
#27312 = CARTESIAN_POINT ( 'NONE',  ( -15.36947541530000017, -101.0685850650000077, 4.769133107380000069 ) ) ;
#27313 = CARTESIAN_POINT ( 'NONE',  ( -2.363861431289999704, -52.59522851920000619, -24.20187825489999867 ) ) ;
#27314 = CARTESIAN_POINT ( 'NONE',  ( -19.01364933584116557, -98.08323605845289705, -7.561538557556316320 ) ) ;
#27315 = CARTESIAN_POINT ( 'NONE',  ( -38.25000000000810729, -63.07121106306455260, -2.719955530748988881 ) ) ;
#27316 = ADVANCED_FACE ( 'NONE', ( #6397 ), #2049, .T. ) ;
#27317 = DIRECTION ( 'NONE',  ( 0.000000000000000000, 1.000000000000000000, 0.000000000000000000 ) ) ;
#27318 = CARTESIAN_POINT ( 'NONE',  ( 22.87094945020000125, -44.87455296059999910, -9.357772773720000714 ) ) ;
#27319 = CARTESIAN_POINT ( 'NONE',  ( 10.12409544680074269, -100.1470164126797044, 14.62208593278274726 ) ) ;
#27320 = DIRECTION ( 'NONE',  ( 0.9839596076661281110, 0.000000000000000000, 0.1783913968820229901 ) ) ;
#27321 = VERTEX_POINT ( 'NONE', #4216 ) ;
#27322 = CARTESIAN_POINT ( 'NONE',  ( 6.563397635340000313, -101.1700440390000040, 13.82292916689999984 ) ) ;
#27323 = CARTESIAN_POINT ( 'NONE',  ( -18.13313556475285537, -92.50000170997873283, -23.79371526278151094 ) ) ;
#27324 = CARTESIAN_POINT ( 'NONE',  ( 7.921626121120000086, -101.0233750200000031, 13.74344063909999925 ) ) ;
#27325 = CARTESIAN_POINT ( 'NONE',  ( -12.08078259732632631, -68.11638242249664188, -25.01700482484572774 ) ) ;
#27326 = CARTESIAN_POINT ( 'NONE',  ( 9.018303738449999329, -35.73233772869999569, -20.14104784029999706 ) ) ;
#27327 = CARTESIAN_POINT ( 'NONE',  ( 36.24656994149999889, -79.00000000000000000, -15.05817610060000078 ) ) ;
#27328 = DIRECTION ( 'NONE',  ( 0.09756097560976705052, 0.000000000000000000, -0.9952295494196654602 ) ) ;
#27329 = CARTESIAN_POINT ( 'NONE',  ( 20.16453947749999998, -36.00000000000000000, -9.644867042430000481 ) ) ;
#27330 = CARTESIAN_POINT ( 'NONE',  ( 0.3669127390019999435, -92.63555401869999173, -30.25482938650000264 ) ) ;
#27331 = CARTESIAN_POINT ( 'NONE',  ( 16.83483089839999991, -99.92967571559999840, 4.239603441799999928 ) ) ;
#27332 = EDGE_LOOP ( 'NONE', ( #17880, #15381, #1661 ) ) ;
#27333 = CARTESIAN_POINT ( 'NONE',  ( -0.8216735279219999910, -65.07443093669999712, -25.13632616349999793 ) ) ;
#27334 = CARTESIAN_POINT ( 'NONE',  ( -40.50000000000000000, -63.30468293320000583, 2.309401076760000393 ) ) ;
#27335 = ORIENTED_EDGE ( 'NONE', *, *, #7224, .F. ) ;
#27336 = CARTESIAN_POINT ( 'NONE',  ( -30.45665982967346253, -92.62800705134041834, 1.627016164164003964 ) ) ;
#27337 = CARTESIAN_POINT ( 'NONE',  ( 0.6132859559569719954, -100.6338045025634784, -16.78345358886858207 ) ) ;
#27338 = CARTESIAN_POINT ( 'NONE',  ( -10.87473961043062509, -19.46454318506218328, 19.18358865193880192 ) ) ;
#27339 = CARTESIAN_POINT ( 'NONE',  ( 0.000000000000000000, -37.08699221940000257, 0.000000000000000000 ) ) ;
#27340 = CARTESIAN_POINT ( 'NONE',  ( 23.54313657600000198, -94.98812477599999227, -6.784142512209999865 ) ) ;
#27341 = CARTESIAN_POINT ( 'NONE',  ( -7.250083186824390680, -73.98707088453728886, -40.01432744588630896 ) ) ;
#27342 = CARTESIAN_POINT ( 'NONE',  ( -14.32651846709999965, -74.09825332389999630, 36.37998168949999922 ) ) ;
#27343 = CARTESIAN_POINT ( 'NONE',  ( 9.687968342419999601, -71.22032982880000418, -26.22375966410000103 ) ) ;
#27344 = CARTESIAN_POINT ( 'NONE',  ( 23.77988130051113203, -92.72722989462202747, -19.09888384160796804 ) ) ;
#27345 = B_SPLINE_SURFACE_WITH_KNOTS ( 'NONE', 5, 5, ( 
 ( #1677, #21911, #6315, #24088, #5887, #10515, #19714, #1961, #23809 ),
 ( #3989, #28601, #8349, #8632, #14901, #26428, #21762, #6455, #8214 ),
 ( #28045, #16972, #6021, #15322, #24240, #4276, #19430, #13151, #1812 ),
 ( #8082, #26290, #14766, #19574, #4125, #19299, #26142, #3851, #22060 ),
 ( #28314, #2109, #3712, #28181, #17250, #19159, #25861, #12571, #21483 ),
 ( #15040, #1541, #23955, #27163, #20450, #19850, #13593, #20298, #24681 ) ),
 .UNSPECIFIED., .F., .F., .F.,
 ( 6, 6 ),
 ( 6, 3, 6 ),
 ( 4.816191416739999731, 6.255250589890000157 ),
 ( 0.000000000000000000, 0.2500000000000000000, 0.5000000000000000000 ),
 .UNSPECIFIED. ) ;
#27346 = ORIENTED_EDGE ( 'NONE', *, *, #27656, .T. ) ;
#27347 = EDGE_CURVE ( 'NONE', #12588, #10083, #24475, .T. ) ;
#27348 = DIRECTION ( 'NONE',  ( 1.000000000000000000, 0.000000000000000000, 0.000000000000000000 ) ) ;
#27349 = CARTESIAN_POINT ( 'NONE',  ( 8.512197389749998067, -28.54984126589999960, -20.54345199129999600 ) ) ;
#27350 = DIRECTION ( 'NONE',  ( 0.4794255386042040046, 0.000000000000000000, 0.8775825618903722036 ) ) ;
#27351 = CARTESIAN_POINT ( 'NONE',  ( 38.62788659690000515, -73.50000000000000000, -7.627568735119999666 ) ) ;
#27352 = CARTESIAN_POINT ( 'NONE',  ( -38.62788781560000473, -74.00000025069999765, -7.627567457969999687 ) ) ;
#27353 = ORIENTED_EDGE ( 'NONE', *, *, #12697, .F. ) ;
#27354 = EDGE_CURVE ( 'NONE', #11126, #11154, #3793, .T. ) ;
#27355 = TOROIDAL_SURFACE ( 'NONE', #14324, 0.5000000000000000000, 0.5000000000000000000 ) ;
#27356 = ORIENTED_EDGE ( 'NONE', *, *, #18879, .F. ) ;
#27357 = EDGE_CURVE ( 'NONE', #20804, #23088, #2409, .T. ) ;
#27358 = EDGE_CURVE ( 'NONE', #13005, #20039, #6103, .T. ) ;
#27359 = CYLINDRICAL_SURFACE ( 'NONE', #3034, 9.999999999999996447 ) ;
#27360 = AXIS2_PLACEMENT_3D ( 'NONE', #676, #25286, #27618 ) ;
#27361 = DIRECTION ( 'NONE',  ( 1.000000000000000000, 0.000000000000000000, 0.000000000000000000 ) ) ;
#27362 = CARTESIAN_POINT ( 'NONE',  ( 5.750078808689999654, -92.99020741600000406, 26.05463881579999708 ) ) ;
#27363 = ORIENTED_EDGE ( 'NONE', *, *, #18170, .T. ) ;
#27364 = CARTESIAN_POINT ( 'NONE',  ( 1.631276547419999945, -94.59276292389999696, 23.74086995720000104 ) ) ;
#27365 = CARTESIAN_POINT ( 'NONE',  ( -27.66037319239678283, -93.38817447838401620, 0.4406502884517963792 ) ) ;
#27366 = CARTESIAN_POINT ( 'NONE',  ( -23.24818410940000035, -92.50000000000000000, -18.83197690249999923 ) ) ;
#27367 = CARTESIAN_POINT ( 'NONE',  ( 10.86700788799999984, -36.00000000000000000, -21.35995475889999895 ) ) ;
#27368 = ORIENTED_EDGE ( 'NONE', *, *, #14277, .T. ) ;
#27369 = CARTESIAN_POINT ( 'NONE',  ( -27.18988201479999844, -22.09844555429999957, -49.77074518290000071 ) ) ;
#27370 = CARTESIAN_POINT ( 'NONE',  ( 22.86992907279976350, -57.41946977148945308, 10.24154027049986126 ) ) ;
#27371 = ORIENTED_EDGE ( 'NONE', *, *, #13175, .T. ) ;
#27372 = CIRCLE ( 'NONE', #12880, 0.5000000000000004441 ) ;
#27373 = CARTESIAN_POINT ( 'NONE',  ( -4.565529784469999797, -98.71594109849999654, -19.04035697939999849 ) ) ;
#27374 = DIRECTION ( 'NONE',  ( 0.000000000000000000, 1.000000000000000000, 0.000000000000000000 ) ) ;
#27375 = CIRCLE ( 'NONE', #6902, 55.67692378859999991 ) ;
#27376 = CARTESIAN_POINT ( 'NONE',  ( -2.143662412449999888, -70.80052042910000409, -27.67943948509999785 ) ) ;
#27377 = DIRECTION ( 'NONE',  ( 0.000000000000000000, 1.000000000000000000, 0.000000000000000000 ) ) ;
#27378 = ORIENTED_EDGE ( 'NONE', *, *, #28515, .F. ) ;
#27379 = CARTESIAN_POINT ( 'NONE',  ( 36.54166093210000810, -74.19847614699999383, -14.46229251740000166 ) ) ;
#27380 = CARTESIAN_POINT ( 'NONE',  ( -15.04954741829999953, -101.1221263650000139, 3.331427410760000374 ) ) ;
#27381 = CARTESIAN_POINT ( 'NONE',  ( 24.13573937880000031, -60.48499519869999830, 0.8202987023390000410 ) ) ;
#27382 = CARTESIAN_POINT ( 'NONE',  ( 36.32677412860000032, -74.12275851199999011, -14.57143996970000011 ) ) ;
#27383 = ORIENTED_EDGE ( 'NONE', *, *, #15198, .F. ) ;
#27384 = CIRCLE ( 'NONE', #7376, 3.750000000000000000 ) ;
#27385 = CARTESIAN_POINT ( 'NONE',  ( -19.41486357870000035, -39.36577621589999865, 11.81755283919999933 ) ) ;
#27386 = DIRECTION ( 'NONE',  ( 0.9639181000863472626, 0.000000000000000000, -0.2661989788220960884 ) ) ;
#27387 = CARTESIAN_POINT ( 'NONE',  ( -7.911401155084729631, -100.0559847774123625, 15.33800364961746787 ) ) ;
#27388 = ORIENTED_EDGE ( 'NONE', *, *, #6681, .T. ) ;
#27389 = ADVANCED_FACE ( 'NONE', ( #2929 ), #14135, .F. ) ;
#27390 = CARTESIAN_POINT ( 'NONE',  ( -10.66313611470000211, -93.32963169590000518, -23.55089348639999969 ) ) ;
#27391 = CARTESIAN_POINT ( 'NONE',  ( 21.64198627210000225, -62.93490527480000196, 11.11445933409999931 ) ) ;
#27392 = CARTESIAN_POINT ( 'NONE',  ( 8.965966767370000312, -34.65022614779999799, -19.90557425269999925 ) ) ;
#27393 = CARTESIAN_POINT ( 'NONE',  ( 16.44482720124391406, -100.3617719035428024, 4.355606921756608685 ) ) ;
#27394 = CARTESIAN_POINT ( 'NONE',  ( 13.80549142619667258, -99.84800943040862364, -10.47552699689475908 ) ) ;
#27395 = ORIENTED_EDGE ( 'NONE', *, *, #12576, .T. ) ;
#27396 = CARTESIAN_POINT ( 'NONE',  ( 45.84677419350000349, -80.50000000000000000, -4.286925650119999709 ) ) ;
#27397 = FACE_OUTER_BOUND ( 'NONE', #28134, .T. ) ;
#27398 = EDGE_CURVE ( 'NONE', #23842, #7500, #11792, .T. ) ;
#27399 = CIRCLE ( 'NONE', #18553, 18.14285714289999873 ) ;
#27400 = CIRCLE ( 'NONE', #13906, 23.36116116979999902 ) ;
#27401 = CARTESIAN_POINT ( 'NONE',  ( 24.36633741079999993, -66.46905249630000867, -9.136733449319999423 ) ) ;
#27402 = CARTESIAN_POINT ( 'NONE',  ( 3.796526407979370354, -93.99435622736375251, 25.82530452799085552 ) ) ;
#27403 = VERTEX_POINT ( 'NONE', #9607 ) ;
#27404 = CARTESIAN_POINT ( 'NONE',  ( 47.12009151217586833, -74.36612146640514709, -1.373451506462775029 ) ) ;
#27405 = ORIENTED_EDGE ( 'NONE', *, *, #20028, .T. ) ;
#27406 = AXIS2_PLACEMENT_3D ( 'NONE', #26816, #2489, #11188 ) ;
#27407 = CARTESIAN_POINT ( 'NONE',  ( 22.16979245059999926, -53.80651132049999319, 10.07374405240000037 ) ) ;
#27408 = CARTESIAN_POINT ( 'NONE',  ( -6.072822415560001019, -101.2995922080000071, 14.71841970630000063 ) ) ;
#27409 = ORIENTED_EDGE ( 'NONE', *, *, #28273, .F. ) ;
#27410 = CARTESIAN_POINT ( 'NONE',  ( -18.13877362739999910, -92.50000000000000000, -23.79298866759999598 ) ) ;
#27411 = CARTESIAN_POINT ( 'NONE',  ( 39.89376886939999878, -74.19145175539999570, 7.305188534010000012 ) ) ;
#27412 = CARTESIAN_POINT ( 'NONE',  ( -10.56814158951102556, -19.46927975582494952, -19.88243901464971941 ) ) ;
#27413 = CARTESIAN_POINT ( 'NONE',  ( -10.20110288159999890, -74.00000000000000000, -41.00000000000000000 ) ) ;
#27414 = LINE ( 'NONE', #4966, #26017 ) ;
#27415 = ORIENTED_EDGE ( 'NONE', *, *, #2168, .T. ) ;
#27416 = TOROIDAL_SURFACE ( 'NONE', #8327, 1.500000000000000000, 0.5000000000000000000 ) ;
#27417 = CARTESIAN_POINT ( 'NONE',  ( 12.82422588410000053, -94.98812656910000385, -19.93894973960000172 ) ) ;
#27418 = CARTESIAN_POINT ( 'NONE',  ( 18.32972815309999959, -98.73889367950000917, 3.377607424290000271 ) ) ;
#27419 = CIRCLE ( 'NONE', #2280, 55.50192378860000275 ) ;
#27420 = CARTESIAN_POINT ( 'NONE',  ( 27.24068616960000000, -92.50000000000000000, -13.71841889620000110 ) ) ;
#27421 = CARTESIAN_POINT ( 'NONE',  ( 16.52775595720000013, -99.70407914540000149, 4.748034318380000229 ) ) ;
#27422 = ORIENTED_EDGE ( 'NONE', *, *, #17008, .F. ) ;
#27423 = CIRCLE ( 'NONE', #15759, 10.00000000000000000 ) ;
#27424 = CARTESIAN_POINT ( 'NONE',  ( -38.25000000000000000, -63.30468293320000583, -1.587713240270000048 ) ) ;
#27425 = CARTESIAN_POINT ( 'NONE',  ( -38.25000000000000000, -65.14977478849999670, -2.684678751729999480 ) ) ;
#27426 = FACE_OUTER_BOUND ( 'NONE', #8294, .T. ) ;
#27427 = ORIENTED_EDGE ( 'NONE', *, *, #10277, .T. ) ;
#27428 = ADVANCED_FACE ( 'NONE', ( #18216 ), #5100, .T. ) ;
#27429 = CARTESIAN_POINT ( 'NONE',  ( -17.74180474119999573, -95.77233259950000388, 13.60688994350000058 ) ) ;
#27430 = B_SPLINE_CURVE_WITH_KNOTS ( 'NONE', 5,
 ( #11579, #18310, #8216, #17108, #23811, #5889 ),
 .UNSPECIFIED., .F., .F.,
 ( 6, 6 ),
 ( 0.000000000000000000, 1.000000000000000000 ),
 .UNSPECIFIED. ) ;
#27431 = ADVANCED_FACE ( 'NONE', ( #905 ), #28266, .T. ) ;
#27432 = CARTESIAN_POINT ( 'NONE',  ( -19.12961493519999934, -39.34784663169999419, 13.40230581219999983 ) ) ;
#27433 = CARTESIAN_POINT ( 'NONE',  ( -16.73195129730000374, -83.75000000000000000, -30.62763141000000289 ) ) ;
#27434 = CYLINDRICAL_SURFACE ( 'NONE', #15426, 5.000000000000000888 ) ;
#27435 = FACE_OUTER_BOUND ( 'NONE', #20534, .T. ) ;
#27436 = EDGE_CURVE ( 'NONE', #18033, #5395, #5195, .T. ) ;
#27437 = CARTESIAN_POINT ( 'NONE',  ( -28.07036528529999941, -39.41300778060000454, -51.38245899869999533 ) ) ;
#27438 = VECTOR ( 'NONE', #1326, 1000.000000000000000 ) ;
#27439 = CIRCLE ( 'NONE', #25584, 10.00000000000000000 ) ;
#27440 = VERTEX_POINT ( 'NONE', #6956 ) ;
#27441 = CIRCLE ( 'NONE', #24636, 6.750000000000000000 ) ;
#27442 = CARTESIAN_POINT ( 'NONE',  ( -39.30828467247898317, -73.61493928634477868, -7.216929735102859844 ) ) ;
#27443 = AXIS2_PLACEMENT_3D ( 'NONE', #14434, #23597, #27978 ) ;
#27444 = CARTESIAN_POINT ( 'NONE',  ( 19.99313163150000250, -36.00000036840000206, -9.451827061030000365 ) ) ;
#27445 = CARTESIAN_POINT ( 'NONE',  ( 10.26464537240000041, -99.91548165649999191, 14.76698580470000088 ) ) ;
#27446 = ORIENTED_EDGE ( 'NONE', *, *, #2781, .T. ) ;
#27447 = FACE_OUTER_BOUND ( 'NONE', #22039, .T. ) ;
#27448 = CARTESIAN_POINT ( 'NONE',  ( 26.77683864449999973, -23.00000000000000000, 49.01467436490000296 ) ) ;
#27449 = CARTESIAN_POINT ( 'NONE',  ( -21.43329341219999762, -64.24504445130001784, 15.59675287610000005 ) ) ;
#27450 = CARTESIAN_POINT ( 'NONE',  ( -7.963319289740001139, -100.1459902240000019, 14.96859886819999907 ) ) ;
#27451 = CARTESIAN_POINT ( 'NONE',  ( -9.284696973382905227, -94.23451058009872838, -22.99616710519532248 ) ) ;
#27452 = CARTESIAN_POINT ( 'NONE',  ( -22.29269500190000386, -94.98812477769999418, -8.065858985560000249 ) ) ;
#27453 = CARTESIAN_POINT ( 'NONE',  ( 7.593737225439999960, -101.4247867140000068, 14.04833072269999938 ) ) ;
#27454 = VERTEX_POINT ( 'NONE', #6807 ) ;
#27455 = CARTESIAN_POINT ( 'NONE',  ( -43.29999236938066076, -65.09474816373038664, 0.01998728354478918057 ) ) ;
#27456 = CARTESIAN_POINT ( 'NONE',  ( 23.15439245339999985, -19.47871561450000044, 1.365412016609999890 ) ) ;
#27457 = CARTESIAN_POINT ( 'NONE',  ( 11.57623580709999800, -97.32097376039999403, -18.02784085140000414 ) ) ;
#27458 = ORIENTED_EDGE ( 'NONE', *, *, #896, .T. ) ;
#27459 = CARTESIAN_POINT ( 'NONE',  ( -2.334489330849077504, -19.47731532786916375, -22.96368096735655939 ) ) ;
#27460 = CARTESIAN_POINT ( 'NONE',  ( 11.19714103559999963, -101.2141467319999890, -10.34781371220000068 ) ) ;
#27461 = CARTESIAN_POINT ( 'NONE',  ( -2.380747058000000305, -45.96202241429999447, -24.01241749629999944 ) ) ;
#27462 = CARTESIAN_POINT ( 'NONE',  ( -17.58052253407977616, -92.66455718075977188, 24.92338817376557714 ) ) ;
#27463 = AXIS2_PLACEMENT_3D ( 'NONE', #2569, #6931, #24849 ) ;
#27464 = AXIS2_PLACEMENT_3D ( 'NONE', #12461, #2114, #17544 ) ;
#27465 = EDGE_CURVE ( 'NONE', #16196, #134, #23161, .T. ) ;
#27466 = EDGE_CURVE ( 'NONE', #23918, #26338, #27551, .T. ) ;
#27467 = DIRECTION ( 'NONE',  ( 0.5895034617991800063, 0.000000000000000000, 0.8077658500622459936 ) ) ;
#27468 = DIRECTION ( 'NONE',  ( 0.000000000000000000, 0.000000000000000000, 1.000000000000000000 ) ) ;
#27469 = CARTESIAN_POINT ( 'NONE',  ( 21.93056824629999824, -44.91471496930000029, -8.496651354669999989 ) ) ;
#27470 = EDGE_CURVE ( 'NONE', #28564, #4268, #3725, .T. ) ;
#27471 = CARTESIAN_POINT ( 'NONE',  ( -40.35498444542948704, -74.39270540183063929, -7.250043397214241736 ) ) ;
#27472 = CARTESIAN_POINT ( 'NONE',  ( -32.77174707999999725, -82.25000000000000000, -21.60034937969999902 ) ) ;
#27473 = ORIENTED_EDGE ( 'NONE', *, *, #15189, .F. ) ;
#27474 = CARTESIAN_POINT ( 'NONE',  ( 6.796301404480000308, -101.1292389600000092, 13.93792919329999869 ) ) ;
#27475 = CARTESIAN_POINT ( 'NONE',  ( 14.02725559393949162, -98.99956644197413880, -12.21074518355317728 ) ) ;
#27476 = CARTESIAN_POINT ( 'NONE',  ( -11.34613726139999912, -94.73579816560000211, -20.70779685270000314 ) ) ;
#27477 = CARTESIAN_POINT ( 'NONE',  ( -4.085620730619999885E-15, -74.00000000000000000, 1.176836406100000135E-15 ) ) ;
#27478 = CYLINDRICAL_SURFACE ( 'NONE', #25257, 57.74999999999999289 ) ;
#27479 = CYLINDRICAL_SURFACE ( 'NONE', #14852, 1.000000000000000888 ) ;
#27480 = AXIS2_PLACEMENT_3D ( 'NONE', #5485, #18755, #22984 ) ;
#27481 = LINE ( 'NONE', #26894, #24107 ) ;
#27482 = CARTESIAN_POINT ( 'NONE',  ( -38.62788659690000515, -74.00000000000000000, 7.627568735119999666 ) ) ;
#27483 = AXIS2_PLACEMENT_3D ( 'NONE', #3802, #26523, #11035 ) ;
#27484 = AXIS2_PLACEMENT_3D ( 'NONE', #16994, #4306, #1701 ) ;
#27485 = DIRECTION ( 'NONE',  ( 0.000000000000000000, -1.000000000000000000, 0.000000000000000000 ) ) ;
#27486 = EDGE_LOOP ( 'NONE', ( #2387, #22249, #24595, #17603 ) ) ;
#27487 = CARTESIAN_POINT ( 'NONE',  ( -32.77174707999999725, -79.81706294759999309, -21.60034937969999902 ) ) ;
#27488 = CARTESIAN_POINT ( 'NONE',  ( -41.45000000000000284, -63.07912966450000880, 2.857883832489999776 ) ) ;
#27489 = ORIENTED_EDGE ( 'NONE', *, *, #3818, .T. ) ;
#27490 = CARTESIAN_POINT ( 'NONE',  ( -30.41021540318250871, -92.80045754832352145, 2.338836450776598852 ) ) ;
#27491 = CARTESIAN_POINT ( 'NONE',  ( 0.4897868758944445289, -100.0863963177148150, -17.22661518339834075 ) ) ;
#27492 = CARTESIAN_POINT ( 'NONE',  ( -11.15184145912447811, -19.46488291679582261, 19.10630597097677352 ) ) ;
#27493 = CARTESIAN_POINT ( 'NONE',  ( -7.415354059669999387, -73.99652904559999911, 39.14864742849999857 ) ) ;
#27494 = CARTESIAN_POINT ( 'NONE',  ( -11.76437930720000047, -100.8023006570000035, -10.51170590289999929 ) ) ;
#27495 = DIRECTION ( 'NONE',  ( 1.000000000000000000, 0.000000000000000000, -1.261617073437678048E-15 ) ) ;
#27496 = CARTESIAN_POINT ( 'NONE',  ( -7.242418265013072620, -74.21175622381174719, -40.33192879111471996 ) ) ;
#27497 = EDGE_CURVE ( 'NONE', #6367, #898, #26590, .T. ) ;
#27498 = EDGE_CURVE ( 'NONE', #1871, #26731, #11139, .T. ) ;
#27499 = DIRECTION ( 'NONE',  ( 0.000000000000000000, -1.000000000000000000, 0.000000000000000000 ) ) ;
#27500 = CARTESIAN_POINT ( 'NONE',  ( 13.78600462180000008, -95.55433883439999931, -17.92375705869999791 ) ) ;
#27501 = ORIENTED_EDGE ( 'NONE', *, *, #5287, .F. ) ;
#27502 = DIRECTION ( 'NONE',  ( 0.4794255386042040601, 0.000000000000000000, 0.8775825618903720926 ) ) ;
#27503 = CYLINDRICAL_SURFACE ( 'NONE', #9844, 3.749999999999996447 ) ;
#27504 = CYLINDRICAL_SURFACE ( 'NONE', #15614, 0.9999999999999991118 ) ;
#27505 = DIRECTION ( 'NONE',  ( 0.000000000000000000, -1.000000000000000000, 0.000000000000000000 ) ) ;
#27506 = AXIS2_PLACEMENT_3D ( 'NONE', #22384, #4755, #702 ) ;
#27507 = ORIENTED_EDGE ( 'NONE', *, *, #18437, .F. ) ;
#27508 = VECTOR ( 'NONE', #22154, 1000.000000000000000 ) ;
#27509 = AXIS2_PLACEMENT_3D ( 'NONE', #8923, #15042, #13441 ) ;
#27510 = EDGE_LOOP ( 'NONE', ( #28766, #1345, #5417, #9022, #8274 ) ) ;
#27511 = CARTESIAN_POINT ( 'NONE',  ( -2.352695545230000018, -57.85578495419999712, -24.35231633660000128 ) ) ;
#27512 = DIRECTION ( 'NONE',  ( 1.000000000000000000, 0.000000000000000000, 0.000000000000000000 ) ) ;
#27513 = CARTESIAN_POINT ( 'NONE',  ( 1.338287881580000116, -94.89420189149998919, 24.43791688079999957 ) ) ;
#27514 = CARTESIAN_POINT ( 'NONE',  ( 1.563038315939999867, -94.54718900769999834, 23.80456907980000025 ) ) ;
#27515 = ORIENTED_EDGE ( 'NONE', *, *, #22877, .F. ) ;
#27516 = EDGE_CURVE ( 'NONE', #10282, #19075, #19999, .T. ) ;
#27517 = VERTEX_POINT ( 'NONE', #11296 ) ;
#27518 = CARTESIAN_POINT ( 'NONE',  ( 0.000000000000000000, -65.07443093669999712, 0.000000000000000000 ) ) ;
#27519 = EDGE_CURVE ( 'NONE', #767, #25860, #1481, .T. ) ;
#27520 = CARTESIAN_POINT ( 'NONE',  ( 21.30683598400000278, -36.18102154449999830, -9.649494700380000012 ) ) ;
#27521 = CARTESIAN_POINT ( 'NONE',  ( 0.03460895995285280524, -93.66270333196790432, 25.99333972228773249 ) ) ;
#27522 = EDGE_LOOP ( 'NONE', ( #16591, #4480, #15544, #11936 ) ) ;
#27523 = AXIS2_PLACEMENT_3D ( 'NONE', #23325, #635, #27275 ) ;
#27524 = DIRECTION ( 'NONE',  ( 0.4151946956541399669, 0.5000000000001689759, 0.7600087925152558821 ) ) ;
#27525 = FACE_OUTER_BOUND ( 'NONE', #24105, .T. ) ;
#27526 = VECTOR ( 'NONE', #18479, 1000.000000000000000 ) ;
#27527 = VECTOR ( 'NONE', #14004, 1000.000000000000114 ) ;
#27528 = CARTESIAN_POINT ( 'NONE',  ( -14.58849462870000124, -79.93035050890000548, 36.50501630579999812 ) ) ;
#27529 = CARTESIAN_POINT ( 'NONE',  ( -1.469312066619999912, -66.04885972420001394, -25.55659601380000012 ) ) ;
#27530 = VECTOR ( 'NONE', #2585, 1000.000000000000000 ) ;
#27531 = ADVANCED_FACE ( 'NONE', ( #2592 ), #119, .T. ) ;
#27532 = CARTESIAN_POINT ( 'NONE',  ( 27.18988201479999844, -22.09844555429999957, 49.77074518290000071 ) ) ;
#27533 = ORIENTED_EDGE ( 'NONE', *, *, #8275, .T. ) ;
#27534 = DIRECTION ( 'NONE',  ( -0.1756244534809639490, 0.000000000000000000, -0.9844572369277969637 ) ) ;
#27535 = CARTESIAN_POINT ( 'NONE',  ( -16.50371898579999907, -100.0989745039999832, 2.846197906239999575 ) ) ;
#27536 = CARTESIAN_POINT ( 'NONE',  ( 23.40870129169999814, -59.03921360480000402, -0.5708451045399999257 ) ) ;
#27537 = CARTESIAN_POINT ( 'NONE',  ( -21.09230234119999992, -65.00127803149999295, 13.73520459809999927 ) ) ;
#27538 = ORIENTED_EDGE ( 'NONE', *, *, #7608, .T. ) ;
#27539 = DIRECTION ( 'NONE',  ( -0.4862861358100839526, 0.000000000000000000, -0.8737996304181506746 ) ) ;
#27540 = CARTESIAN_POINT ( 'NONE',  ( -7.283077424107684550, -73.99998247163075860, 39.66139668322427525 ) ) ;
#27541 = CARTESIAN_POINT ( 'NONE',  ( 36.71809979542844360, -74.32420712084812919, -14.48873512655322671 ) ) ;
#27542 = EDGE_LOOP ( 'NONE', ( #15827, #5246 ) ) ;
#27543 = DIRECTION ( 'NONE',  ( 0.000000000000000000, -1.000000000000000000, 0.000000000000000000 ) ) ;
#27544 = CARTESIAN_POINT ( 'NONE',  ( 27.18988201479999844, -16.70155444569999759, 49.77074518290000071 ) ) ;
#27545 = CARTESIAN_POINT ( 'NONE',  ( 8.468983517309998987, -34.90594137040000078, -20.83695881339999900 ) ) ;
#27546 = CARTESIAN_POINT ( 'NONE',  ( 16.42988691214025820, -100.3796496172251693, 4.355994341102395140 ) ) ;
#27547 = CARTESIAN_POINT ( 'NONE',  ( 13.81100091409999919, -99.92967571559999840, -10.51865105429999936 ) ) ;
#27548 = EDGE_LOOP ( 'NONE', ( #4172, #23218, #19262, #9026 ) ) ;
#27549 = VECTOR ( 'NONE', #4397, 1000.000000000000000 ) ;
#27550 = AXIS2_PLACEMENT_3D ( 'NONE', #10681, #6194, #12869 ) ;
#27551 = CIRCLE ( 'NONE', #2876, 1.000000000000000888 ) ;
#27552 = APPLICATION_PROTOCOL_DEFINITION ( 'draft international standard', 'automotive_design', 1998, #5873 ) ;
#27553 = CARTESIAN_POINT ( 'NONE',  ( -11.39898658829999967, -18.85531877220000041, 18.89825401980000308 ) ) ;
#27554 = CARTESIAN_POINT ( 'NONE',  ( 40.50000000000000000, -11.00000000000000000, -4.500000000000000000 ) ) ;
#27555 = CARTESIAN_POINT ( 'NONE',  ( 9.576796425482188013, -93.08693841336391017, 27.46382748655467410 ) ) ;
#27556 = ORIENTED_EDGE ( 'NONE', *, *, #1746, .F. ) ;
#27557 = CYLINDRICAL_SURFACE ( 'NONE', #2583, 0.1999999999999996780 ) ;
#27558 = ORIENTED_EDGE ( 'NONE', *, *, #4749, .T. ) ;
#27559 = CARTESIAN_POINT ( 'NONE',  ( -11.33386635579999790, -27.06678469999999948, 19.29914645179999866 ) ) ;
#27560 = CARTESIAN_POINT ( 'NONE',  ( 8.289122765224647083, -18.50000007361606436, -18.87681024063931545 ) ) ;
#27561 = EDGE_LOOP ( 'NONE', ( #3195, #13262, #8732, #16478 ) ) ;
#27562 = EDGE_CURVE ( 'NONE', #25484, #22871, #9780, .T. ) ;
#27563 = CARTESIAN_POINT ( 'NONE',  ( -37.15721607020263662, -63.17171877515593792, -0.3794438750330945687 ) ) ;
#27564 = CARTESIAN_POINT ( 'NONE',  ( -40.00000000000000000, -69.00000000000000000, 0.000000000000000000 ) ) ;
#27565 = EDGE_CURVE ( 'NONE', #7740, #26971, #22426, .T. ) ;
#27566 = TOROIDAL_SURFACE ( 'NONE', #25299, 3.750000000000000000, 1.000000000000000000 ) ;
#27567 = AXIS2_PLACEMENT_3D ( 'NONE', #15170, #6305, #17244 ) ;
#27568 = CYLINDRICAL_SURFACE ( 'NONE', #25564, 32.39999999999999147 ) ;
#27569 = CARTESIAN_POINT ( 'NONE',  ( -10.55455086157921940, -19.48670042615375309, -21.19291729735819274 ) ) ;
#27570 = CARTESIAN_POINT ( 'NONE',  ( -13.07115940794487052, -101.6174239712916716, -9.267504955542015921 ) ) ;
#27571 = ADVANCED_FACE ( 'NONE', ( #20654 ), #6034, .F. ) ;
#27572 = CARTESIAN_POINT ( 'NONE',  ( 7.358959778060000012, -101.1389411659999951, 13.51882459459999986 ) ) ;
#27573 = VECTOR ( 'NONE', #28536, 1000.000000000000000 ) ;
#27574 = CARTESIAN_POINT ( 'NONE',  ( 47.05374491310924157, -79.59514489290765482, -2.116163992179171949 ) ) ;
#27575 = ORIENTED_EDGE ( 'NONE', *, *, #27358, .T. ) ;
#27576 = ADVANCED_FACE ( 'NONE', ( #11739 ), #12898, .T. ) ;
#27577 = CARTESIAN_POINT ( 'NONE',  ( -32.67527180340000825, -79.69119431650000251, -22.00249031550000112 ) ) ;
#27578 = LINE ( 'NONE', #9909, #24231 ) ;
#27579 = B_SPLINE_CURVE_WITH_KNOTS ( 'NONE', 3,
 ( #5871, #10502, #3834, #12835, #14751, #23654 ),
 .UNSPECIFIED., .F., .F.,
 ( 4, 2, 4 ),
 ( 0.000000000000000000, 0.5000000000000000000, 1.000000000000000000 ),
 .UNSPECIFIED. ) ;
#27580 = ORIENTED_EDGE ( 'NONE', *, *, #1987, .T. ) ;
#27581 = CARTESIAN_POINT ( 'NONE',  ( 29.71814534510813033, -92.87422005961060734, 6.861636527948729025 ) ) ;
#27582 = CARTESIAN_POINT ( 'NONE',  ( 32.39999999999999858, -82.50000000000000000, 3.967724586379999025E-15 ) ) ;
#27583 = ORIENTED_EDGE ( 'NONE', *, *, #4603, .F. ) ;
#27584 = DIRECTION ( 'NONE',  ( 0.4794255386042040046, 0.000000000000000000, 0.8775825618903722036 ) ) ;
#27585 = CARTESIAN_POINT ( 'NONE',  ( -18.70529629369999824, -26.09793778670000108, 12.22846835330000026 ) ) ;
#27586 = CARTESIAN_POINT ( 'NONE',  ( 40.70731707320000226, -82.25000000000000000, -7.215414233289999757 ) ) ;
#27587 = DIRECTION ( 'NONE',  ( 0.000000000000000000, -1.000000000000000000, 0.000000000000000000 ) ) ;
#27588 = CARTESIAN_POINT ( 'NONE',  ( 22.31839213210000139, -59.04258408700000160, -7.084352054500000051 ) ) ;
#27589 = CARTESIAN_POINT ( 'NONE',  ( 0.000000000000000000, 0.000000000000000000, 0.000000000000000000 ) ) ;
#27590 = CARTESIAN_POINT ( 'NONE',  ( -10.85441475189999849, -19.15747270589999829, 19.16405033270000047 ) ) ;
#27591 = AXIS2_PLACEMENT_3D ( 'NONE', #18139, #13614, #15940 ) ;
#27592 = ORIENTED_EDGE ( 'NONE', *, *, #25646, .F. ) ;
#27593 = CARTESIAN_POINT ( 'NONE',  ( 8.797620038699999867, -37.04760834070000186, -21.76996719339999942 ) ) ;
#27594 = FACE_BOUND ( 'NONE', #20110, .T. ) ;
#27595 = CARTESIAN_POINT ( 'NONE',  ( 21.27769661889999853, -36.50665358839999897, -8.736999621189999843 ) ) ;
#27596 = DIRECTION ( 'NONE',  ( 1.000000000000000000, 0.000000000000000000, 0.000000000000000000 ) ) ;
#27597 = EDGE_LOOP ( 'NONE', ( #2599, #17476 ) ) ;
#27598 = CYLINDRICAL_SURFACE ( 'NONE', #6458, 5.000000000000002665 ) ;
#27599 = CARTESIAN_POINT ( 'NONE',  ( -13.46646172799999874, -101.3150705500000157, -9.098097921289998169 ) ) ;
#27600 = EDGE_CURVE ( 'NONE', #6516, #418, #21086, .T. ) ;
#27601 = B_SPLINE_SURFACE_WITH_KNOTS ( 'NONE', 5, 5, ( 
 ( #16482, #1071, #9911, #12368, #25929, #6650, #15662, #17870, #21556 ),
 ( #15513, #16906, #4460, #10449, #3642, #19368, #20047, #26066, #25797 ),
 ( #26769, #8016, #5953, #8279, #6801, #2139, #17725, #8152, #13328 ),
 ( #22233, #6095, #19890, #5825, #14836, #23739, #24564, #2283, #21276 ),
 ( #26609, #1332, #23884, #3782, #24422, #28774, #11130, #10175, #19093 ),
 ( #112, #8962, #27979, #14707, #23598, #12504, #12643, #21415, #1473 ),
 ( #17039, #10314, #19227, #28115, #1611, #28243, #17179, #14972, #3920 ),
 ( #12785, #21693, #22979, #3029, #11882, #848, #16105, #22680, #25005 ),
 ( #22542, #22387, #27053, #20196, #13930, #18311, #15811, #11289, #406 ) ),
 .UNSPECIFIED., .F., .F., .F.,
 ( 6, 3, 6 ),
 ( 6, 3, 6 ),
 ( 7.186332009700000079, 18.82032539240000091, 25.08217527269999891 ),
 ( 0.000000000000000000, 0.2500000000000000000, 0.5000000000000000000 ),
 .UNSPECIFIED. ) ;
#27602 = CARTESIAN_POINT ( 'NONE',  ( 47.11548663039999951, -79.82827424500000291, -1.752954514250000040 ) ) ;
#27603 = CARTESIAN_POINT ( 'NONE',  ( 9.175396146610001580, -40.70401306919999485, -22.46104921330000082 ) ) ;
#27604 = CARTESIAN_POINT ( 'NONE',  ( 7.604558782770000747, -101.6481558220000068, 14.07757856980000000 ) ) ;
#27605 = EDGE_LOOP ( 'NONE', ( #9076, #128, #16710, #1454 ) ) ;
#27606 = ADVANCED_FACE ( 'NONE', ( #9410 ), #27503, .F. ) ;
#27607 = CARTESIAN_POINT ( 'NONE',  ( -40.35276762241279869, -74.22736093640011745, 7.241427273148282495 ) ) ;
#27608 = CARTESIAN_POINT ( 'NONE',  ( -9.249130345009998422, -111.0000000000000000, -19.10987009810000004 ) ) ;
#27609 = CARTESIAN_POINT ( 'NONE',  ( 11.23915487290000037, -100.8869813350000015, -10.91500521270000057 ) ) ;
#27610 = EDGE_LOOP ( 'NONE', ( #13702, #27427, #20973, #2543 ) ) ;
#27611 = CARTESIAN_POINT ( 'NONE',  ( 19.07516306020000130, -18.50000000000000000, -8.007516059049999413 ) ) ;
#27612 = CIRCLE ( 'NONE', #18760, 0.3500000000000003664 ) ;
#27613 = CARTESIAN_POINT ( 'NONE',  ( 0.000000000000000000, -10.50000000000000000, 0.000000000000000000 ) ) ;
#27614 = AXIS2_PLACEMENT_3D ( 'NONE', #21404, #26208, #28233 ) ;
#27615 = CARTESIAN_POINT ( 'NONE',  ( -2.582078993590000149, -32.66150190429999611, -24.62446518169999976 ) ) ;
#27616 = CARTESIAN_POINT ( 'NONE',  ( 14.28941763439999946, -93.00000000000000000, -3.575252188409999921 ) ) ;
#27617 = CARTESIAN_POINT ( 'NONE',  ( -37.75000000000000000, -65.63577453799999262, 0.7216878364859999895 ) ) ;
#27618 = DIRECTION ( 'NONE',  ( 1.000000000000000000, 0.000000000000000000, 0.000000000000000000 ) ) ;
#27619 = CARTESIAN_POINT ( 'NONE',  ( 22.93608650079999833, -36.50000000029999825, -9.381593461610000517 ) ) ;
#27620 = CARTESIAN_POINT ( 'NONE',  ( -39.31221710997630936, -74.09469053470054689, -7.479534728624519957 ) ) ;
#27621 = FACE_OUTER_BOUND ( 'NONE', #27191, .T. ) ;
#27622 = ORIENTED_EDGE ( 'NONE', *, *, #25799, .F. ) ;
#27623 = CARTESIAN_POINT ( 'NONE',  ( 7.102042752109999135, -101.5369810359999860, 14.33739825589999839 ) ) ;
#27624 = CARTESIAN_POINT ( 'NONE',  ( 47.16974535660000356, -74.50000000000000000, -1.075756255579999987 ) ) ;
#27625 = CIRCLE ( 'NONE', #14995, 57.75000000000000000 ) ;
#27626 = CARTESIAN_POINT ( 'NONE',  ( -11.16211105210000021, -94.83053003919999924, -21.09958095109999832 ) ) ;
#27627 = CARTESIAN_POINT ( 'NONE',  ( 8.396977894420000865, -36.03998444319999805, -21.19011196440000333 ) ) ;
#27628 = DIRECTION ( 'NONE',  ( 0.000000000000000000, -1.000000000000000000, 0.000000000000000000 ) ) ;
#27629 = B_SPLINE_CURVE_WITH_KNOTS ( 'NONE', 3,
 ( #15374, #20467, #8676, #18288, #535, #6222, #5019, #17588, #13908, #26477, #17299, #15936, #27178, #12894, #26191, #22810, #24287, #4329, #15087, #2848, #22111 ),
 .UNSPECIFIED., .F., .F.,
 ( 4, 2, 2, 1, 2, 2, 2, 2, 2, 2, 4 ),
 ( 0.000000000000000000, 0.2499999999999882316, 0.3749999999999823475, 0.4374999999999761302, 0.4687499999999980016, 0.5000000000000199840, 0.6250000000000873746, 0.6875000000000981437, 0.7187500000000924816, 0.7500000000000868194, 1.000000000000000000 ),
 .UNSPECIFIED. ) ;
#27630 = CARTESIAN_POINT ( 'NONE',  ( 23.58466923419999972, -94.98812477769999418, -2.405350023570000051 ) ) ;
#27631 = TOROIDAL_SURFACE ( 'NONE', #15470, 3.750000000000000000, 1.000000000000000000 ) ;
#27632 = CARTESIAN_POINT ( 'NONE',  ( -23.49132717730000053, -93.00000000000000000, -19.26887671769999955 ) ) ;
#27633 = EDGE_CURVE ( 'NONE', #14582, #6516, #14030, .T. ) ;
#27634 = SURFACE_SIDE_STYLE ('',( #14066 ) ) ;
#27635 = ORIENTED_EDGE ( 'NONE', *, *, #3856, .T. ) ;
#27636 = CARTESIAN_POINT ( 'NONE',  ( -32.77174707999999725, -79.50000000000000000, -21.60034937969999902 ) ) ;
#27637 = EDGE_CURVE ( 'NONE', #10282, #1710, #18703, .T. ) ;
#27638 = CARTESIAN_POINT ( 'NONE',  ( -12.89904789370000060, -65.07443093669999712, -21.58991903219999742 ) ) ;
#27639 = ORIENTED_EDGE ( 'NONE', *, *, #21386, .T. ) ;
#27640 = FACE_OUTER_BOUND ( 'NONE', #10150, .T. ) ;
#27641 = CARTESIAN_POINT ( 'NONE',  ( 6.962669195700001090, -93.00000450890000536, -28.64060852350000275 ) ) ;
#27642 = CARTESIAN_POINT ( 'NONE',  ( -7.310176754529999599, -73.98157068460000119, 39.44185033859999834 ) ) ;
#27643 = AXIS2_PLACEMENT_3D ( 'NONE', #15774, #20454, #26870 ) ;
#27644 = FACE_OUTER_BOUND ( 'NONE', #7401, .T. ) ;
#27645 = DIRECTION ( 'NONE',  ( 0.000000000000000000, 1.000000000000000000, 0.000000000000000000 ) ) ;
#27646 = CARTESIAN_POINT ( 'NONE',  ( 26.61374759190000105, -73.81001964159999318, -28.89513312169999892 ) ) ;
#27647 = CARTESIAN_POINT ( 'NONE',  ( 0.3872056760429999911, -111.0000000000000000, -17.35614698070000017 ) ) ;
#27648 = CARTESIAN_POINT ( 'NONE',  ( 13.49546580460000023, -95.85308664759999431, -18.00277386639999833 ) ) ;
#27649 = DIRECTION ( 'NONE',  ( 0.000000000000000000, -1.000000000000000000, 0.000000000000000000 ) ) ;
#27650 = DIRECTION ( 'NONE',  ( 0.1516076670439319707, -0.9486832980505756074, 0.2775159730418759185 ) ) ;
#27651 = CARTESIAN_POINT ( 'NONE',  ( -40.00000000000000000, -65.00000000000000000, -3.175426480540000096 ) ) ;
#27652 = AXIS2_PLACEMENT_3D ( 'NONE', #16944, #17072, #10624 ) ;
#27653 = CARTESIAN_POINT ( 'NONE',  ( -41.74999999999177902, -63.07121106306900771, 2.719955530729126991 ) ) ;
#27654 = ORIENTED_EDGE ( 'NONE', *, *, #8825, .T. ) ;
#27655 = CARTESIAN_POINT ( 'NONE',  ( 9.444187806723459033, -35.99901531098080909, -19.97576011151723563 ) ) ;
#27656 = EDGE_CURVE ( 'NONE', #5033, #10479, #4656, .T. ) ;
#27657 = ORIENTED_EDGE ( 'NONE', *, *, #25539, .F. ) ;
#27658 = CIRCLE ( 'NONE', #26702, 39.25000000000000000 ) ;
#27659 = DIRECTION ( 'NONE',  ( 0.4794255386042041711, 0.000000000000000000, 0.8775825618903722036 ) ) ;
#27660 = AXIS2_PLACEMENT_3D ( 'NONE', #3442, #3994, #1269 ) ;
#27661 = CARTESIAN_POINT ( 'NONE',  ( 11.31764183700000004, -36.00000000000000000, -22.43277176020000141 ) ) ;
#27662 = CARTESIAN_POINT ( 'NONE',  ( -5.121557230439998776, -99.75094652300001030, 17.11281665599999968 ) ) ;
#27663 = CARTESIAN_POINT ( 'NONE',  ( -0.7205257401540000606, -101.6484611540000031, -15.98376809950000066 ) ) ;
#27664 = ORIENTED_EDGE ( 'NONE', *, *, #12445, .F. ) ;
#27665 = EDGE_CURVE ( 'NONE', #1691, #4525, #25012, .T. ) ;
#27666 = EDGE_CURVE ( 'NONE', #7650, #16368, #12105, .T. ) ;
#27667 = CARTESIAN_POINT ( 'NONE',  ( -11.31667057079999950, -95.23931402160000914, -21.36056405359999744 ) ) ;
#27668 = CARTESIAN_POINT ( 'NONE',  ( -7.135467692470220946, -73.63090023098223469, 38.71641001238775459 ) ) ;
#27669 = CYLINDRICAL_SURFACE ( 'NONE', #21013, 4.750000000000001776 ) ;
#27670 = VERTEX_POINT ( 'NONE', #10391 ) ;
#27671 = CARTESIAN_POINT ( 'NONE',  ( 15.53338745080000116, -84.25000000000000000, 28.43367500519999780 ) ) ;
#27672 = DIRECTION ( 'NONE',  ( 0.000000000000000000, 1.000000000000000000, 0.000000000000000000 ) ) ;
#27673 = CARTESIAN_POINT ( 'NONE',  ( 26.73327912300000264, -92.84292488370000740, -12.41348515490000182 ) ) ;
#27674 = CARTESIAN_POINT ( 'NONE',  ( 23.70295537799999863, -94.59276292389999696, -2.111841813949999924 ) ) ;
#27675 = CARTESIAN_POINT ( 'NONE',  ( -36.59277592640000165, -74.50000000000000000, -25.98617420859999783 ) ) ;
#27676 = ORIENTED_EDGE ( 'NONE', *, *, #20883, .F. ) ;
#27677 = CARTESIAN_POINT ( 'NONE',  ( 36.49700125519999716, -74.06833701100001122, -14.20639533249999964 ) ) ;
#27678 = CARTESIAN_POINT ( 'NONE',  ( -15.66925473879999764, -101.4673694920000031, 3.460543690009999729 ) ) ;
#27679 = CARTESIAN_POINT ( 'NONE',  ( -5.969238273050000210, -101.2530993000000024, 13.97222956270000083 ) ) ;
#27680 = ORIENTED_EDGE ( 'NONE', *, *, #22748, .T. ) ;
#27681 = AXIS2_PLACEMENT_3D ( 'NONE', #15509, #4456, #26764 ) ;
#27682 = DIRECTION ( 'NONE',  ( 0.000000000000000000, 1.000000000000000000, 0.000000000000000000 ) ) ;
#27683 = CARTESIAN_POINT ( 'NONE',  ( -7.250391496897478305, -74.00000000000000000, 39.93225832964911604 ) ) ;
#27684 = CARTESIAN_POINT ( 'NONE',  ( 36.61782233228550609, -74.16892777906130618, -14.30620871315702658 ) ) ;
#27685 = ORIENTED_EDGE ( 'NONE', *, *, #3847, .T. ) ;
#27686 = ADVANCED_FACE ( 'NONE', ( #8090 ), #11684, .F. ) ;
#27687 = CARTESIAN_POINT ( 'NONE',  ( 0.000000000000000000, -30.20000000000000284, 0.000000000000000000 ) ) ;
#27688 = CARTESIAN_POINT ( 'NONE',  ( -31.99304886599999875, -74.00000000020000357, -21.98470665500000010 ) ) ;
#27689 = DIRECTION ( 'NONE',  ( 0.000000000000000000, 1.000000000000000000, 0.000000000000000000 ) ) ;
#27690 = CARTESIAN_POINT ( 'NONE',  ( 0.000000000000000000, -18.50000000000000000, 0.000000000000000000 ) ) ;
#27691 = ORIENTED_EDGE ( 'NONE', *, *, #17570, .T. ) ;
#27692 = VECTOR ( 'NONE', #16260, 1000.000000000000114 ) ;
#27693 = AXIS2_PLACEMENT_3D ( 'NONE', #3975, #17233, #8072 ) ;
#27694 = EDGE_CURVE ( 'NONE', #17770, #26105, #25586, .T. ) ;
#27695 = CARTESIAN_POINT ( 'NONE',  ( 6.584707521381107931, -93.38816055823026829, 26.86884258581816454 ) ) ;
#27696 = EDGE_LOOP ( 'NONE', ( #2276, #6857, #20398, #16321 ) ) ;
#27697 = CARTESIAN_POINT ( 'NONE',  ( 47.16888291020000423, -74.56821585100000505, -1.104556675960000067 ) ) ;
#27698 = ORIENTED_EDGE ( 'NONE', *, *, #6345, .T. ) ;
#27699 = AXIS2_PLACEMENT_3D ( 'NONE', #12543, #14876, #5862 ) ;
#27700 = CARTESIAN_POINT ( 'NONE',  ( -11.25709297429999900, -19.46485661140000190, 19.04110009109999879 ) ) ;
#27701 = CARTESIAN_POINT ( 'NONE',  ( -5.750261582500000301, -100.9405348700000076, 14.87178911969999895 ) ) ;
#27702 = EDGE_LOOP ( 'NONE', ( #23572, #23720, #8808, #13774 ) ) ;
#27703 = CARTESIAN_POINT ( 'NONE',  ( 45.84677420572959505, -80.34292036800317760, -4.286925633470588082 ) ) ;
#27704 = CARTESIAN_POINT ( 'NONE',  ( 40.28438195609999894, -74.37144044050000957, 7.256982118289999839 ) ) ;
#27705 = CARTESIAN_POINT ( 'NONE',  ( -10.51051889136755513, -19.48405220144317695, -21.03322345498822443 ) ) ;
#27706 = CARTESIAN_POINT ( 'NONE',  ( 25.53957162523754576, -69.04156329992152052, -8.628252605428819777 ) ) ;
#27707 = CARTESIAN_POINT ( 'NONE',  ( -11.67416330133831437, -61.62341122741943877, -23.03586770298056052 ) ) ;
#27708 = CARTESIAN_POINT ( 'NONE',  ( -29.76178938840000043, -93.00000000000000000, 6.669774538800000485 ) ) ;
#27709 = VERTEX_POINT ( 'NONE', #7952 ) ;
#27710 = CARTESIAN_POINT ( 'NONE',  ( -6.322973885729999743, -74.00000000000000000, 35.51864961870000315 ) ) ;
#27711 = CARTESIAN_POINT ( 'NONE',  ( 8.508194237257523440, -34.61672934516087707, -20.76917592404496204 ) ) ;
#27712 = FACE_OUTER_BOUND ( 'NONE', #509, .T. ) ;
#27713 = CARTESIAN_POINT ( 'NONE',  ( 0.000000000000000000, -33.79999999999999716, 0.000000000000000000 ) ) ;
#27714 = ORIENTED_EDGE ( 'NONE', *, *, #14200, .T. ) ;
#27715 = CARTESIAN_POINT ( 'NONE',  ( -2.874157831770000282, -80.49856749429999070, 46.70286942899999616 ) ) ;
#27716 = CARTESIAN_POINT ( 'NONE',  ( -41.54999999999999716, -65.00000000000000000, 2.684678751729999480 ) ) ;
#27717 = ORIENTED_EDGE ( 'NONE', *, *, #11030, .T. ) ;
#27718 = CYLINDRICAL_SURFACE ( 'NONE', #3450, 10.99999999999999822 ) ;
#27719 = CONICAL_SURFACE ( 'NONE', #16471, 52.86371681419998936, 1.437659999240000097 ) ;
#27720 = DIRECTION ( 'NONE',  ( 0.000000000000000000, 1.000000000000000000, 0.000000000000000000 ) ) ;
#27721 = FACE_OUTER_BOUND ( 'NONE', #22158, .T. ) ;
#27722 = CARTESIAN_POINT ( 'NONE',  ( -38.17164989577617007, -65.73761215452408635, 1.198860239814103057 ) ) ;
#27723 = DIRECTION ( 'NONE',  ( 1.000000000000000000, 0.000000000000000000, 0.000000000000000000 ) ) ;
#27724 = ADVANCED_FACE ( 'NONE', ( #17409 ), #15184, .T. ) ;
#27725 = ADVANCED_FACE ( 'NONE', ( #10254 ), #19437, .T. ) ;
#27726 = EDGE_CURVE ( 'NONE', #623, #21436, #6917, .T. ) ;
#27727 = VERTEX_POINT ( 'NONE', #13455 ) ;
#27728 = CARTESIAN_POINT ( 'NONE',  ( 20.43617771219999923, -55.54030921969999923, 11.17804412479999954 ) ) ;
#27729 = FACE_OUTER_BOUND ( 'NONE', #13056, .T. ) ;
#27730 = AXIS2_PLACEMENT_3D ( 'NONE', #13399, #13550, #26680 ) ;
#27731 = CARTESIAN_POINT ( 'NONE',  ( 6.962684791734604417, -92.86910576386146943, -28.64059324402698081 ) ) ;
#27732 = EDGE_LOOP ( 'NONE', ( #190, #25308, #1757, #14358 ) ) ;
#27733 = CARTESIAN_POINT ( 'NONE',  ( 8.028473304129999377, -18.50000000000000000, -18.85230009969999898 ) ) ;
#27734 = DIRECTION ( 'NONE',  ( -0.000000000000000000, 1.000000000000000000, 0.000000000000000000 ) ) ;
#27735 = SURFACE_STYLE_USAGE ( .BOTH. , #5148 ) ;
#27736 = CARTESIAN_POINT ( 'NONE',  ( 9.449797638950000689, -44.86350384200000008, -23.17371582650000050 ) ) ;
#27737 = CARTESIAN_POINT ( 'NONE',  ( 7.584268299279999681, -101.5369811529999993, 14.08825296820000084 ) ) ;
#27738 = ORIENTED_EDGE ( 'NONE', *, *, #7421, .F. ) ;
#27739 = CARTESIAN_POINT ( 'NONE',  ( -39.65872146214135796, -73.77182148721053068, 7.242474372565215646 ) ) ;
#27740 = CARTESIAN_POINT ( 'NONE',  ( 23.69918219720000252, -19.41822431039999941, 1.513728844550000119 ) ) ;
#27741 = CARTESIAN_POINT ( 'NONE',  ( 11.43994181019999878, -100.8816831189999874, -10.88980295719999880 ) ) ;
#27742 = ORIENTED_EDGE ( 'NONE', *, *, #12736, .F. ) ;
#27743 = DIRECTION ( 'NONE',  ( 0.000000000000000000, -1.000000000000000000, 0.000000000000000000 ) ) ;
#27744 = DIRECTION ( 'NONE',  ( -0.3687499999999825917, 0.000000000000000000, 0.9295286103719523352 ) ) ;
#27745 = CARTESIAN_POINT ( 'NONE',  ( -0.5567039383430000266, -26.09744228910000174, -22.25837505089999979 ) ) ;
#27746 = FACE_OUTER_BOUND ( 'NONE', #19629, .T. ) ;
#27747 = CARTESIAN_POINT ( 'NONE',  ( -0.3035179129464828374, -74.42029229106765342, 47.25000000000000000 ) ) ;
#27748 = CARTESIAN_POINT ( 'NONE',  ( 11.86685847370859470, -101.5019029711483682, -10.89638159996464850 ) ) ;
#27749 = CARTESIAN_POINT ( 'NONE',  ( 22.33517371069999768, -36.52243084719999899, -9.146761579799999708 ) ) ;
#27750 = DIRECTION ( 'NONE',  ( 0.000000000000000000, -1.000000000000000000, 0.000000000000000000 ) ) ;
#27751 = CARTESIAN_POINT ( 'NONE',  ( -37.28811165380000148, -65.41419836839999391, 0.4550164754539999801 ) ) ;
#27752 = ORIENTED_EDGE ( 'NONE', *, *, #7012, .T. ) ;
#27753 = EDGE_CURVE ( 'NONE', #5069, #4593, #13754, .T. ) ;
#27754 = CARTESIAN_POINT ( 'NONE',  ( 7.102042752109999135, -101.6484611540000031, 14.33739825589999839 ) ) ;
#27755 = CARTESIAN_POINT ( 'NONE',  ( -4.556355293060001005E-12, -111.0000000000000000, 3.907985046680000915E-12 ) ) ;
#27756 = CARTESIAN_POINT ( 'NONE',  ( 7.629218925470000023, -101.5342894280000081, 14.06592359269999903 ) ) ;
#27757 = VECTOR ( 'NONE', #643, 1000.000000000000000 ) ;
#27758 = ADVANCED_FACE ( 'NONE', ( #83 ), #22886, .F. ) ;
#27759 = CARTESIAN_POINT ( 'NONE',  ( -11.21692420940000012, -94.79902974079999467, -20.68495762359999901 ) ) ;
#27760 = CARTESIAN_POINT ( 'NONE',  ( 20.87697854030000144, -35.04923858010000970, -8.448077735809999211 ) ) ;
#27761 = DIRECTION ( 'NONE',  ( -0.2287893768880245315, 0.000000000000000000, 0.9734759478401042720 ) ) ;
#27762 = CARTESIAN_POINT ( 'NONE',  ( 0.000000000000000000, -92.50000000000000000, 0.000000000000000000 ) ) ;
#27763 = CYLINDRICAL_SURFACE ( 'NONE', #14211, 1.000000000000000000 ) ;
#27764 =( NAMED_UNIT ( * ) PLANE_ANGLE_UNIT ( ) SI_UNIT ( $, .RADIAN. ) );
#27765 = ORIENTED_EDGE ( 'NONE', *, *, #14353, .F. ) ;
#27766 = CARTESIAN_POINT ( 'NONE',  ( 32.43349014520016027, -74.01270418637506054, -21.45979546804144178 ) ) ;
#27767 = CARTESIAN_POINT ( 'NONE',  ( 18.94592261899999741, -19.50000000000000000, -9.024080787800000891 ) ) ;
#27768 = ORIENTED_EDGE ( 'NONE', *, *, #26886, .F. ) ;
#27769 = CARTESIAN_POINT ( 'NONE',  ( -25.98617420859999783, -77.00000000000000000, -36.59277592640000165 ) ) ;
#27770 = CARTESIAN_POINT ( 'NONE',  ( 0.5962742269612683055, -100.4103893717004325, -16.96241722493727622 ) ) ;
#27771 = CARTESIAN_POINT ( 'NONE',  ( -7.319780978429999863, -73.91748504689999777, 39.18460075750000016 ) ) ;
#27772 = CARTESIAN_POINT ( 'NONE',  ( 13.19836993693740901, -92.83160374581309782, 27.49641872786132168 ) ) ;
#27773 = CARTESIAN_POINT ( 'NONE',  ( -13.26856174610000139, -93.91547326100000248, -20.89962974999999901 ) ) ;
#27774 = CARTESIAN_POINT ( 'NONE',  ( 20.36016146999999776, -74.00000000000000000, -32.97008227039999895 ) ) ;
#27775 = DIRECTION ( 'NONE',  ( 0.4794255386042000078, 0.000000000000000000, 0.8775825618903743131 ) ) ;
#27776 = CARTESIAN_POINT ( 'NONE',  ( -12.17175180279999935, -57.47855601759999900, -19.93971687999999887 ) ) ;
#27777 = DIRECTION ( 'NONE',  ( 1.000000000000000000, 0.000000000000000000, 0.000000000000000000 ) ) ;
#27778 = CARTESIAN_POINT ( 'NONE',  ( 8.976488324580000011, -22.51608882080000029, -19.49531134190000259 ) ) ;
#27779 = DIRECTION ( 'NONE',  ( 0.000000000000000000, -1.000000000000000000, 0.000000000000000000 ) ) ;
#27780 = EDGE_LOOP ( 'NONE', ( #1638, #21617, #10068, #17160, #26717, #25402 ) ) ;
#27781 = EDGE_CURVE ( 'NONE', #20206, #12333, #10817, .T. ) ;
#27782 = DIRECTION ( 'NONE',  ( 0.000000000000000000, 1.000000000000000000, 0.000000000000000000 ) ) ;
#27783 = ORIENTED_EDGE ( 'NONE', *, *, #25419, .T. ) ;
#27784 = EDGE_CURVE ( 'NONE', #20968, #26598, #28713, .T. ) ;
#27785 = ADVANCED_FACE ( 'NONE', ( #20307 ), #13847, .T. ) ;
#27786 = LINE ( 'NONE', #12178, #21614 ) ;
#27787 = DIRECTION ( 'NONE',  ( 0.4794255386042000078, 0.000000000000000000, 0.8775825618903743131 ) ) ;
#27788 = CARTESIAN_POINT ( 'NONE',  ( -0.7116806507476617361, -101.2404586421512960, -15.78755322732534516 ) ) ;
#27789 = CARTESIAN_POINT ( 'NONE',  ( -20.45998242170000125, -52.56313962710000709, 14.78974999389999923 ) ) ;
#27790 = CARTESIAN_POINT ( 'NONE',  ( 50.00000000000000000, -15.00000000000000000, -4.500000000000000000 ) ) ;
#27791 = LINE ( 'NONE', #7832, #18100 ) ;
#27792 = EDGE_LOOP ( 'NONE', ( #12490, #12293, #9196, #19602, #4255, #18668 ) ) ;
#27793 = CARTESIAN_POINT ( 'NONE',  ( -37.60355029590000697, -84.00000000000000000, 9.356041104380000917 ) ) ;
#27794 = CARTESIAN_POINT ( 'NONE',  ( 7.707964880030000465, -36.74561153859999507, -21.48083100459999883 ) ) ;
#27795 = CARTESIAN_POINT ( 'NONE',  ( 25.51708727519999798, -93.49005502320000005, -5.885575441059999413 ) ) ;
#27796 = CARTESIAN_POINT ( 'NONE',  ( -15.31688208200000112, -69.70331854509998948, 22.99240601979999710 ) ) ;
#27797 = EDGE_LOOP ( 'NONE', ( #16020, #13051, #12992, #19354 ) ) ;
#27798 = CARTESIAN_POINT ( 'NONE',  ( 46.25000000000000000, -75.00000000000000000, -13.75000000000000000 ) ) ;
#27799 = AXIS2_PLACEMENT_3D ( 'NONE', #10798, #15033, #23948 ) ;
#27800 = CARTESIAN_POINT ( 'NONE',  ( -16.61164113330000092, -100.3817456209999932, 3.144183042669999928 ) ) ;
#27801 = CARTESIAN_POINT ( 'NONE',  ( 23.62253742169999882, -60.59277760239999822, -0.2692575271260000402 ) ) ;
#27802 = DIRECTION ( 'NONE',  ( 1.000000000000000000, 0.000000000000000000, 0.000000000000000000 ) ) ;
#27803 = ORIENTED_EDGE ( 'NONE', *, *, #4198, .T. ) ;
#27804 = FACE_OUTER_BOUND ( 'NONE', #16349, .T. ) ;
#27805 = CARTESIAN_POINT ( 'NONE',  ( 18.93437244977972611, -18.87168146926155643, -8.901252598746989264 ) ) ;
#27806 = PLANE ( 'NONE',  #4750 ) ;
#27807 = ORIENTED_EDGE ( 'NONE', *, *, #24306, .F. ) ;
#27808 = ADVANCED_FACE ( 'NONE', ( #13163 ), #13010, .T. ) ;
#27809 = CARTESIAN_POINT ( 'NONE',  ( -41.71910660533971082, -65.10668761693263207, -2.792605221528440929 ) ) ;
#27810 = CIRCLE ( 'NONE', #23616, 1.250000000000000000 ) ;
#27811 = CARTESIAN_POINT ( 'NONE',  ( -41.81387021366961676, -65.73322674265565979, -1.234409484187863892 ) ) ;
#27812 = CARTESIAN_POINT ( 'NONE',  ( 7.318372426699999878, -73.93831497249999529, 38.68350751799999898 ) ) ;
#27813 = CARTESIAN_POINT ( 'NONE',  ( 31.00000000000000000, -11.00000000000000000, -4.500000000000000000 ) ) ;
#27814 = VERTEX_POINT ( 'NONE', #22513 ) ;
#27815 = PRODUCT_DEFINITION_CONTEXT ( 'detailed design', #23920, 'design' ) ;
#27816 = B_SPLINE_SURFACE_WITH_KNOTS ( 'NONE', 5, 5, ( 
 ( #10633, #6589, #19547, #15451, #19977, #15015 ),
 ( #17371, #22036, #13270, #50, #26115, #10494 ),
 ( #3967, #28579, #2219, #28435, #8895, #12689 ),
 ( #19409, #17809, #19689, #8613, #14879, #23787 ),
 ( #28290, #6142, #23929, #17515, #2084, #26401 ),
 ( #6431, #19830, #17954, #4845, #5134, #11519 ) ),
 .UNSPECIFIED., .F., .F., .F.,
 ( 6, 6 ),
 ( 6, 6 ),
 ( 13.75601705980000133, 16.62037739340000186 ),
 ( 0.000000000000000000, 2.000000000000000000 ),
 .UNSPECIFIED. ) ;
#27817 = CARTESIAN_POINT ( 'NONE',  ( 36.92830089767138446, -79.76883227166896972, -14.38962487061029272 ) ) ;
#27818 = CARTESIAN_POINT ( 'NONE',  ( 7.111342659921327858, -99.99762666413238321, 15.77675795231586697 ) ) ;
#27819 = PLANE ( 'NONE',  #22235 ) ;
#27820 = ORIENTED_EDGE ( 'NONE', *, *, #7639, .F. ) ;
#27821 = VECTOR ( 'NONE', #28094, 1000.000000000000114 ) ;
#27822 = CARTESIAN_POINT ( 'NONE',  ( -18.26355152109625379, -98.33636770627157375, 5.096710379585314143 ) ) ;
#27823 = ORIENTED_EDGE ( 'NONE', *, *, #21286, .T. ) ;
#27824 = DIRECTION ( 'NONE',  ( 0.4794255386042041156, 0.000000000000000000, 0.8775825618903722036 ) ) ;
#27825 = CARTESIAN_POINT ( 'NONE',  ( -6.273729852859999845, -101.4254868729999970, 14.68495471219999970 ) ) ;
#27826 = ORIENTED_EDGE ( 'NONE', *, *, #7093, .T. ) ;
#27827 = CARTESIAN_POINT ( 'NONE',  ( -3.253648539801173634, -97.41291607254315466, -20.33721584584428399 ) ) ;
#27828 = ADVANCED_FACE ( 'NONE', ( #2555 ), #6472, .F. ) ;
#27829 = CIRCLE ( 'NONE', #13871, 7.000000000000000000 ) ;
#27830 = CARTESIAN_POINT ( 'NONE',  ( -25.09792694589999940, -16.00000000000000000, -45.94144711499999545 ) ) ;
#27831 = CARTESIAN_POINT ( 'NONE',  ( -13.17202554217881172, -101.5620304352245000, -9.196801823362664052 ) ) ;
#27832 = CYLINDRICAL_SURFACE ( 'NONE', #18104, 4.750000000000000888 ) ;
#27833 = CARTESIAN_POINT ( 'NONE',  ( 47.02598405681334981, -79.63081725461873361, -2.257492274610140015 ) ) ;
#27834 = ORIENTED_EDGE ( 'NONE', *, *, #1133, .T. ) ;
#27835 = CARTESIAN_POINT ( 'NONE',  ( 46.25000000000000000, -79.00000000000000000, -13.75000000000000000 ) ) ;
#27836 = DIRECTION ( 'NONE',  ( 0.7071067811865475727, 0.000000000000000000, -0.7071067811865475727 ) ) ;
#27837 = CARTESIAN_POINT ( 'NONE',  ( 14.84965784370000108, -101.2530993010000060, 3.216001622850000352 ) ) ;
#27838 = CARTESIAN_POINT ( 'NONE',  ( -1.157192565939999973, -53.84184168659999870, -23.27396048310000154 ) ) ;
#27839 = CARTESIAN_POINT ( 'NONE',  ( -1.540392455020000106, -79.77809169310000925, 47.20175211690000339 ) ) ;
#27840 = ORIENTED_EDGE ( 'NONE', *, *, #14394, .T. ) ;
#27841 = CIRCLE ( 'NONE', #23212, 3.500000000000003109 ) ;
#27842 = DIRECTION ( 'NONE',  ( 1.000000000000000000, 0.000000000000000000, 0.000000000000000000 ) ) ;
#27843 = DIRECTION ( 'NONE',  ( 0.000000000000000000, 0.000000000000000000, -1.000000000000000000 ) ) ;
#27844 = FACE_OUTER_BOUND ( 'NONE', #1595, .T. ) ;
#27845 = CARTESIAN_POINT ( 'NONE',  ( 29.82685776330000138, -73.10703858080000828, -25.25856749939999801 ) ) ;
#27846 = CARTESIAN_POINT ( 'NONE',  ( -26.69293917519999937, -19.70310889130000120, -48.86109741659999628 ) ) ;
#27847 =( LENGTH_UNIT ( ) NAMED_UNIT ( * ) SI_UNIT ( .MILLI., .METRE. ) );
#27848 = AXIS2_PLACEMENT_3D ( 'NONE', #24181, #4215, #13536 ) ;
#27849 = ORIENTED_EDGE ( 'NONE', *, *, #6763, .F. ) ;
#27850 = CARTESIAN_POINT ( 'NONE',  ( -40.08893529113748855, -74.03750509262607693, -7.249551406113103447 ) ) ;
#27851 = ORIENTED_EDGE ( 'NONE', *, *, #13945, .F. ) ;
#27852 = CARTESIAN_POINT ( 'NONE',  ( -13.08859102019999909, -101.0314399550000104, -8.948266247160001186 ) ) ;
#27853 = TOROIDAL_SURFACE ( 'NONE', #14813, 3.500000000000000000, 0.5000000000000000000 ) ;
#27854 = CIRCLE ( 'NONE', #15255, 10.00000000000000000 ) ;
#27855 = EDGE_CURVE ( 'NONE', #2986, #13987, #3279, .T. ) ;
#27856 = CARTESIAN_POINT ( 'NONE',  ( 3.907985046679999924E-15, -73.50000000000000000, -40.00000000000000000 ) ) ;
#27857 = CARTESIAN_POINT ( 'NONE',  ( -7.700314492880000472, -100.7430069139999915, 14.58460939829999958 ) ) ;
#27858 = ORIENTED_EDGE ( 'NONE', *, *, #9782, .T. ) ;
#27859 = CARTESIAN_POINT ( 'NONE',  ( 3.969098514279999712, -92.85282594270000800, 28.21540908839999773 ) ) ;
#27860 = DIRECTION ( 'NONE',  ( 0.000000000000000000, 1.000000000000000000, 0.000000000000000000 ) ) ;
#27861 = CARTESIAN_POINT ( 'NONE',  ( 7.611014957459999231, -101.5361728780000021, 14.07441484610000160 ) ) ;
#27862 = VERTEX_POINT ( 'NONE', #2697 ) ;
#27863 = EDGE_CURVE ( 'NONE', #12535, #584, #2223, .T. ) ;
#27864 = CARTESIAN_POINT ( 'NONE',  ( -40.39659210501955044, -74.26034152734142424, 7.239203719547485427 ) ) ;
#27865 = FACE_OUTER_BOUND ( 'NONE', #25846, .T. ) ;
#27866 = FACE_OUTER_BOUND ( 'NONE', #632, .T. ) ;
#27867 = ORIENTED_EDGE ( 'NONE', *, *, #7751, .F. ) ;
#27868 = CARTESIAN_POINT ( 'NONE',  ( 18.94592261899999741, -19.18584073480000285, -9.024080787970000017 ) ) ;
#27869 = EDGE_CURVE ( 'NONE', #19768, #28710, #2996, .T. ) ;
#27870 = CARTESIAN_POINT ( 'NONE',  ( -14.06220372179999956, -74.01102208230000201, 36.25327798059999651 ) ) ;
#27871 = CARTESIAN_POINT ( 'NONE',  ( -18.27190991239999818, -94.89419557770000324, 16.28310526140000292 ) ) ;
#27872 = CARTESIAN_POINT ( 'NONE',  ( 7.627566167509999495, -74.00000000000000000, -38.62788938250000115 ) ) ;
#27873 = EDGE_CURVE ( 'NONE', #10298, #14992, #5010, .T. ) ;
#27874 = CARTESIAN_POINT ( 'NONE',  ( -1.328705758835786233, -74.17186053442132732, 47.12725970932369535 ) ) ;
#27875 = CARTESIAN_POINT ( 'NONE',  ( -0.1711623186869999924, -101.1411470200000053, -15.38827638959999966 ) ) ;
#27876 = CARTESIAN_POINT ( 'NONE',  ( 22.33353630010000046, -57.45905992459999823, -8.600016955360000992 ) ) ;
#27877 = CARTESIAN_POINT ( 'NONE',  ( 15.82520484449999998, -101.1659666750000071, 2.449319158209999792 ) ) ;
#27878 = CARTESIAN_POINT ( 'NONE',  ( 8.408940298597524787, -35.33620340784488434, -20.95510887256177313 ) ) ;
#27879 = CARTESIAN_POINT ( 'NONE',  ( -10.83788578300000083, -34.62274519420000018, -21.57372758079999997 ) ) ;
#27880 = ORIENTED_EDGE ( 'NONE', *, *, #19891, .T. ) ;
#27881 = CONICAL_SURFACE ( 'NONE', #385, 55.67692378859999280, 1.047197551199999799 ) ;
#27882 = AXIS2_PLACEMENT_3D ( 'NONE', #25961, #23770, #3813 ) ;
#27883 = CARTESIAN_POINT ( 'NONE',  ( 6.651374809830000068, -101.0640712160000021, 14.66145036780000055 ) ) ;
#27884 = DIRECTION ( 'NONE',  ( 0.4794255386042041156, 0.000000000000000000, 0.8775825618903722036 ) ) ;
#27885 = CIRCLE ( 'NONE', #19044, 0.4999999999999990008 ) ;
#27886 = CARTESIAN_POINT ( 'NONE',  ( -11.80897046999999844, -94.89420189129998562, -21.43714095509999851 ) ) ;
#27887 = CARTESIAN_POINT ( 'NONE',  ( -0.7205257401540000606, -101.6484611540000031, -15.98376809950000066 ) ) ;
#27888 = CARTESIAN_POINT ( 'NONE',  ( 6.867289776849999861, -92.50000000000000000, 29.52484619129999643 ) ) ;
#27889 = LINE ( 'NONE', #3290, #22800 ) ;
#27890 = CARTESIAN_POINT ( 'NONE',  ( -4.500000000000000000, -15.00000000000000000, -50.00000000000000000 ) ) ;
#27891 = DIRECTION ( 'NONE',  ( 0.000000000000000000, -1.000000000000000000, 0.000000000000000000 ) ) ;
#27892 = CARTESIAN_POINT ( 'NONE',  ( 20.82664911639999872, -28.53805357630000117, -8.124862095080001012 ) ) ;
#27893 = CARTESIAN_POINT ( 'NONE',  ( 27.89292634430000106, -72.00000000000000000, 12.34776042340000046 ) ) ;
#27894 = ORIENTED_EDGE ( 'NONE', *, *, #6243, .F. ) ;
#27895 = CIRCLE ( 'NONE', #12970, 6.749999999999999112 ) ;
#27896 = CARTESIAN_POINT ( 'NONE',  ( 0.000000000000000000, -94.59276292389999696, 0.000000000000000000 ) ) ;
#27897 = DIRECTION ( 'NONE',  ( 1.000000000000000000, 0.000000000000000000, 0.000000000000000000 ) ) ;
#27898 = ORIENTED_EDGE ( 'NONE', *, *, #9274, .T. ) ;
#27899 = EDGE_CURVE ( 'NONE', #28309, #23896, #2619, .T. ) ;
#27900 = CARTESIAN_POINT ( 'NONE',  ( 7.215414233289999757, -74.50000000000000000, -40.70731707320000226 ) ) ;
#27901 = ORIENTED_EDGE ( 'NONE', *, *, #23120, .F. ) ;
#27903 = EDGE_CURVE ( 'NONE', #1018, #10833, #847, .T. ) ;
#27902 = CIRCLE ( 'NONE', #19066, 60.85000000000000142 ) ;
#27904 = AXIS2_PLACEMENT_3D ( 'NONE', #18346, #5510, #7272 ) ;
#27905 = CARTESIAN_POINT ( 'NONE',  ( 0.3082441019822620976, -101.4241070620154233, -16.17049741965218956 ) ) ;
#27906 = CARTESIAN_POINT ( 'NONE',  ( 6.592724576960000249, -99.70407914540000149, 15.88227091829999971 ) ) ;
#27907 = CARTESIAN_POINT ( 'NONE',  ( 13.35210321545571333, -92.71346081467784472, 27.42209601977759093 ) ) ;
#27908 = B_SPLINE_CURVE_WITH_KNOTS ( 'NONE', 5,
 ( #10163, #19634, #26055, #19217, #10573, #3909, #21685, #3499, #28104 ),
 .UNSPECIFIED., .F., .F.,
 ( 6, 3, 6 ),
 ( 0.000000000000000000, 0.5000000000000000000, 1.000000000000000000 ),
 .UNSPECIFIED. ) ;
#27909 = CARTESIAN_POINT ( 'NONE',  ( 7.584268328590000330, -111.0000000000000000, 14.08825304710000026 ) ) ;
#27910 = EDGE_CURVE ( 'NONE', #28554, #25683, #15798, .T. ) ;
#27911 = CARTESIAN_POINT ( 'NONE',  ( 26.58635620580000136, -73.91993066429999715, -28.92424498180000114 ) ) ;
#27912 = EDGE_CURVE ( 'NONE', #24436, #14792, #8699, .T. ) ;
#27913 = LINE ( 'NONE', #14906, #11826 ) ;
#27914 = B_SPLINE_CURVE_WITH_KNOTS ( 'NONE', 3,
 ( #20890, #27154, #805, #14183 ),
 .UNSPECIFIED., .F., .F.,
 ( 4, 4 ),
 ( 0.000000000000000000, 1.000000000000000000 ),
 .UNSPECIFIED. ) ;
#27915 = CARTESIAN_POINT ( 'NONE',  ( -14.64568814080000081, -101.2530993010000060, 4.044604232330000215 ) ) ;
#27916 = CARTESIAN_POINT ( 'NONE',  ( -11.91832687610000185, -65.33654462490000014, -22.94749264700000069 ) ) ;
#27917 = DIRECTION ( 'NONE',  ( 0.5503789995269310342, 0.000000000000000000, -0.8349149399068952482 ) ) ;
#27918 = CARTESIAN_POINT ( 'NONE',  ( 19.36781163719999910, -19.46510053389999939, 10.50580276810000058 ) ) ;
#27919 = VERTEX_POINT ( 'NONE', #22803 ) ;
#27920 = CARTESIAN_POINT ( 'NONE',  ( 32.75000000000000000, -73.00000000000000000, 1.546052475400000102E-15 ) ) ;
#27921 = EDGE_LOOP ( 'NONE', ( #13812, #24347, #14530, #4921, #17618, #14986 ) ) ;
#27922 = AXIS2_PLACEMENT_3D ( 'NONE', #8588, #17491, #15424 ) ;
#27923 = AXIS2_PLACEMENT_3D ( 'NONE', #12186, #11902, #18771 ) ;
#27924 = FACE_OUTER_BOUND ( 'NONE', #21007, .T. ) ;
#27925 = CARTESIAN_POINT ( 'NONE',  ( -27.96632252730000090, -92.66001714109999909, 1.737774121780000014 ) ) ;
#27926 = CARTESIAN_POINT ( 'NONE',  ( 46.25000000000000000, -77.00000000000000000, -14.75000000000000000 ) ) ;
#27927 = EDGE_LOOP ( 'NONE', ( #17414, #12987, #27515, #15123 ) ) ;
#27928 = DIRECTION ( 'NONE',  ( 0.000000000000000000, 1.000000000000000000, 0.000000000000000000 ) ) ;
#27929 = ADVANCED_FACE ( 'NONE', ( #18721 ), #14312, .F. ) ;
#27930 = DIRECTION ( 'NONE',  ( 0.000000000000000000, 1.000000000000000000, 0.000000000000000000 ) ) ;
#27931 = VERTEX_POINT ( 'NONE', #16660 ) ;
#27932 = LINE ( 'NONE', #27671, #26143 ) ;
#27933 = CARTESIAN_POINT ( 'NONE',  ( -29.76178938840000043, -111.0000000000000000, 6.669774538800000485 ) ) ;
#27934 = ADVANCED_FACE ( 'NONE', ( #2841 ), #7811, .T. ) ;
#27935 = TOROIDAL_SURFACE ( 'NONE', #1430, 10.50000000000000000, 0.5000000000000000000 ) ;
#27936 = DIRECTION ( 'NONE',  ( 1.000000000000000000, 0.000000000000000000, 0.000000000000000000 ) ) ;
#27937 = ORIENTED_EDGE ( 'NONE', *, *, #25132, .F. ) ;
#27938 = CIRCLE ( 'NONE', #24212, 11.00000000000000000 ) ;
#27939 = EDGE_CURVE ( 'NONE', #13659, #17905, #28245, .T. ) ;
#27940 = DIRECTION ( 'NONE',  ( -1.000000000000000000, 0.000000000000000000, 0.000000000000000000 ) ) ;
#27941 = AXIS2_PLACEMENT_3D ( 'NONE', #11304, #9270, #18171 ) ;
#27942 = CARTESIAN_POINT ( 'NONE',  ( -16.17838246639999866, -100.4713644509999995, 2.927895792630000216 ) ) ;
#27943 = CARTESIAN_POINT ( 'NONE',  ( 0.000000000000000000, -110.0000000000000000, 0.000000000000000000 ) ) ;
#27944 = CARTESIAN_POINT ( 'NONE',  ( -5.998097866333861994, -101.1962283502516158, 14.03978137420685890 ) ) ;
#27945 = VERTEX_POINT ( 'NONE', #9526 ) ;
#27946 = CARTESIAN_POINT ( 'NONE',  ( 20.36577900666061325, -98.12113811797581775, -1.382477163405677389 ) ) ;
#27947 = CARTESIAN_POINT ( 'NONE',  ( -1.684828471230000124, -18.50000000000000000, -21.44817583509999892 ) ) ;
#27948 = CARTESIAN_POINT ( 'NONE',  ( -7.717204813168451416, -100.8945630372283517, 14.68338577015975233 ) ) ;
#27949 = ORIENTED_EDGE ( 'NONE', *, *, #19452, .F. ) ;
#27950 = CARTESIAN_POINT ( 'NONE',  ( 0.000000000000000000, -84.00000000000000000, 40.00000000000000000 ) ) ;
#27951 = CARTESIAN_POINT ( 'NONE',  ( -9.597487326430000465, -80.00000000000000000, 38.57396449699999863 ) ) ;
#27952 = DIRECTION ( 'NONE',  ( 0.000000000000000000, -1.000000000000000000, 0.000000000000000000 ) ) ;
#27953 = VERTEX_POINT ( 'NONE', #23096 ) ;
#27954 = CARTESIAN_POINT ( 'NONE',  ( 36.86594131523432338, -79.67252481679619791, -14.49340671423261462 ) ) ;
#27955 = CARTESIAN_POINT ( 'NONE',  ( 6.656876267563871963, -101.0147714271303698, 15.09013656268733072 ) ) ;
#27956 = TOROIDAL_SURFACE ( 'NONE', #16791, 3.500000000000000000, 0.5000000000000000000 ) ;
#27957 = DIRECTION ( 'NONE',  ( -0.3790931394101558771, -0.6121731929912518355, -0.6939253370752848094 ) ) ;
#27958 = CIRCLE ( 'NONE', #18685, 2.000000000000000000 ) ;
#27959 = ORIENTED_EDGE ( 'NONE', *, *, #27666, .T. ) ;
#27960 = AXIS2_PLACEMENT_3D ( 'NONE', #7616, #5411, #16758 ) ;
#27961 = CARTESIAN_POINT ( 'NONE',  ( 47.18156631880000162, -74.63487131880000902, -1.134746784699999900 ) ) ;
#27962 = EDGE_LOOP ( 'NONE', ( #15428, #21089, #8887, #18981 ) ) ;
#27963 = CARTESIAN_POINT ( 'NONE',  ( 27.45142615009999787, -92.87863191399999607, 9.755964952359999387 ) ) ;
#27964 = CARTESIAN_POINT ( 'NONE',  ( -5.298188773579999733, -100.9197086960000007, 14.69882804600000092 ) ) ;
#27965 = ORIENTED_EDGE ( 'NONE', *, *, #21438, .F. ) ;
#27966 = CARTESIAN_POINT ( 'NONE',  ( -26.60903970598167589, -15.80000000000000071, -48.70752046822583736 ) ) ;
#27967 = DIRECTION ( 'NONE',  ( 0.000000000000000000, 1.000000000000000000, 0.000000000000000000 ) ) ;
#27968 = ADVANCED_FACE ( 'NONE', ( #7658 ), #377, .F. ) ;
#27969 = EDGE_CURVE ( 'NONE', #8453, #25457, #9640, .T. ) ;
#27970 = CARTESIAN_POINT ( 'NONE',  ( 40.70731707320000226, -74.50000000000000000, 7.215414233289999757 ) ) ;
#27971 = CARTESIAN_POINT ( 'NONE',  ( -26.69293917519999937, -26.29689110869999880, -48.86109741659999628 ) ) ;
#27972 = EDGE_CURVE ( 'NONE', #3865, #23386, #26545, .T. ) ;
#27973 = CARTESIAN_POINT ( 'NONE',  ( 20.34628061889999984, -52.63293862049999916, 11.13082833170000008 ) ) ;
#27974 = CARTESIAN_POINT ( 'NONE',  ( 4.929390229339999696E-15, -84.50000000000000000, 40.00000000000000000 ) ) ;
#27975 = ORIENTED_EDGE ( 'NONE', *, *, #19305, .F. ) ;
#27976 = CARTESIAN_POINT ( 'NONE',  ( -13.22728828230000175, -99.73367660430000115, -11.16491717010000073 ) ) ;
#27977 = CARTESIAN_POINT ( 'NONE',  ( 8.988996100299999625, -34.66800400750000222, -19.43643858049999906 ) ) ;
#27978 = DIRECTION ( 'NONE',  ( 1.000000000000000000, 0.000000000000000000, 0.000000000000000000 ) ) ;
#27979 = CARTESIAN_POINT ( 'NONE',  ( 24.22375112459999968, -93.90388142510001046, -8.961400531120000679 ) ) ;
#27980 = ORIENTED_EDGE ( 'NONE', *, *, #12172, .F. ) ;
#27981 = CARTESIAN_POINT ( 'NONE',  ( -3.072375608539999803, -79.99928376260000107, 46.95756812850000017 ) ) ;
#27982 = CARTESIAN_POINT ( 'NONE',  ( -15.04362262010000073, -66.18012799950000158, 22.59069390079999806 ) ) ;
#27983 = ORIENTED_EDGE ( 'NONE', *, *, #27129, .T. ) ;
#27984 = CONICAL_SURFACE ( 'NONE', #2875, 13.13304743849999667, 0.9119902906770002149 ) ;
#27985 = CARTESIAN_POINT ( 'NONE',  ( -17.42343749999999858, -77.00000000000000000, 43.92022684009999978 ) ) ;
#27986 = VECTOR ( 'NONE', #11260, 1000.000000000000000 ) ;
#27987 = DIRECTION ( 'NONE',  ( 1.000000000000000000, 0.000000000000000000, 0.000000000000000000 ) ) ;
#27988 = CARTESIAN_POINT ( 'NONE',  ( 38.65106240728522380, -73.99999920929936081, 7.498734568567305914 ) ) ;
#27989 = CARTESIAN_POINT ( 'NONE',  ( 29.90404901189999620, -73.44398176539999668, -25.16348247620000222 ) ) ;
#27990 = CARTESIAN_POINT ( 'NONE',  ( -14.47589974207729568, -74.09467030769806684, 36.25997764697337544 ) ) ;
#27991 = DIRECTION ( 'NONE',  ( 1.000000000000000000, 0.000000000000000000, 0.000000000000000000 ) ) ;
#27992 = B_SPLINE_SURFACE_WITH_KNOTS ( 'NONE', 5, 5, ( 
 ( #27599, #5296, #7770, #11973, #25533, #14316, #5572, #14456, #12257 ),
 ( #23349, #3393, #25680, #18974, #27852, #1764, #3662, #21715, #16926 ),
 ( #1634, #3941, #16782, #8445, #24040, #10198, #4078, #7904, #10603 ),
 ( #25819, #28138, #17347, #12806, #5705, #8298, #26240, #12946, #21299 ),
 ( #12526, #14589, #12665, #10063, #21437, #5974, #3805, #21577, #14993 ),
 ( #14725, #21859, #23491, #8172, #17202, #1496, #19114, #1350, #3530 ) ),
 .UNSPECIFIED., .F., .F., .F.,
 ( 6, 6 ),
 ( 6, 3, 6 ),
 ( 4.816191416729999730, 6.255250589890000157 ),
 ( 0.000000000000000000, 0.2500000000000000000, 0.5000000000000000000 ),
 .UNSPECIFIED. ) ;
#27993 = EDGE_CURVE ( 'NONE', #26731, #20895, #6862, .T. ) ;
#27994 = ORIENTED_EDGE ( 'NONE', *, *, #19369, .T. ) ;
#27995 = CARTESIAN_POINT ( 'NONE',  ( 20.57859482010000107, -35.48124439810000297, -8.749812979389998802 ) ) ;
#27996 = AXIS2_PLACEMENT_3D ( 'NONE', #16827, #14630, #23529 ) ;
#27997 = CARTESIAN_POINT ( 'NONE',  ( -25.37284092810000047, -111.0000000000000000, 2.543411731580000001 ) ) ;
#27998 = FACE_OUTER_BOUND ( 'NONE', #12317, .T. ) ;
#27999 = ORIENTED_EDGE ( 'NONE', *, *, #19311, .F. ) ;
#28000 = AXIS2_PLACEMENT_3D ( 'NONE', #2369, #25100, #4691 ) ;
#28001 = CARTESIAN_POINT ( 'NONE',  ( 9.165534020729998232, -98.33329995120000433, 16.60371393490000003 ) ) ;
#28002 = AXIS2_PLACEMENT_3D ( 'NONE', #21223, #14509, #1275 ) ;
#28003 = EDGE_CURVE ( 'NONE', #3837, #17168, #25931, .T. ) ;
#28004 = DIRECTION ( 'NONE',  ( 1.000000000000000000, 0.000000000000000000, 0.000000000000000000 ) ) ;
#28005 = CARTESIAN_POINT ( 'NONE',  ( -8.176071803510000180, -99.94549701829998867, 14.79262394269999881 ) ) ;
#28006 = CARTESIAN_POINT ( 'NONE',  ( -1.526193099469999925, -100.8869807189999932, -15.59252015110000045 ) ) ;
#28007 = CARTESIAN_POINT ( 'NONE',  ( 11.86655840719999944, -101.3150700380000018, -11.10431293650000129 ) ) ;
#28008 = FACE_OUTER_BOUND ( 'NONE', #27561, .T. ) ;
#28009 = ORIENTED_EDGE ( 'NONE', *, *, #23307, .T. ) ;
#28010 = CARTESIAN_POINT ( 'NONE',  ( 13.05506823074590450, -101.2145573445107232, -9.820936334222084341 ) ) ;
#28011 = CARTESIAN_POINT ( 'NONE',  ( 7.215414233289999757, -74.50000000000000000, -40.70731707320000226 ) ) ;
#28012 = CARTESIAN_POINT ( 'NONE',  ( -13.00673796568629648, -19.48509974121062172, 19.66549047931116689 ) ) ;
#28013 = FACE_OUTER_BOUND ( 'NONE', #23148, .T. ) ;
#28014 = ORIENTED_EDGE ( 'NONE', *, *, #14543, .F. ) ;
#28015 = CARTESIAN_POINT ( 'NONE',  ( 18.94592261899999741, -19.50000000009999823, -9.024080787920000901 ) ) ;
#28016 = FACE_OUTER_BOUND ( 'NONE', #28225, .T. ) ;
#28017 = DIRECTION ( 'NONE',  ( 0.000000000000000000, 1.000000000000000000, 0.000000000000000000 ) ) ;
#28018 = CARTESIAN_POINT ( 'NONE',  ( -18.16554934440000224, -94.32610680340000897, 17.27505836280000295 ) ) ;
#28019 = CARTESIAN_POINT ( 'NONE',  ( -17.56889148192910355, -92.66777315148752336, 24.93158845175500460 ) ) ;
#28020 = EDGE_LOOP ( 'NONE', ( #25305, #22552, #20770, #5910 ) ) ;
#28021 = CYLINDRICAL_SURFACE ( 'NONE', #17439, 0.4999999999999982236 ) ;
#28022 = FACE_OUTER_BOUND ( 'NONE', #12744, .T. ) ;
#28023 = CARTESIAN_POINT ( 'NONE',  ( 27.10195004252156892, -92.50000267095391848, -12.39581383284575722 ) ) ;
#28024 = CARTESIAN_POINT ( 'NONE',  ( 15.19718069640000024, -101.1364147039999892, 2.131293228500000581 ) ) ;
#28025 = CARTESIAN_POINT ( 'NONE',  ( 21.12062292599999580, -58.34046154589999844, 10.52028212929999995 ) ) ;
#28026 = DIRECTION ( 'NONE',  ( 0.000000000000000000, 1.000000000000000000, 0.000000000000000000 ) ) ;
#28027 = TOROIDAL_SURFACE ( 'NONE', #16396, 9.000000000000000000, 2.000000000000000000 ) ;
#28028 = EDGE_LOOP ( 'NONE', ( #3705, #28521, #18768, #8402 ) ) ;
#28029 = ADVANCED_FACE ( 'NONE', ( #12280 ), #12434, .T. ) ;
#28030 = CARTESIAN_POINT ( 'NONE',  ( 6.750186163829999586, -101.4829589650000088, 14.64766651940000131 ) ) ;
#28031 = CARTESIAN_POINT ( 'NONE',  ( 15.53854631970000000, -101.2063419769999939, 3.759158181819999722 ) ) ;
#28032 = CARTESIAN_POINT ( 'NONE',  ( -11.51095922780000080, -94.71799100319999809, -20.64292660030000093 ) ) ;
#28033 = CARTESIAN_POINT ( 'NONE',  ( 4.438282752932665609, -92.81370807104723042, -30.17535407529405589 ) ) ;
#28034 = ADVANCED_FACE ( 'NONE', ( #25701 ), #22697, .T. ) ;
#28035 = CARTESIAN_POINT ( 'NONE',  ( -6.544663280410000006, -97.83383802230000015, 18.86537983400000229 ) ) ;
#28036 = CARTESIAN_POINT ( 'NONE',  ( 1.723886190540000030, -92.49999926799999628, -29.27157131740000295 ) ) ;
#28037 = DIRECTION ( 'NONE',  ( 0.000000000000000000, -1.000000000000000000, 0.000000000000000000 ) ) ;
#28038 = AXIS2_PLACEMENT_3D ( 'NONE', #13181, #8525, #17426 ) ;
#28039 = ORIENTED_EDGE ( 'NONE', *, *, #11974, .F. ) ;
#28040 = STYLED_ITEM ( 'NONE', ( #16542 ), #6684 ) ;
#28041 = CARTESIAN_POINT ( 'NONE',  ( 0.000000000000000000, -16.50000000000000000, 0.000000000000000000 ) ) ;
#28042 = CARTESIAN_POINT ( 'NONE',  ( -5.390284282690000595, -100.8869817940000075, 14.71056662440000018 ) ) ;
#28043 = ORIENTED_EDGE ( 'NONE', *, *, #10109, .T. ) ;
#28044 = AXIS2_PLACEMENT_3D ( 'NONE', #18547, #4987, #20589 ) ;
#28045 = CARTESIAN_POINT ( 'NONE',  ( -1.099649763710000006, -101.5317765570000006, -16.05045154129999929 ) ) ;
#28046 = CARTESIAN_POINT ( 'NONE',  ( -7.346953802149999824, -74.24999999150000463, 39.87739400550000113 ) ) ;
#28047 = CARTESIAN_POINT ( 'NONE',  ( 46.25000000000000000, -80.00000000000000000, -4.582575694960000057 ) ) ;
#28048 = CARTESIAN_POINT ( 'NONE',  ( 15.11157726140000079, -100.8815367389999977, 4.163621051679999852 ) ) ;
#28049 = CARTESIAN_POINT ( 'NONE',  ( 27.75394116159999669, -74.50000000000000000, -27.75394116159999669 ) ) ;
#28050 = CARTESIAN_POINT ( 'NONE',  ( 10.20110288159999890, -74.00000000000000000, -41.00000000000000000 ) ) ;
#28051 = PRODUCT_DEFINITION_SHAPE ( 'NONE', 'NONE',  #28060 ) ;
#28052 = CYLINDRICAL_SURFACE ( 'NONE', #5546, 39.24999999999998579 ) ;
#28053 = CARTESIAN_POINT ( 'NONE',  ( -11.77695074510000062, -64.47177033809998647, -23.22164031879999868 ) ) ;
#28054 = CARTESIAN_POINT ( 'NONE',  ( 24.04216374601140771, -94.35876167748494936, -8.283021781734792199 ) ) ;
#28055 = FACE_OUTER_BOUND ( 'NONE', #24767, .T. ) ;
#28056 = EDGE_LOOP ( 'NONE', ( #22446, #17526, #6084, #21990, #17017 ) ) ;
#28057 = CARTESIAN_POINT ( 'NONE',  ( -40.50000000000000000, -65.63577453799999262, 2.309401076760000393 ) ) ;
#28058 = AXIS2_PLACEMENT_3D ( 'NONE', #26857, #22490, #6752 ) ;
#28059 = EDGE_LOOP ( 'NONE', ( #7927, #5409, #14943, #1694, #27820, #3962, #10641 ) ) ;
#28060 = PRODUCT_DEFINITION ( 'UNKNOWN', '', #2266, #4506 ) ;
#28061 = AXIS2_PLACEMENT_3D ( 'NONE', #3326, #14252, #23141 ) ;
#28062 = ADVANCED_FACE ( 'NONE', ( #19133 ), #24070, .F. ) ;
#28063 = CARTESIAN_POINT ( 'NONE',  ( -2.605870651600000087, -64.47177090210000472, -25.91540045190000185 ) ) ;
#28064 = ADVANCED_FACE ( 'NONE', ( #28022 ), #10561, .T. ) ;
#28065 = DIRECTION ( 'NONE',  ( 0.7436828042389473925, 0.000000000000000000, -0.6685326369589560391 ) ) ;
#28066 = CARTESIAN_POINT ( 'NONE',  ( -19.54048411319999801, -52.63055504209999924, 12.61913916920000034 ) ) ;
#28067 = EDGE_CURVE ( 'NONE', #12325, #6364, #1742, .T. ) ;
#28068 = EDGE_LOOP ( 'NONE', ( #9381, #10599, #5221, #1909 ) ) ;
#28069 = AXIS2_PLACEMENT_3D ( 'NONE', #16377, #19412, #25705 ) ;
#28070 = CARTESIAN_POINT ( 'NONE',  ( -17.92889229695188291, -97.41291607277516107, -10.13624181689873716 ) ) ;
#28071 = CARTESIAN_POINT ( 'NONE',  ( -7.627568735119999666, -74.00000000000000000, -38.62788659690000515 ) ) ;
#28072 = ORIENTED_EDGE ( 'NONE', *, *, #27159, .T. ) ;
#28073 = CARTESIAN_POINT ( 'NONE',  ( 7.533204440554428061, -37.08603407206901892, -21.49405318675248822 ) ) ;
#28074 = CARTESIAN_POINT ( 'NONE',  ( -14.59919346459999900, -79.65691081869999834, 36.80099829179999205 ) ) ;
#28075 = CIRCLE ( 'NONE', #3879, 1.999999999999999112 ) ;
#28076 = CARTESIAN_POINT ( 'NONE',  ( -7.333297298759998917, -94.59276292389999696, -22.63874378639999563 ) ) ;
#28077 = FACE_OUTER_BOUND ( 'NONE', #19228, .T. ) ;
#28078 = CARTESIAN_POINT ( 'NONE',  ( -16.78472755060580113, -98.73470581871430340, -7.771690127070184140 ) ) ;
#28079 = CARTESIAN_POINT ( 'NONE',  ( -20.00096871140000232, -59.03952408640000016, 12.17600098870000203 ) ) ;
#28080 = EDGE_LOOP ( 'NONE', ( #3583, #6762, #9098 ) ) ;
#28081 = CARTESIAN_POINT ( 'NONE',  ( 23.73263625450000092, -64.92652906329999496, -8.873745374080000303 ) ) ;
#28082 = CARTESIAN_POINT ( 'NONE',  ( -12.52932295349999947, -101.5216621940000152, -9.967556391629999624 ) ) ;
#28083 = CARTESIAN_POINT ( 'NONE',  ( -1.797800075250000074, -19.46723765599999822, -22.31531904799999921 ) ) ;
#28084 = DIRECTION ( 'NONE',  ( -0.000000000000000000, 1.000000000000000000, 0.000000000000000000 ) ) ;
#28085 = ORIENTED_EDGE ( 'NONE', *, *, #24110, .F. ) ;
#28086 = CIRCLE ( 'NONE', #10367, 3.749999999999996447 ) ;
#28087 = CARTESIAN_POINT ( 'NONE',  ( 11.70455088819999823, -101.1889999979999999, 8.942783294160001617 ) ) ;
#28088 = CARTESIAN_POINT ( 'NONE',  ( -41.75000000000000000, -65.63577453799999262, -1.587713240270000048 ) ) ;
#28089 = CARTESIAN_POINT ( 'NONE',  ( 11.69905354509999995, -15.49681045920000066, 21.41497386989999896 ) ) ;
#28090 = EDGE_LOOP ( 'NONE', ( #10548, #2937, #16799, #7230 ) ) ;
#28091 = ADVANCED_FACE ( 'NONE', ( #5133 ), #17839, .F. ) ;
#28092 = CARTESIAN_POINT ( 'NONE',  ( 6.662036864477173026, -100.9510322837155627, 15.14271383432438789 ) ) ;
#28093 = AXIS2_PLACEMENT_3D ( 'NONE', #18087, #26841, #2512 ) ;
#28094 = DIRECTION ( 'NONE',  ( 0.4381045938801422235, -0.4061384660531317525, 0.8019450799232605842 ) ) ;
#28095 = ADVANCED_FACE ( 'NONE', ( #25521 ), #13347, .F. ) ;
#28096 = ORIENTED_EDGE ( 'NONE', *, *, #23951, .F. ) ;
#28097 = CARTESIAN_POINT ( 'NONE',  ( 47.25003994149999897, -74.79572188120000931, -0.5609601642099999452 ) ) ;
#28098 = ORIENTED_EDGE ( 'NONE', *, *, #12276, .F. ) ;
#28099 = CARTESIAN_POINT ( 'NONE',  ( 20.53262164509999721, -53.84414347720000649, 10.87832573719999907 ) ) ;
#28100 = DIRECTION ( 'NONE',  ( 1.000000000000000000, 0.000000000000000000, 0.000000000000000000 ) ) ;
#28101 = CARTESIAN_POINT ( 'NONE',  ( -7.261004788010000155, -74.03378462380000258, -40.00100507770000036 ) ) ;
#28102 = ORIENTED_EDGE ( 'NONE', *, *, #9646, .T. ) ;
#28103 = CARTESIAN_POINT ( 'NONE',  ( -42.25000000000000000, -63.30468293320000583, 0.7216878364880000563 ) ) ;
#28104 = CARTESIAN_POINT ( 'NONE',  ( 22.43277176080000146, -36.00000000000000000, -11.31764183710000005 ) ) ;
#28105 = VECTOR ( 'NONE', #8092, 1000.000000000000000 ) ;
#28106 = AXIS2_PLACEMENT_3D ( 'NONE', #14233, #13932, #14369 ) ;
#28107 = DIRECTION ( 'NONE',  ( 1.000000000000000000, 0.000000000000000000, 0.000000000000000000 ) ) ;
#28108 = DIRECTION ( 'NONE',  ( 0.4794255386042040601, 0.000000000000000000, 0.8775825618903720926 ) ) ;
#28109 = CARTESIAN_POINT ( 'NONE',  ( -27.59093974670000193, -39.32601556110000018, -50.50487643680000360 ) ) ;
#28110 = CARTESIAN_POINT ( 'NONE',  ( 25.04851980253549470, -66.68373043499040875, 10.87574838088278106 ) ) ;
#28111 = VERTEX_POINT ( 'NONE', #10182 ) ;
#28112 = CARTESIAN_POINT ( 'NONE',  ( 9.393614001710000494, -38.00000000000000000, -22.97877290430000130 ) ) ;
#28113 = CARTESIAN_POINT ( 'NONE',  ( 13.27522782530000001, -100.4731125450000064, -9.288511226849999858 ) ) ;
#28114 = FACE_OUTER_BOUND ( 'NONE', #23555, .T. ) ;
#28115 = CARTESIAN_POINT ( 'NONE',  ( 23.95450574879999905, -94.06807348049999007, -8.162316271139999913 ) ) ;
#28116 = EDGE_LOOP ( 'NONE', ( #1157, #24071, #19386, #2917 ) ) ;
#28117 = CIRCLE ( 'NONE', #239, 6.749999999999999112 ) ;
#28118 = CARTESIAN_POINT ( 'NONE',  ( 14.19394421396252071, -96.53847999818489711, -15.96643556996691515 ) ) ;
#28119 = CARTESIAN_POINT ( 'NONE',  ( -19.23238473919999691, -19.17792668139999890, 14.16443425210000129 ) ) ;
#28120 = ORIENTED_EDGE ( 'NONE', *, *, #5966, .T. ) ;
#28121 = DIRECTION ( 'NONE',  ( 0.000000000000000000, 1.000000000000000000, 0.000000000000000000 ) ) ;
#28122 = CARTESIAN_POINT ( 'NONE',  ( -18.59081129359999807, -92.50000000000000000, 24.17915911369999904 ) ) ;
#28123 = CARTESIAN_POINT ( 'NONE',  ( 0.000000000000000000, -10.95575221240000019, 0.000000000000000000 ) ) ;
#28124 = CARTESIAN_POINT ( 'NONE',  ( 8.563236930420002224, -35.95760432990000055, -20.91612140590000024 ) ) ;
#28125 = DIRECTION ( 'NONE',  ( 0.000000000000000000, 1.000000000000000000, 0.000000000000000000 ) ) ;
#28126 = ADVANCED_FACE ( 'NONE', ( #19234 ), #16635, .F. ) ;
#28127 = B_SPLINE_CURVE_WITH_KNOTS ( 'NONE', 5,
 ( #10247, #19301, #14640, #14903, #21215, #12717 ),
 .UNSPECIFIED., .F., .F.,
 ( 6, 6 ),
 ( 0.000000000000000000, 1.000000000000000000 ),
 .UNSPECIFIED. ) ;
#28128 =( NAMED_UNIT ( * ) PLANE_ANGLE_UNIT ( ) SI_UNIT ( $, .RADIAN. ) );
#28129 = AXIS2_PLACEMENT_3D ( 'NONE', #107, #8955, #27048 ) ;
#28130 = B_SPLINE_CURVE_WITH_KNOTS ( 'NONE', 5,
 ( #22415, #26792, #1873, #24006, #13215, #13503, #22123, #28520, #2462 ),
 .UNSPECIFIED., .F., .F.,
 ( 6, 3, 6 ),
 ( 0.000000000000000000, 0.5000000000000000000, 1.000000000000000000 ),
 .UNSPECIFIED. ) ;
#28131 = ADVANCED_FACE ( 'NONE', ( #5960 ), #26408, .T. ) ;
#28132 = EDGE_LOOP ( 'NONE', ( #7882, #15934, #17720, #9123 ) ) ;
#28133 = CARTESIAN_POINT ( 'NONE',  ( 28.44874375979999925, -10.08849557519999962, 52.07507615039999394 ) ) ;
#28134 = EDGE_LOOP ( 'NONE', ( #14376, #6291, #26279, #2817, #25915, #15847 ) ) ;
#28135 = CARTESIAN_POINT ( 'NONE',  ( 20.19624812569999861, -35.90543013560000674, -9.066694748779999813 ) ) ;
#28136 = CARTESIAN_POINT ( 'NONE',  ( 0.000000000000000000, -26.59999999999999787, 0.000000000000000000 ) ) ;
#28137 = ORIENTED_EDGE ( 'NONE', *, *, #23275, .F. ) ;
#28138 = CARTESIAN_POINT ( 'NONE',  ( -13.09607815989999935, -101.5026188610000020, -9.231260805549998949 ) ) ;
#28139 = CARTESIAN_POINT ( 'NONE',  ( 7.595444726729600567E-15, -73.50000000000000000, 32.25000000000000000 ) ) ;
#28140 = CARTESIAN_POINT ( 'NONE',  ( -0.5856137342820000313, -19.46510053389999939, -22.02591827759999887 ) ) ;
#28141 = TOROIDAL_SURFACE ( 'NONE', #14659, 0.5000000000000000000, 0.5000000000000000000 ) ;
#28142 = CARTESIAN_POINT ( 'NONE',  ( -1.589809170069999888, -93.96464232220000667, 24.84966672209999672 ) ) ;
#28143 = CARTESIAN_POINT ( 'NONE',  ( 9.307783803350000440, -57.43039249360000298, -22.95932595720000080 ) ) ;
#28144 = CARTESIAN_POINT ( 'NONE',  ( -40.31253929845618700, -65.70258710782171363, 2.225363999267659043 ) ) ;
#28145 = ORIENTED_EDGE ( 'NONE', *, *, #25811, .F. ) ;
#28146 = CARTESIAN_POINT ( 'NONE',  ( -40.00000000000000000, -82.25000000000000000, 0.000000000000000000 ) ) ;
#28147 = CARTESIAN_POINT ( 'NONE',  ( -28.39119738240000146, -92.85282594270000800, -2.408934254250000073 ) ) ;
#28148 = CARTESIAN_POINT ( 'NONE',  ( -15.55828293390000105, -101.6484611540000031, 3.733608462140000306 ) ) ;
#28149 = ORIENTED_EDGE ( 'NONE', *, *, #3151, .T. ) ;
#28150 = AXIS2_PLACEMENT_3D ( 'NONE', #12687, #8058, #21597 ) ;
#28151 = CARTESIAN_POINT ( 'NONE',  ( -8.852567479250000204, -98.72068567929999006, -16.20451607640000091 ) ) ;
#28152 = B_SPLINE_CURVE_WITH_KNOTS ( 'NONE', 3,
 ( #28641, #19616, #22106, #15218, #12888, #15369, #17583, #19900, #26471, #6508, #17009, #5922, #14806, #17734 ),
 .UNSPECIFIED., .F., .F.,
 ( 4, 2, 1, 1, 1, 1, 2, 2, 4 ),
 ( 0.000000000000000000, 0.2499999999998663291, 0.3749999999998062661, 0.4374999999997802869, 0.4687499999997731814, 0.4843749999997706279, 0.4921874999997750688, 0.4999999999997795097, 1.000000000000000000 ),
 .UNSPECIFIED. ) ;
#28153 = CARTESIAN_POINT ( 'NONE',  ( -14.57172147319999844, -74.36322263760000340, 36.76767988459999970 ) ) ;
#28154 = CARTESIAN_POINT ( 'NONE',  ( -18.05296197570000061, -94.57749224630001095, 16.11416072500000141 ) ) ;
#28155 = CARTESIAN_POINT ( 'NONE',  ( -41.75000000000000000, -65.63577453799999262, -1.587713240270000048 ) ) ;
#28156 = VERTEX_POINT ( 'NONE', #17185 ) ;
#28157 = B_SPLINE_CURVE_WITH_KNOTS ( 'NONE', 5,
 ( #7582, #3201, #27239, #5516, #7277, #14403 ),
 .UNSPECIFIED., .F., .F.,
 ( 6, 6 ),
 ( 0.000000000000000000, 1.000000000000000000 ),
 .UNSPECIFIED. ) ;
#28158 = CARTESIAN_POINT ( 'NONE',  ( -4.439198032609999743E-16, -74.50000000000000000, 47.25000000000000000 ) ) ;
#28159 = CARTESIAN_POINT ( 'NONE',  ( 0.05945881221699999414, -101.4908759489999994, -16.03087095909999960 ) ) ;
#28160 = CARTESIAN_POINT ( 'NONE',  ( 9.864792964790000340, -62.95257329789999545, -24.33712608820000156 ) ) ;
#28161 = CARTESIAN_POINT ( 'NONE',  ( -38.71640869449999656, -73.50000064450000536, -7.135466578850000019 ) ) ;
#28162 = CARTESIAN_POINT ( 'NONE',  ( 20.51027264869999911, -57.91805294160000273, 11.21560916570000010 ) ) ;
#28163 = CARTESIAN_POINT ( 'NONE',  ( -10.93265203729999868, -19.39368411250000079, -21.85641315899999881 ) ) ;
#28164 = ORIENTED_EDGE ( 'NONE', *, *, #17902, .F. ) ;
#28165 = EDGE_CURVE ( 'NONE', #1181, #25772, #9171, .T. ) ;
#28166 = EDGE_CURVE ( 'NONE', #8116, #5957, #27810, .T. ) ;
#28167 = CARTESIAN_POINT ( 'NONE',  ( 6.497518321730000324, -100.8455998110000138, 14.66870431030000077 ) ) ;
#28168 = CARTESIAN_POINT ( 'NONE',  ( 15.35292075490000130, -101.1617736559999940, 3.478357854820000039 ) ) ;
#28169 = CARTESIAN_POINT ( 'NONE',  ( -40.29219269051309027, -65.70788121356240197, -2.219015993087579464 ) ) ;
#28170 = DIRECTION ( 'NONE',  ( 0.4794255386042042266, 0.000000000000000000, 0.8775825618903720926 ) ) ;
#28171 = LINE ( 'NONE', #25984, #3200 ) ;
#28172 = EDGE_LOOP ( 'NONE', ( #2195, #10310, #25877, #12647 ) ) ;
#28173 = CARTESIAN_POINT ( 'NONE',  ( 0.2582735113180000264, -92.50000947299999154, -29.99035778690000242 ) ) ;
#28174 = CARTESIAN_POINT ( 'NONE',  ( 20.76917537310000128, -34.61672842239999426, -8.508194708340001355 ) ) ;
#28175 = CARTESIAN_POINT ( 'NONE',  ( -0.6842253573819999657, -101.2530993000000024, -15.17849927279999989 ) ) ;
#28176 = DIRECTION ( 'NONE',  ( 0.000000000000000000, 1.000000000000000000, 0.000000000000000000 ) ) ;
#28177 = EDGE_LOOP ( 'NONE', ( #17341, #16678, #14949, #24156 ) ) ;
#28178 = DIRECTION ( 'NONE',  ( 0.000000000000000000, -1.000000000000000000, 0.000000000000000000 ) ) ;
#28179 = FACE_OUTER_BOUND ( 'NONE', #18408, .T. ) ;
#28180 = VERTEX_POINT ( 'NONE', #26073 ) ;
#28181 = CARTESIAN_POINT ( 'NONE',  ( -0.8151688476029999020, -101.3256027080000052, -15.88609378809999839 ) ) ;
#28182 = EDGE_CURVE ( 'NONE', #8439, #4998, #28251, .T. ) ;
#28183 = DIRECTION ( 'NONE',  ( 0.9923152162251017705, 0.000000000000000000, 0.1237356522920117774 ) ) ;
#28184 = AXIS2_PLACEMENT_3D ( 'NONE', #776, #5116, #18817 ) ;
#28185 = CARTESIAN_POINT ( 'NONE',  ( 13.63898564678551217, -92.59735406129850332, 27.28055442926964247 ) ) ;
#28186 = CARTESIAN_POINT ( 'NONE',  ( 25.08988466659999972, -73.89104832229999431, -30.05843389639999685 ) ) ;
#28187 = CARTESIAN_POINT ( 'NONE',  ( -22.58183123469999742, -70.96441436690000160, 17.76382364619999876 ) ) ;
#28188 = FACE_OUTER_BOUND ( 'NONE', #9936, .T. ) ;
#28189 = CARTESIAN_POINT ( 'NONE',  ( -18.59048430349110959, -19.47314420526488021, 13.19884344879934090 ) ) ;
#28190 = FACE_OUTER_BOUND ( 'NONE', #25389, .T. ) ;
#28191 = DIRECTION ( 'NONE',  ( 0.000000000000000000, -1.000000000000000000, 0.000000000000000000 ) ) ;
#28192 = ORIENTED_EDGE ( 'NONE', *, *, #419, .T. ) ;
#28193 = EDGE_LOOP ( 'NONE', ( #5302, #910, #342, #4809, #16846 ) ) ;
#28194 = CARTESIAN_POINT ( 'NONE',  ( -13.87613801740000063, -58.81368956530000247, 21.27373992140000070 ) ) ;
#28195 = CARTESIAN_POINT ( 'NONE',  ( -2.349289058739999714, -62.62089253250000098, -25.05573335040000060 ) ) ;
#28196 = CARTESIAN_POINT ( 'NONE',  ( 10.95532170329999921, -36.00000000000000000, -21.46129409690000145 ) ) ;
#28197 = CARTESIAN_POINT ( 'NONE',  ( 4.500000000000000000, -11.00000000000000000, -31.00000000000000000 ) ) ;
#28198 = CARTESIAN_POINT ( 'NONE',  ( -40.00000000000000000, -69.50000000000000000, 2.464695114669999848E-15 ) ) ;
#28199 = B_SPLINE_CURVE_WITH_KNOTS ( 'NONE', 3,
 ( #26753, #10533, #19450, #28338 ),
 .UNSPECIFIED., .F., .F.,
 ( 4, 4 ),
 ( 0.000000000000000000, 1.000000000000000000 ),
 .UNSPECIFIED. ) ;
#28200 = CARTESIAN_POINT ( 'NONE',  ( 15.21476480610000159, -100.7776802639999971, 4.291817874450000403 ) ) ;
#28201 = ORIENTED_EDGE ( 'NONE', *, *, #2488, .T. ) ;
#28202 = CARTESIAN_POINT ( 'NONE',  ( 21.37275086740000063, -35.46743101519999897, -7.456866577549999597 ) ) ;
#28203 = DIRECTION ( 'NONE',  ( 0.000000000000000000, 1.000000000000000000, 0.000000000000000000 ) ) ;
#28204 = EDGE_LOOP ( 'NONE', ( #21819, #17195, #27840, #21044 ) ) ;
#28205 = DIRECTION ( 'NONE',  ( 0.000000000000000000, -1.000000000000000000, 0.000000000000000000 ) ) ;
#28206 = ORIENTED_EDGE ( 'NONE', *, *, #27159, .F. ) ;
#28207 = DIRECTION ( 'NONE',  ( -0.2414462220490755373, 0.000000000000000000, 0.9704142011833033488 ) ) ;
#28208 = ADVANCED_FACE ( 'NONE', ( #8022 ), #1304, .F. ) ;
#28209 = CARTESIAN_POINT ( 'NONE',  ( -32.18583505495173114, -74.02375072073509443, -22.07098972207143106 ) ) ;
#28210 = CARTESIAN_POINT ( 'NONE',  ( -40.50000000000000000, -63.30468293320000583, 2.309401076760000393 ) ) ;
#28211 = B_SPLINE_SURFACE_WITH_KNOTS ( 'NONE', 5, 5, ( 
 ( #20781, #2859, #690, #18444, #27330, #9678, #18589, #28173, #21336 ),
 ( #21473, #10646, #3838, #28449, #6156, #19560, #21751, #8484, #28036 ),
 ( #1950, #17386, #15167, #25853, #8206, #1528, #10374, #28302, #8621 ),
 ( #26280, #15028, #12703, #10791, #6301, #24077, #23941, #21618, #4116 ),
 ( #12988, #16965, #8076, #3980, #1803, #14892, #19289, #21897, #19706 ),
 ( #14627, #19149, #28592, #8335, #17238, #17527, #26132, #5745, #5876 ),
 ( #23527, #14754, #3563, #17094, #12839, #12418, #25986, #10506, #1391 ),
 ( #6012, #10235, #1669, #23658, #19420, #3701, #12561, #23803, #22050 ),
 ( #9202, #13135, #6445, #15310, #18115, #19991, #27007, #4414, #4264 ) ),
 .UNSPECIFIED., .F., .F., .F.,
 ( 6, 3, 6 ),
 ( 6, 3, 6 ),
 ( 7.186332009330000048, 18.82032539060000076, 25.08217526979999690 ),
 ( 0.000000000000000000, 0.2500000000000000000, 0.5000000000000000000 ),
 .UNSPECIFIED. ) ;
#28212 = ORIENTED_EDGE ( 'NONE', *, *, #18470, .T. ) ;
#28213 = CYLINDRICAL_SURFACE ( 'NONE', #17597, 1.000000000000000888 ) ;
#28214 = CARTESIAN_POINT ( 'NONE',  ( -12.20497308240000045, -100.9364576079999978, -10.26977901770000123 ) ) ;
#28215 = EDGE_CURVE ( 'NONE', #13014, #23896, #12245, .T. ) ;
#28216 = CARTESIAN_POINT ( 'NONE',  ( 22.87124123144904075, -93.20709273738651746, 15.22480860173989292 ) ) ;
#28217 = CARTESIAN_POINT ( 'NONE',  ( -7.050140110103686908, -101.5829753080988951, 14.41921209752971933 ) ) ;
#28218 = ORIENTED_EDGE ( 'NONE', *, *, #17692, .F. ) ;
#28219 = ADVANCED_FACE ( 'NONE', ( #7888 ), #23163, .T. ) ;
#28220 = CARTESIAN_POINT ( 'NONE',  ( 8.677144207910000517, -37.95796631070000160, -21.92880662259999980 ) ) ;
#28221 = CARTESIAN_POINT ( 'NONE',  ( 16.41935458950000282, -101.1889999979999999, 3.555952033500000109 ) ) ;
#28222 = CARTESIAN_POINT ( 'NONE',  ( 36.47289904670000027, -79.00000000000000000, -14.78463635570000001 ) ) ;
#28223 = ORIENTED_EDGE ( 'NONE', *, *, #8722, .T. ) ;
#28224 = FACE_BOUND ( 'NONE', #21959, .T. ) ;
#28225 = EDGE_LOOP ( 'NONE', ( #13257, #24712 ) ) ;
#28226 = DIRECTION ( 'NONE',  ( 1.000000000000000000, 0.000000000000000000, 0.000000000000000000 ) ) ;
#28227 = CARTESIAN_POINT ( 'NONE',  ( 47.25012594850000625, -74.74525943189999566, -0.5385019865560000119 ) ) ;
#28228 = ORIENTED_EDGE ( 'NONE', *, *, #21327, .F. ) ;
#28229 = CARTESIAN_POINT ( 'NONE',  ( 29.48758676550000146, -92.76843000840000286, 7.141489252159999523 ) ) ;
#28230 = CARTESIAN_POINT ( 'NONE',  ( -7.332335648789999993, -74.23958658489999607, -39.85912817280000553 ) ) ;
#28231 = ORIENTED_EDGE ( 'NONE', *, *, #12697, .T. ) ;
#28232 = CARTESIAN_POINT ( 'NONE',  ( -2.033096837813636260, -98.16872835121394303, -19.54781630589999963 ) ) ;
#28233 = DIRECTION ( 'NONE',  ( 1.000000000000000000, 0.000000000000000000, 0.000000000000000000 ) ) ;
#28234 = CARTESIAN_POINT ( 'NONE',  ( -29.51923111000500199, -92.73901256242717750, -0.4406596607846700042 ) ) ;
#28235 = CARTESIAN_POINT ( 'NONE',  ( -23.24818218629999933, -92.50000942380000879, -18.83198054589999870 ) ) ;
#28236 = CIRCLE ( 'NONE', #12428, 19.50000000000000000 ) ;
#28237 = DIRECTION ( 'NONE',  ( 0.000000000000000000, 1.000000000000000000, 0.000000000000000000 ) ) ;
#28238 = EDGE_LOOP ( 'NONE', ( #25152, #6893, #13097, #19445, #15979 ) ) ;
#28239 = EDGE_CURVE ( 'NONE', #27670, #25484, #26876, .T. ) ;
#28240 = CARTESIAN_POINT ( 'NONE',  ( 25.99900676471481731, -64.47177303794710213, 1.411681790086568355 ) ) ;
#28241 = CARTESIAN_POINT ( 'NONE',  ( 13.69115815750000031, -100.1275643909999928, -9.470476298019999462 ) ) ;
#28242 = CARTESIAN_POINT ( 'NONE',  ( -18.87095359170000108, -92.56168502750000471, 22.85581819720000141 ) ) ;
#28243 = CARTESIAN_POINT ( 'NONE',  ( 23.60984797820000125, -93.86380869110000447, -8.186449766750000023 ) ) ;
#28244 = CARTESIAN_POINT ( 'NONE',  ( 26.69293917519999937, -26.29689110869999880, 48.86109741659999628 ) ) ;
#28245 = CIRCLE ( 'NONE', #27360, 3.000000000000002665 ) ;
#28246 = CARTESIAN_POINT ( 'NONE',  ( 29.87796749985422551, -92.54938211466324560, 6.129015425175801113 ) ) ;
#28247 = FACE_OUTER_BOUND ( 'NONE', #15742, .T. ) ;
#28248 = ORIENTED_EDGE ( 'NONE', *, *, #4237, .T. ) ;
#28249 = ADVANCED_FACE ( 'NONE', ( #1212 ), #4545, .T. ) ;
#28250 = CARTESIAN_POINT ( 'NONE',  ( -5.329070518200000398E-15, -19.50000000000000000, 0.000000000000000000 ) ) ;
#28251 = LINE ( 'NONE', #3794, #8236 ) ;
#28252 = FACE_OUTER_BOUND ( 'NONE', #6810, .T. ) ;
#28253 = CARTESIAN_POINT ( 'NONE',  ( -17.94180966909999597, -19.50000000000000000, 18.81731824139999887 ) ) ;
#28254 = CARTESIAN_POINT ( 'NONE',  ( -13.61185859470209891, -68.68656850711893469, 23.08127642874307028 ) ) ;
#28255 =( NAMED_UNIT ( * ) SI_UNIT ( $, .STERADIAN. ) SOLID_ANGLE_UNIT ( ) );
#28256 = FACE_OUTER_BOUND ( 'NONE', #18149, .T. ) ;
#28257 = VERTEX_POINT ( 'NONE', #14441 ) ;
#28258 = LINE ( 'NONE', #4071, #26587 ) ;
#28259 = CARTESIAN_POINT ( 'NONE',  ( 21.34306235150000219, -35.70901436039999766, -7.836671688740000974 ) ) ;
#28260 = ORIENTED_EDGE ( 'NONE', *, *, #16687, .F. ) ;
#28261 = CIRCLE ( 'NONE', #15222, 38.75000000000000000 ) ;
#28262 = CARTESIAN_POINT ( 'NONE',  ( 21.36168465690000318, -36.64960054550000024, -8.292164435260001909 ) ) ;
#28263 = CARTESIAN_POINT ( 'NONE',  ( 9.107729735749998667, -35.83389485320000034, -19.55231199680000387 ) ) ;
#28264 = VERTEX_POINT ( 'NONE', #28122 ) ;
#28265 = CARTESIAN_POINT ( 'NONE',  ( 9.220169834260000030, -98.40144667389999711, 16.53004056780000042 ) ) ;
#28266 = B_SPLINE_SURFACE_WITH_KNOTS ( 'NONE', 5, 5, ( 
 ( #2779, #20549, #16308, #24923, #18507, #762 ),
 ( #27111, #9748, #27401, #5393, #11934, #7451 ),
 ( #7151, #20986, #20843, #616, #25221, #7594 ),
 ( #468, #13836, #18368, #25068, #14274, #23171 ),
 ( #27255, #7292, #3213, #11486, #20395, #9312 ),
 ( #4953, #10983, #13194, #7105, #6656, #2442 ) ),
 .UNSPECIFIED., .F., .F., .F.,
 ( 6, 6 ),
 ( 6, 6 ),
 ( 28.77370706320000338, 40.74965893960000329 ),
 ( 0.000000000000000000, 2.000000000000000000 ),
 .UNSPECIFIED. ) ;
#28267 = CARTESIAN_POINT ( 'NONE',  ( -2.790536503729999840, -64.24504439390000243, -26.36014981959999659 ) ) ;
#28268 = CARTESIAN_POINT ( 'NONE',  ( -2.813068680090000218, -100.0569316250000043, -17.72190955770000187 ) ) ;
#28269 = ADVANCED_FACE ( 'NONE', ( #12512 ), #23334, .F. ) ;
#28270 = CARTESIAN_POINT ( 'NONE',  ( 7.066909182049999849, -57.47855601759999900, -22.26662627820000040 ) ) ;
#28271 = CARTESIAN_POINT ( 'NONE',  ( -40.42662148796791399, -65.66662781299683616, 2.269983138304441095 ) ) ;
#28272 = EDGE_LOOP ( 'NONE', ( #26427, #3523, #5800, #24728, #26251, #15234, #6030, #28693 ) ) ;
#28273 = EDGE_CURVE ( 'NONE', #9035, #23613, #8717, .T. ) ;
#28274 = AXIS2_PLACEMENT_3D ( 'NONE', #16704, #5494, #20955 ) ;
#28275 = CARTESIAN_POINT ( 'NONE',  ( 13.28061171819887498, -100.9510322836353566, -9.864576516243763749 ) ) ;
#28276 = DIRECTION ( 'NONE',  ( 1.000000000000000000, 0.000000000000000000, 0.000000000000000000 ) ) ;
#28277 = CARTESIAN_POINT ( 'NONE',  ( 24.11323408290000003, -67.98014023149998764, 11.30446450930000069 ) ) ;
#28278 = CARTESIAN_POINT ( 'NONE',  ( 10.08117464879999936, -95.77248565549999171, -19.95701232960000127 ) ) ;
#28279 = EDGE_LOOP ( 'NONE', ( #18519, #3871, #3071, #17896 ) ) ;
#28280 = AXIS2_PLACEMENT_3D ( 'NONE', #8567, #23883, #6093 ) ;
#28281 = CARTESIAN_POINT ( 'NONE',  ( -39.45553247920000217, -74.12472287219999600, 7.440556932039999793 ) ) ;
#28282 = CARTESIAN_POINT ( 'NONE',  ( -40.00000000000000000, -94.00000000000000000, 0.000000000000000000 ) ) ;
#28283 = DIRECTION ( 'NONE',  ( 0.000000000000000000, 0.000000000000000000, -1.000000000000000000 ) ) ;
#28284 = DIRECTION ( 'NONE',  ( 0.000000000000000000, 0.000000000000000000, -1.000000000000000000 ) ) ;
#28285 = ORIENTED_EDGE ( 'NONE', *, *, #15508, .T. ) ;
#28286 = EDGE_CURVE ( 'NONE', #3896, #18698, #27384, .T. ) ;
#28287 = CARTESIAN_POINT ( 'NONE',  ( -1.269269612537524239, -74.18468793103146197, 47.13810727879495488 ) ) ;
#28288 = CARTESIAN_POINT ( 'NONE',  ( 8.986258419809999509, -35.50000000000000000, -19.49544308430000328 ) ) ;
#28289 = CARTESIAN_POINT ( 'NONE',  ( 8.328365334949999976, -63.55534151250000008, -23.20786089210000114 ) ) ;
#28290 = CARTESIAN_POINT ( 'NONE',  ( -12.06225679689999986, -68.93430146459999719, -25.32738640609999692 ) ) ;
#28291 = CARTESIAN_POINT ( 'NONE',  ( 23.29550765120000122, -59.99252585180000352, 10.45228063749999947 ) ) ;
#28292 = CARTESIAN_POINT ( 'NONE',  ( -15.57528087630000080, -80.00000000000000000, 40.61740797039999507 ) ) ;
#28293 = ORIENTED_EDGE ( 'NONE', *, *, #7668, .T. ) ;
#28294 = CARTESIAN_POINT ( 'NONE',  ( 6.684844807969999358, -101.1412505549999992, 14.72083923979999831 ) ) ;
#28295 = CARTESIAN_POINT ( 'NONE',  ( 15.35098429600000003, -101.1417990620000040, 3.558396942789999962 ) ) ;
#28296 = CARTESIAN_POINT ( 'NONE',  ( -34.89999999999999858, -84.50000000000000000, 0.000000000000000000 ) ) ;
#28297 = AXIS2_PLACEMENT_3D ( 'NONE', #20090, #15402, #24316 ) ;
#28298 = CARTESIAN_POINT ( 'NONE',  ( 8.986258609349999205, -35.49999998740000251, -19.49544309740000259 ) ) ;
#28299 = CARTESIAN_POINT ( 'NONE',  ( 22.23400538530000148, -18.50000000000000000, 1.911111031959999984 ) ) ;
#28300 = CARTESIAN_POINT ( 'NONE',  ( -5.767817971120000387, -96.58372172840000758, 20.50849305530000066 ) ) ;
#28301 = VERTEX_POINT ( 'NONE', #17046 ) ;
#28302 = CARTESIAN_POINT ( 'NONE',  ( 3.175154110669999863, -92.54030566109999256, -28.53399386439999930 ) ) ;
#28303 = CARTESIAN_POINT ( 'NONE',  ( 19.90557383419999837, -34.65022531199999634, -8.965967189899998857 ) ) ;
#28304 = CARTESIAN_POINT ( 'NONE',  ( 6.730370301866488880, -101.4085864805377355, 14.71977399093492522 ) ) ;
#28305 = CARTESIAN_POINT ( 'NONE',  ( -6.781378104809999030, -101.5369810359999860, 14.49182221120000058 ) ) ;
#28306 = ORIENTED_EDGE ( 'NONE', *, *, #7185, .T. ) ;
#28307 = CARTESIAN_POINT ( 'NONE',  ( -36.59277592640000165, -74.50000000000000000, -27.40038777100000189 ) ) ;
#28308 = CARTESIAN_POINT ( 'NONE',  ( -12.64133138332632811, -100.8061861236792112, -10.84778541818321607 ) ) ;
#28309 = VERTEX_POINT ( 'NONE', #12929 ) ;
#28310 = CARTESIAN_POINT ( 'NONE',  ( 26.78516883749999877, -92.58502644580001117, -10.10571434189999884 ) ) ;
#28311 = ORIENTED_EDGE ( 'NONE', *, *, #24510, .F. ) ;
#28312 = EDGE_CURVE ( 'NONE', #19001, #27953, #2242, .T. ) ;
#28313 = EDGE_CURVE ( 'NONE', #6421, #10170, #2246, .T. ) ;
#28314 = CARTESIAN_POINT ( 'NONE',  ( -0.8498591013580000242, -101.6484611580000035, -15.97793793410000340 ) ) ;
#28315 = CARTESIAN_POINT ( 'NONE',  ( 22.03468988030000020, -19.46429362099999949, -0.1835573589099999958 ) ) ;
#28316 = DIRECTION ( 'NONE',  ( 0.000000000000000000, 1.000000000000000000, 0.000000000000000000 ) ) ;
#28317 = VECTOR ( 'NONE', #19265, 1000.000000000000000 ) ;
#28318 = DIRECTION ( 'NONE',  ( 0.000000000000000000, -1.000000000000000000, 0.000000000000000000 ) ) ;
#28319 = EDGE_CURVE ( 'NONE', #8501, #14660, #18562, .T. ) ;
#28320 = CYLINDRICAL_SURFACE ( 'NONE', #17281, 57.74999999999999289 ) ;
#28321 = TOROIDAL_SURFACE ( 'NONE', #22775, 21.14285714289999873, 0.5000000000000000000 ) ;
#28322 = CIRCLE ( 'NONE', #19934, 34.89999999999999858 ) ;
#28323 = CARTESIAN_POINT ( 'NONE',  ( -22.57449023189999693, -71.67452784319999637, 17.69693788339999685 ) ) ;
#28324 = AXIS2_PLACEMENT_3D ( 'NONE', #17207, #10478, #2068 ) ;
#28325 = B_SPLINE_CURVE_WITH_KNOTS ( 'NONE', 5,
 ( #9323, #4521, #4670, #24790, #4828, #10903, #24487, #2502, #13253 ),
 .UNSPECIFIED., .F., .F.,
 ( 6, 3, 6 ),
 ( 0.000000000000000000, 0.5000000000000000000, 1.000000000000000000 ),
 .UNSPECIFIED. ) ;
#28326 = CARTESIAN_POINT ( 'NONE',  ( 24.73953371475964147, -92.49999918154817635, 14.89633460343937799 ) ) ;
#28327 = CARTESIAN_POINT ( 'NONE',  ( 7.939780906490000234, -101.1889999979999999, 14.74863990870000130 ) ) ;
#28328 = CARTESIAN_POINT ( 'NONE',  ( 6.846103682120000755, -36.12241484350000320, -21.55427193710000111 ) ) ;
#28329 = CARTESIAN_POINT ( 'NONE',  ( 0.000000000000000000, -15.00000000000000000, 52.35000000000000142 ) ) ;
#28330 = ORIENTED_EDGE ( 'NONE', *, *, #19241, .F. ) ;
#28331 = CARTESIAN_POINT ( 'NONE',  ( 7.765654448670000320, -18.50000000000000000, -19.88144340339999872 ) ) ;
#28332 = ORIENTED_EDGE ( 'NONE', *, *, #10628, .T. ) ;
#28333 = DIRECTION ( 'NONE',  ( 0.000000000000000000, 1.000000000000000000, 0.000000000000000000 ) ) ;
#28334 = ADVANCED_FACE ( 'NONE', ( #1896 ), #10883, .F. ) ;
#28335 = CARTESIAN_POINT ( 'NONE',  ( -2.698605191359999544, -63.31646347429999366, -26.06520130500000221 ) ) ;
#28336 = AXIS2_PLACEMENT_3D ( 'NONE', #26109, #3820, #16945 ) ;
#28337 = DIRECTION ( 'NONE',  ( 0.000000000000000000, 1.000000000000000000, 0.000000000000000000 ) ) ;
#28338 = CARTESIAN_POINT ( 'NONE',  ( -41.75000000000000000, -63.07912966450000880, -2.684678751739999925 ) ) ;
#28339 = CARTESIAN_POINT ( 'NONE',  ( -20.45998242170000125, -52.56313962710000709, 14.78974999389999923 ) ) ;
#28340 = AXIS2_PLACEMENT_3D ( 'NONE', #25462, #3454, #1420 ) ;
#28341 = AXIS2_PLACEMENT_3D ( 'NONE', #26837, #9328, #11362 ) ;
#28342 = AXIS2_PLACEMENT_3D ( 'NONE', #25004, #16552, #27495 ) ;
#28343 = ORIENTED_EDGE ( 'NONE', *, *, #11528, .T. ) ;
#28344 = CARTESIAN_POINT ( 'NONE',  ( 47.25000000000000000, -73.00000000000000000, 2.433892081919999696E-15 ) ) ;
#28345 = CARTESIAN_POINT ( 'NONE',  ( 7.102042752109999135, -101.1889999979999999, 14.33739825589999839 ) ) ;
#28346 = ORIENTED_EDGE ( 'NONE', *, *, #20275, .T. ) ;
#28347 = CYLINDRICAL_SURFACE ( 'NONE', #1059, 0.9999999999999990008 ) ;
#28348 = ADVANCED_FACE ( 'NONE', ( #26224 ), #12893, .T. ) ;
#28349 = DIRECTION ( 'NONE',  ( 0.000000000000000000, -1.000000000000000000, 0.000000000000000000 ) ) ;
#28350 = CARTESIAN_POINT ( 'NONE',  ( 22.42985924190000091, -18.87168151170000030, 9.783895484440000345 ) ) ;
#28351 = FACE_OUTER_BOUND ( 'NONE', #8447, .T. ) ;
#28352 = CARTESIAN_POINT ( 'NONE',  ( -19.90266458450000187, -57.44036972699999666, 14.20824301549999902 ) ) ;
#28353 = ORIENTED_EDGE ( 'NONE', *, *, #26480, .F. ) ;
#28354 = CARTESIAN_POINT ( 'NONE',  ( 23.93802380909999883, -64.72767011149998950, -9.438994838039999280 ) ) ;
#28355 = CARTESIAN_POINT ( 'NONE',  ( -11.98370860700000051, -101.2530993010000060, -9.340542411159999503 ) ) ;
#28356 = CARTESIAN_POINT ( 'NONE',  ( -7.898777529207614556, -100.4010812938397521, 15.03135312487839137 ) ) ;
#28357 = ORIENTED_EDGE ( 'NONE', *, *, #24293, .T. ) ;
#28358 = CIRCLE ( 'NONE', #2793, 0.5000000000000008882 ) ;
#28359 = VECTOR ( 'NONE', #5162, 999.9999999999998863 ) ;
#28360 = DIRECTION ( 'NONE',  ( 0.000000000000000000, -1.000000000000000000, 0.000000000000000000 ) ) ;
#28361 = CARTESIAN_POINT ( 'NONE',  ( -32.59032919970000108, -74.28456446479999897, -21.87590318590000038 ) ) ;
#28362 = CARTESIAN_POINT ( 'NONE',  ( 37.29611236860000645, -79.99999990109998294, -13.74999974979999884 ) ) ;
#28363 = VERTEX_POINT ( 'NONE', #10736 ) ;
#28364 = EDGE_CURVE ( 'NONE', #2148, #16095, #20299, .T. ) ;
#28365 = CARTESIAN_POINT ( 'NONE',  ( 6.982153158335030696, -100.1517898586307496, 15.69801493785662849 ) ) ;
#28366 = CARTESIAN_POINT ( 'NONE',  ( -0.8787802303807957793, -79.83340751218206321, 47.19654850980432315 ) ) ;
#28367 = ORIENTED_EDGE ( 'NONE', *, *, #27147, .T. ) ;
#28368 = CARTESIAN_POINT ( 'NONE',  ( -29.47186832370000076, -93.00000450890000536, -0.4149655844399999793 ) ) ;
#28369 = DIRECTION ( 'NONE',  ( -0.09756097560976770278, 0.000000000000000000, -0.9952295494196654602 ) ) ;
#28370 = VERTEX_POINT ( 'NONE', #13085 ) ;
#28371 = CARTESIAN_POINT ( 'NONE',  ( 21.54084985340000102, -53.82492386869999734, 10.13856859999999926 ) ) ;
#28372 = DIRECTION ( 'NONE',  ( 0.9952295494196655712, 0.000000000000000000, 0.09756097560976655092 ) ) ;
#28373 = CARTESIAN_POINT ( 'NONE',  ( -5.969238273219999336, -101.2530993000000024, 13.97222956260000082 ) ) ;
#28374 = ADVANCED_FACE ( 'NONE', ( #4502 ), #23642, .F. ) ;
#28375 = ORIENTED_EDGE ( 'NONE', *, *, #8190, .F. ) ;
#28376 = AXIS2_PLACEMENT_3D ( 'NONE', #26003, #23963, #1550 ) ;
#28377 = CARTESIAN_POINT ( 'NONE',  ( -41.75000000000000000, -63.30468293320000583, 1.587713240270000048 ) ) ;
#28378 = DIRECTION ( 'NONE',  ( 0.000000000000000000, -1.000000000000000000, 0.000000000000000000 ) ) ;
#28379 = TOROIDAL_SURFACE ( 'NONE', #19084, 55.85192378860000417, 0.3499999999999999778 ) ;
#28380 = CARTESIAN_POINT ( 'NONE',  ( -21.60034894820000062, -79.50000026560000776, -32.77174736439999947 ) ) ;
#28381 = CARTESIAN_POINT ( 'NONE',  ( -18.93875617240000153, -93.07693985719998864, -21.17499315530000104 ) ) ;
#28382 = CARTESIAN_POINT ( 'NONE',  ( 24.22382764319999993, -64.24504439390000243, 10.76339940740000145 ) ) ;
#28383 = ORIENTED_EDGE ( 'NONE', *, *, #742, .T. ) ;
#28384 = DIRECTION ( 'NONE',  ( 0.4794255386042038936, 0.000000000000000000, 0.8775825618903723147 ) ) ;
#28385 = CARTESIAN_POINT ( 'NONE',  ( 13.59944669439999920, -100.1512121650000040, -9.587914801669999321 ) ) ;
#28386 = CARTESIAN_POINT ( 'NONE',  ( 25.14694229440000228, -65.07443093669999712, -0.3759436444569999591 ) ) ;
#28387 = DIRECTION ( 'NONE',  ( 0.000000000000000000, -1.000000000000000000, 0.000000000000000000 ) ) ;
#28388 = CARTESIAN_POINT ( 'NONE',  ( 10.77859369565145897, -72.53894543248756577, -26.82390758811301623 ) ) ;
#28389 = CARTESIAN_POINT ( 'NONE',  ( 0.3872056760440000245, -101.1889999979999999, -17.35614698070000017 ) ) ;
#28390 = VERTEX_POINT ( 'NONE', #8428 ) ;
#28391 = PLANE ( 'NONE',  #23461 ) ;
#28392 = CARTESIAN_POINT ( 'NONE',  ( 8.793068625647139314, -37.96202148991682890, -22.01683846075131967 ) ) ;
#28393 = DIRECTION ( 'NONE',  ( 0.000000000000000000, 1.000000000000000000, 0.000000000000000000 ) ) ;
#28394 = DIRECTION ( 'NONE',  ( 1.000000000000000000, 0.000000000000000000, -1.261617073437678048E-15 ) ) ;
#28395 = CARTESIAN_POINT ( 'NONE',  ( -0.1180621203445222367, -92.72059904818335951, -30.49977178675158029 ) ) ;
#28396 = VECTOR ( 'NONE', #314, 1000.000000000000000 ) ;
#28397 = CIRCLE ( 'NONE', #14893, 39.75000000000000000 ) ;
#28398 = AXIS2_PLACEMENT_3D ( 'NONE', #10634, #21740, #6144 ) ;
#28399 = ADVANCED_FACE ( 'NONE', ( #15114 ), #11523, .F. ) ;
#28400 = EDGE_CURVE ( 'NONE', #24581, #7391, #4061, .T. ) ;
#28401 = ORIENTED_EDGE ( 'NONE', *, *, #25959, .F. ) ;
#28402 = CARTESIAN_POINT ( 'NONE',  ( 20.72386479999999764, -35.83655893530000469, -8.803829908180000885 ) ) ;
#28403 = ORIENTED_EDGE ( 'NONE', *, *, #19731, .T. ) ;
#28404 = CARTESIAN_POINT ( 'NONE',  ( 19.56129018700000088, -35.88702891199999812, -9.158871637020000733 ) ) ;
#28405 = DIRECTION ( 'NONE',  ( 1.000000000000000000, 0.000000000000000000, 0.000000000000000000 ) ) ;
#28406 = EDGE_CURVE ( 'NONE', #5383, #10466, #13371, .T. ) ;
#28407 = EDGE_LOOP ( 'NONE', ( #5058, #2133, #23330, #10349, #11600 ) ) ;
#28408 = CARTESIAN_POINT ( 'NONE',  ( 11.96443931099999958, -96.83683775170000274, 17.18597302079999878 ) ) ;
#28409 = ADVANCED_FACE ( 'NONE', ( #8705 ), #6889, .F. ) ;
#28410 = CARTESIAN_POINT ( 'NONE',  ( -14.12278956529999974, -93.04972065580000162, -23.64156151090000080 ) ) ;
#28411 = CARTESIAN_POINT ( 'NONE',  ( -0.5658552861894227126, -18.49999996075941411, -21.28277172089477887 ) ) ;
#28412 = CARTESIAN_POINT ( 'NONE',  ( 0.000000000000000000, -16.50000000000000000, 0.000000000000000000 ) ) ;
#28413 = CARTESIAN_POINT ( 'NONE',  ( 7.215414233289999757, -74.50000000000000000, -40.70731707320000226 ) ) ;
#28414 = CARTESIAN_POINT ( 'NONE',  ( 7.675802715190000569, -57.47600051900000295, -22.13628143409999893 ) ) ;
#28415 = CARTESIAN_POINT ( 'NONE',  ( -11.08724219600000183, -18.85485920039999996, -18.88147462500000273 ) ) ;
#28416 = CIRCLE ( 'NONE', #8396, 7.250000000000000000 ) ;
#28417 = CARTESIAN_POINT ( 'NONE',  ( 0.000000000000000000, -107.5000000000000000, 0.000000000000000000 ) ) ;
#28418 = ORIENTED_EDGE ( 'NONE', *, *, #15047, .F. ) ;
#28419 = AXIS2_PLACEMENT_3D ( 'NONE', #6331, #26447, #23681 ) ;
#28420 = CARTESIAN_POINT ( 'NONE',  ( 13.59220273991967609, -100.4872618013039158, -10.06240860112436941 ) ) ;
#28421 = AXIS2_PLACEMENT_3D ( 'NONE', #5715, #3541, #23502 ) ;
#28422 = CARTESIAN_POINT ( 'NONE',  ( 22.78606152149999886, -34.66500525210000205, 0.4244034508280000173 ) ) ;
#28423 = CARTESIAN_POINT ( 'NONE',  ( 24.61976394740000273, -69.66720773109999243, 11.67393097119999901 ) ) ;
#28424 = CARTESIAN_POINT ( 'NONE',  ( 9.273496252050001942, -94.57749834670001121, -22.35125233299999792 ) ) ;
#28425 = ORIENTED_EDGE ( 'NONE', *, *, #13200, .T. ) ;
#28426 = CARTESIAN_POINT ( 'NONE',  ( -40.70731707320000226, -74.50000000000000000, 7.215414233289999757 ) ) ;
#28427 = AXIS2_PLACEMENT_3D ( 'NONE', #7713, #14112, #21110 ) ;
#28428 = DIRECTION ( 'NONE',  ( 0.000000000000000000, -1.000000000000000000, 0.000000000000000000 ) ) ;
#28429 = CARTESIAN_POINT ( 'NONE',  ( -0.5856201115350000430, -19.46363745430000236, -22.02586699820000149 ) ) ;
#28430 = CARTESIAN_POINT ( 'NONE',  ( 4.037078284719999375E-15, -74.00000000000000000, -40.00000000000000000 ) ) ;
#28431 = ORIENTED_EDGE ( 'NONE', *, *, #17942, .F. ) ;
#28432 = CARTESIAN_POINT ( 'NONE',  ( 26.13146017414465305, -67.22652123492960641, -0.08258631501461731472 ) ) ;
#28433 = DIRECTION ( 'NONE',  ( 0.000000000000000000, 1.000000000000000000, 0.000000000000000000 ) ) ;
#28434 = CARTESIAN_POINT ( 'NONE',  ( 9.160187750109999527, -60.39422136570000532, -22.93664085480000381 ) ) ;
#28435 = CARTESIAN_POINT ( 'NONE',  ( -12.45933098930000149, -68.79094677780000211, -23.93918507130000251 ) ) ;
#28436 = CARTESIAN_POINT ( 'NONE',  ( 21.63571321169999706, -57.45864736019999697, 10.20337583880000132 ) ) ;
#28437 = CARTESIAN_POINT ( 'NONE',  ( -12.17175116130000134, -57.47855602620000326, -19.93971707270000238 ) ) ;
#28438 = VERTEX_POINT ( 'NONE', #24176 ) ;
#28439 = CIRCLE ( 'NONE', #24737, 1.999999999999999334 ) ;
#28440 = CARTESIAN_POINT ( 'NONE',  ( 7.181689937160000703, -99.92967571559999840, 15.80535030819999953 ) ) ;
#28441 = CARTESIAN_POINT ( 'NONE',  ( 15.72706581430000128, -101.2251655520000071, 3.980808227969999447 ) ) ;
#28442 = CIRCLE ( 'NONE', #1475, 3.499999999999999556 ) ;
#28443 = EDGE_CURVE ( 'NONE', #15667, #1954, #20378, .T. ) ;
#28444 = ORIENTED_EDGE ( 'NONE', *, *, #20364, .T. ) ;
#28445 = DIRECTION ( 'NONE',  ( -8.326672684689999093E-17, 0.000000000000000000, -1.000000000000000000 ) ) ;
#28446 = CARTESIAN_POINT ( 'NONE',  ( 6.008696179649185787, -92.50638022835023833, -29.90261591053662471 ) ) ;
#28447 = CARTESIAN_POINT ( 'NONE',  ( -42.01869634261938558, -65.72281118314606374, -0.9050793633985121378 ) ) ;
#28448 = ORIENTED_EDGE ( 'NONE', *, *, #6726, .F. ) ;
#28449 = CARTESIAN_POINT ( 'NONE',  ( 1.937685342960000057, -92.76004107139999633, -29.70233978819999976 ) ) ;
#28450 = ADVANCED_FACE ( 'NONE', ( #4806 ), #18543, .T. ) ;
#28451 = B_SPLINE_SURFACE_WITH_KNOTS ( 'NONE', 5, 5, ( 
 ( #5586, #8315, #6135, #23510, #28154, #23638, #23366, #27871, #5723 ),
 ( #16803, #10215, #15009, #25696, #3547, #19129, #28018, #25967, #8056 ),
 ( #8187, #23779, #12684, #21593, #10488, #13264, #4245, #13117, #8889 ),
 ( #20272, #21878, #4682, #9042, #12964, #6282, #24356, #24653, #4396 ),
 ( #13563, #22469, #22172, #11216, #26539, #2513, #26842, #1931, #11368 ),
 ( #340, #8740, #15148, #26693, #24498, #19683, #24056, #6734, #2212 ),
 ( #4096, #17948, #6582, #22029, #15443, #9183, #20124, #10770, #2077 ),
 ( #15599, #17509, #28572, #28700, #8607, #41, #26394, #17802, #17657 ),
 ( #6424, #15287, #26260, #24209, #10916, #19824, #11055, #19971, #4531 ) ),
 .UNSPECIFIED., .F., .F., .F.,
 ( 6, 3, 6 ),
 ( 6, 3, 6 ),
 ( 54.97253517989999949, 63.48927009810000044, 72.86859331460000533 ),
 ( 0.000000000000000000, 0.2500000000000000000, 0.5000000000000000000 ),
 .UNSPECIFIED. ) ;
#28452 = CARTESIAN_POINT ( 'NONE',  ( 6.877703509944694815, -101.5829753080977298, 14.50225318756008974 ) ) ;
#28453 = CARTESIAN_POINT ( 'NONE',  ( -6.729715370570000132, -101.1284992150000051, 13.85798327430000043 ) ) ;
#28454 = EDGE_LOOP ( 'NONE', ( #242, #11747, #25070, #20209 ) ) ;
#28455 = LINE ( 'NONE', #23807, #21349 ) ;
#28456 = VERTEX_POINT ( 'NONE', #16300 ) ;
#28457 = CARTESIAN_POINT ( 'NONE',  ( 8.670860352240000068, -36.23359953109999765, -21.01414488289999838 ) ) ;
#28458 = CARTESIAN_POINT ( 'NONE',  ( 24.64041555829999908, -93.75379239679999444, -3.870821881539999954 ) ) ;
#28459 = CARTESIAN_POINT ( 'NONE',  ( 11.24690583532123256, -93.66270333200120035, -23.43420612766421485 ) ) ;
#28460 = AXIS2_PLACEMENT_3D ( 'NONE', #28630, #22092, #4454 ) ;
#28461 = CARTESIAN_POINT ( 'NONE',  ( 22.46071958670000157, -18.85738404119999956, 1.064556727120000046 ) ) ;
#28462 = CARTESIAN_POINT ( 'NONE',  ( -43.29972737720588327, -63.05366291736145001, 0.03679144966651182874 ) ) ;
#28463 = CARTESIAN_POINT ( 'NONE',  ( -20.71870563330397275, -92.77481473461477890, -22.38281498381969925 ) ) ;
#28464 = ORIENTED_EDGE ( 'NONE', *, *, #27910, .T. ) ;
#28465 = DIRECTION ( 'NONE',  ( 0.000000000000000000, -1.000000000000000000, 0.000000000000000000 ) ) ;
#28466 = AXIS2_PLACEMENT_3D ( 'NONE', #13081, #21696, #2038 ) ;
#28467 = CARTESIAN_POINT ( 'NONE',  ( -7.615241770509999806E-12, -84.00000000000000000, -9.798384326129999571E-12 ) ) ;
#28468 = CARTESIAN_POINT ( 'NONE',  ( -36.78600833567148953, -65.14196057590905298, 0.1651269895895124684 ) ) ;
#28469 = CARTESIAN_POINT ( 'NONE',  ( 23.96368475870000125, -92.50000000000000000, 8.717328305520000598 ) ) ;
#28470 = CARTESIAN_POINT ( 'NONE',  ( -18.54060892918908721, -19.47131810279708830, 13.04730683233061583 ) ) ;
#28471 = CARTESIAN_POINT ( 'NONE',  ( 7.664900609720000091, -35.15980160819999867, -21.28729237769999827 ) ) ;
#28472 = FACE_BOUND ( 'NONE', #21175, .T. ) ;
#28473 = EDGE_LOOP ( 'NONE', ( #19537, #14863, #8127, #20293 ) ) ;
#28474 = CARTESIAN_POINT ( 'NONE',  ( 7.730596112549999788, -19.15810972889999775, -20.62158084869999897 ) ) ;
#28475 = CARTESIAN_POINT ( 'NONE',  ( 22.96193664180000127, -37.37167648650000018, -9.452942635470000354 ) ) ;
#28476 = ADVANCED_FACE ( 'NONE', ( #11783 ), #9683, .F. ) ;
#28477 = ORIENTED_EDGE ( 'NONE', *, *, #27465, .F. ) ;
#28478 = B_SPLINE_CURVE_WITH_KNOTS ( 'NONE', 3,
 ( #4141, #6475, #22074, #6628, #85, #26881, #4727, #8786, #17698, #15489, #24399, #4436, #8935, #6920, #2257, #24538, #19727, #13607, #13166, #17845, #9086, #11103, #20016, #19866, #15786, #2121, #15336, #24253, #4292, #13306, #26742, #22211, #6777, #22515, #4579, #13458, #11409 ),
 .UNSPECIFIED., .F., .F.,
 ( 4, 2, 2, 1, 1, 1, 2, 2, 2, 2, 1, 1, 1, 2, 2, 2, 2, 1, 1, 1, 2, 2, 4 ),
 ( 0.000000000000000000, 0.1250000000000152656, 0.1875000000000219269, 0.2187500000000252576, 0.2343750000000270339, 0.2421875000000283662, 0.2460937500000285050, 0.2500000000000286438, 0.3750000000000290323, 0.4375000000000291434, 0.4687500000000289213, 0.4843750000000290878, 0.4921875000000295874, 0.4960937500000296985, 0.5000000000000298650, 0.6250000000000226485, 0.6875000000000187628, 0.7187500000000167644, 0.7343750000000157652, 0.7421875000000152101, 0.7460937500000150990, 0.7500000000000148770, 1.000000000000000000 ),
 .UNSPECIFIED. ) ;
#28479 = AXIS2_PLACEMENT_3D ( 'NONE', #10100, #19671, #24045 ) ;
#28480 = CARTESIAN_POINT ( 'NONE',  ( -1.447122895489999950, -60.30889230620000063, -23.76394779129999790 ) ) ;
#28481 = CARTESIAN_POINT ( 'NONE',  ( 9.063914967340000572, -37.97325489250000174, -22.27494422110000016 ) ) ;
#28482 = DIRECTION ( 'NONE',  ( 0.000000000000000000, 1.000000000000000000, 0.000000000000000000 ) ) ;
#28483 = AXIS2_PLACEMENT_3D ( 'NONE', #10369, #19285, #28170 ) ;
#28484 = FACE_OUTER_BOUND ( 'NONE', #17636, .T. ) ;
#28485 = EDGE_CURVE ( 'NONE', #6598, #12283, #19270, .T. ) ;
#28486 = ORIENTED_EDGE ( 'NONE', *, *, #9296, .F. ) ;
#28487 = CARTESIAN_POINT ( 'NONE',  ( 21.18684992340000051, -34.75995393510000042, -7.793340637920000091 ) ) ;
#28488 = CARTESIAN_POINT ( 'NONE',  ( 7.135466514619999145, -73.65708014139998738, -38.71640952649999434 ) ) ;
#28489 = ORIENTED_EDGE ( 'NONE', *, *, #18509, .T. ) ;
#28490 = FACE_OUTER_BOUND ( 'NONE', #1206, .T. ) ;
#28491 = CARTESIAN_POINT ( 'NONE',  ( 19.71712935880000117, -26.09894693429999890, 10.34883699620000108 ) ) ;
#28492 = CARTESIAN_POINT ( 'NONE',  ( -7.498699138939999287, -94.79581646409999962, -22.45487619560000070 ) ) ;
#28493 = CARTESIAN_POINT ( 'NONE',  ( 21.60905208779999853, -19.48534420260000033, 9.488781546969999425 ) ) ;
#28494 = CARTESIAN_POINT ( 'NONE',  ( -20.30783661097642678, -96.61062616337834186, -6.202245570597845870 ) ) ;
#28495 = CARTESIAN_POINT ( 'NONE',  ( -13.14229091329999832, -100.8869817940000075, -8.528547626079999944 ) ) ;
#28496 = EDGE_CURVE ( 'NONE', #5829, #8703, #20694, .T. ) ;
#28497 = VERTEX_POINT ( 'NONE', #2632 ) ;
#28498 = AXIS2_PLACEMENT_3D ( 'NONE', #18038, #13217, #22125 ) ;
#28499 = CARTESIAN_POINT ( 'NONE',  ( 16.08037959500000014, -101.1889999979999999, 2.354223078750000031 ) ) ;
#28500 = CARTESIAN_POINT ( 'NONE',  ( -11.76437930720000047, -100.8023006570000035, -10.51170590289999929 ) ) ;
#28501 = AXIS2_PLACEMENT_3D ( 'NONE', #1838, #6639, #28759 ) ;
#28502 = CARTESIAN_POINT ( 'NONE',  ( -7.701451075213345376, -100.9229461894397843, 14.66641892369707278 ) ) ;
#28503 = VERTEX_POINT ( 'NONE', #459 ) ;
#28504 = CARTESIAN_POINT ( 'NONE',  ( 11.51925138921799352, -70.92537290725283583, -27.02474293696387520 ) ) ;
#28505 = CARTESIAN_POINT ( 'NONE',  ( -32.47291160230000173, -74.11800272920001476, -21.73792012110000016 ) ) ;
#28506 = CARTESIAN_POINT ( 'NONE',  ( 36.75261502460000429, -80.49999978700000725, -13.77875165610000074 ) ) ;
#28507 = VERTEX_POINT ( 'NONE', #25058 ) ;
#28508 = ADVANCED_FACE ( 'NONE', ( #5092 ), #8505, .T. ) ;
#28509 = PRODUCT_DEFINITION_SHAPE ( 'NONE', 'NONE',  #28807 ) ;
#28510 = CONICAL_SURFACE ( 'NONE', #6177, 55.67692378859999280, 1.047197551199999799 ) ;
#28511 = CARTESIAN_POINT ( 'NONE',  ( -30.31271238969999970, -92.50000000000000000, 0.1252161350790000072 ) ) ;
#28512 = CARTESIAN_POINT ( 'NONE',  ( 19.92559242949999998, -35.99861502429999405, -9.426072644010000445 ) ) ;
#28513 = CARTESIAN_POINT ( 'NONE',  ( 12.03044342970000002, -92.63020460699999603, 27.45853671740000124 ) ) ;
#28514 = VERTEX_POINT ( 'NONE', #5387 ) ;
#28515 = EDGE_CURVE ( 'NONE', #4628, #21477, #20856, .T. ) ;
#28516 = DIRECTION ( 'NONE',  ( -1.000000000000000000, 0.000000000000000000, -5.551115123129999410E-17 ) ) ;
#28517 = CARTESIAN_POINT ( 'NONE',  ( -19.83822443902547050, -96.11102763504688085, 9.124294855013181049 ) ) ;
#28518 = ORIENTED_EDGE ( 'NONE', *, *, #21102, .T. ) ;
#28519 = CARTESIAN_POINT ( 'NONE',  ( -43.20000000000000284, -65.14977478849999670, -0.1732050807570000017 ) ) ;
#28520 = CARTESIAN_POINT ( 'NONE',  ( -14.86197364899999940, -100.8869795979999964, 4.957594172660000353 ) ) ;
#28521 = ORIENTED_EDGE ( 'NONE', *, *, #24039, .T. ) ;
#28522 = VECTOR ( 'NONE', #9137, 1000.000000000000000 ) ;
#28523 = CARTESIAN_POINT ( 'NONE',  ( -34.47145558279999733, -74.50000000000000000, -23.86485386499999706 ) ) ;
#28524 = DIRECTION ( 'NONE',  ( 0.000000000000000000, 1.000000000000000000, 0.000000000000000000 ) ) ;
#28525 = CARTESIAN_POINT ( 'NONE',  ( -22.17563740510000159, -80.50000000000000000, -32.38675284270000532 ) ) ;
#28526 = CARTESIAN_POINT ( 'NONE',  ( -23.49132533670000100, -92.92146929989999649, -19.26888038349999732 ) ) ;
#28527 = CARTESIAN_POINT ( 'NONE',  ( 25.16030248577766670, -66.99910240652532423, 10.87945431192736301 ) ) ;
#28528 = ORIENTED_EDGE ( 'NONE', *, *, #20744, .T. ) ;
#28529 = CARTESIAN_POINT ( 'NONE',  ( -6.065234971653478802, -101.5839620086842388, 14.85812437776191963 ) ) ;
#28530 = CARTESIAN_POINT ( 'NONE',  ( 13.74656640350000103, -99.97545561319999763, -9.830828057420001542 ) ) ;
#28531 = CARTESIAN_POINT ( 'NONE',  ( -18.75664408759999802, -92.68584073459999217, 22.80736227010000050 ) ) ;
#28532 = ADVANCED_FACE ( 'NONE', ( #7988 ), #14810, .T. ) ;
#28533 = DIRECTION ( 'NONE',  ( 0.000000000000000000, 1.000000000000000000, 0.000000000000000000 ) ) ;
#28534 = TOROIDAL_SURFACE ( 'NONE', #7162, 55.85192378860000417, 0.3499999999999999778 ) ;
#28535 = CARTESIAN_POINT ( 'NONE',  ( 10.94782719350765632, -72.47277773194394968, -26.85191487759274409 ) ) ;
#28536 = DIRECTION ( 'NONE',  ( 0.000000000000000000, 1.000000000000000000, 0.000000000000000000 ) ) ;
#28537 = EDGE_LOOP ( 'NONE', ( #8042, #5251, #20217, #28670 ) ) ;
#28538 = DIRECTION ( 'NONE',  ( -0.3422283636740854340, -0.7003189540771749266, -0.6264448177271558782 ) ) ;
#28539 = CARTESIAN_POINT ( 'NONE',  ( 8.408333318189998979E-15, -74.00000000000000000, 40.00000000000000000 ) ) ;
#28540 = CARTESIAN_POINT ( 'NONE',  ( -24.15983059781524389, -92.58347372262571184, -18.61592446762897879 ) ) ;
#28541 = CARTESIAN_POINT ( 'NONE',  ( 14.05983645159999895, -99.53431386179998697, -10.27466725399999881 ) ) ;
#28542 = EDGE_CURVE ( 'NONE', #22471, #21436, #16117, .T. ) ;
#28543 = CARTESIAN_POINT ( 'NONE',  ( -0.8786661444248782260, -92.52249206705035078, -30.48734580142448536 ) ) ;
#28544 = CIRCLE ( 'NONE', #11343, 57.75000000000000000 ) ;
#28545 = APPLICATION_PROTOCOL_DEFINITION ( 'draft international standard', 'automotive_design', 1998, #16864 ) ;
#28546 = CARTESIAN_POINT ( 'NONE',  ( 0.000000000000000000, -102.5000000000000000, 0.000000000000000000 ) ) ;
#28547 = EDGE_LOOP ( 'NONE', ( #1654, #15875, #19554, #2887 ) ) ;
#28548 = AXIS2_PLACEMENT_3D ( 'NONE', #8855, #4361, #15410 ) ;
#28549 = CARTESIAN_POINT ( 'NONE',  ( 21.19481781799999709, -97.14975610550000340, -2.160707968160000103 ) ) ;
#28550 = ORIENTED_EDGE ( 'NONE', *, *, #18163, .T. ) ;
#28551 = CIRCLE ( 'NONE', #4374, 1.249999999999999112 ) ;
#28552 = CARTESIAN_POINT ( 'NONE',  ( 21.42228108240000140, -36.78979570469999771, -8.360528863789999932 ) ) ;
#28553 = DIRECTION ( 'NONE',  ( 1.000000000000000000, 0.000000000000000000, 0.000000000000000000 ) ) ;
#28554 = VERTEX_POINT ( 'NONE', #25770 ) ;
#28555 = CARTESIAN_POINT ( 'NONE',  ( 8.472395020760000506, -37.95144078679999922, -21.79230213740000011 ) ) ;
#28556 = CARTESIAN_POINT ( 'NONE',  ( -13.14595372920000038, -93.06132229930000221, -23.62747770269999847 ) ) ;
#28557 = DIRECTION ( 'NONE',  ( 0.000000000000000000, 1.000000000000000000, 0.000000000000000000 ) ) ;
#28558 = CARTESIAN_POINT ( 'NONE',  ( 8.188637977920000921, -100.9197082849999987, 13.30686163390000054 ) ) ;
#28559 = CARTESIAN_POINT ( 'NONE',  ( -30.40445704718852227, -92.82044061123613687, 2.412276836114850553 ) ) ;
#28560 = CARTESIAN_POINT ( 'NONE',  ( 8.496651354449999971, -44.91471497059999507, -21.93056824609999822 ) ) ;
#28561 = AXIS2_PLACEMENT_3D ( 'NONE', #2805, #20123, #192 ) ;
#28562 = CARTESIAN_POINT ( 'NONE',  ( -11.41039530250000134, -19.15810975349999978, -18.83652256670000114 ) ) ;
#28563 = CARTESIAN_POINT ( 'NONE',  ( -40.28472764600749656, -65.70971443685482427, 2.216654594839819303 ) ) ;
#28564 = VERTEX_POINT ( 'NONE', #27951 ) ;
#28565 = CARTESIAN_POINT ( 'NONE',  ( 13.63352270484119977, -100.4103893717064437, -10.10970819179740587 ) ) ;
#28566 = CARTESIAN_POINT ( 'NONE',  ( 22.11862230030000021, -19.46485671829999831, 0.2283802166510000287 ) ) ;
#28567 = CARTESIAN_POINT ( 'NONE',  ( 24.39287928049999721, -64.76590626969999676, 10.80146537900000148 ) ) ;
#28568 = CARTESIAN_POINT ( 'NONE',  ( 39.06010443568764856, -73.53996501802137686, 7.188997797742533891 ) ) ;
#28569 = ORIENTED_EDGE ( 'NONE', *, *, #13926, .F. ) ;
#28570 = ADVANCED_FACE ( 'NONE', ( #1044 ), #24556, .F. ) ;
#28571 = DIRECTION ( 'NONE',  ( 0.000000000000000000, -1.000000000000000000, 0.000000000000000000 ) ) ;
#28572 = CARTESIAN_POINT ( 'NONE',  ( -14.17503812420000031, -92.50889039439999806, 25.96392922189999908 ) ) ;
#28573 = CARTESIAN_POINT ( 'NONE',  ( -20.62204820664130978, -93.91746156109596200, 13.70703326616601636 ) ) ;
#28574 = ORIENTED_EDGE ( 'NONE', *, *, #4741, .T. ) ;
#28575 = EDGE_CURVE ( 'NONE', #134, #3865, #24477, .T. ) ;
#28576 = CARTESIAN_POINT ( 'NONE',  ( 25.64005057298560786, -66.15241698523519176, -0.2567751734516250939 ) ) ;
#28577 = CARTESIAN_POINT ( 'NONE',  ( 0.7851461961000000267, -99.77922884479998800, -17.12662525980000083 ) ) ;
#28578 = CARTESIAN_POINT ( 'NONE',  ( 7.379008025240000102, -59.04182300869999978, -22.22481934930000236 ) ) ;
#28579 = CARTESIAN_POINT ( 'NONE',  ( -12.08593779409999946, -68.40342018370000687, -24.66380339859999893 ) ) ;
#28580 = ADVANCED_FACE ( 'NONE', ( #14538 ), #1305, .T. ) ;
#28581 = CARTESIAN_POINT ( 'NONE',  ( 21.15302165019999947, -58.77396426510000538, 10.53974575699999860 ) ) ;
#28582 = FACE_OUTER_BOUND ( 'NONE', #15230, .T. ) ;
#28583 = ORIENTED_EDGE ( 'NONE', *, *, #4173, .T. ) ;
#28584 = ADVANCED_FACE ( 'NONE', ( #12068 ), #5929, .T. ) ;
#28585 = CARTESIAN_POINT ( 'NONE',  ( 15.59178597810000078, -101.4254868729999970, 3.450949677659999715 ) ) ;
#28586 = CARTESIAN_POINT ( 'NONE',  ( -5.914019803513142826, -97.43430234653058619, 19.69980648870009787 ) ) ;
#28587 = AXIS2_PLACEMENT_3D ( 'NONE', #22987, #11890, #7397 ) ;
#28588 = CARTESIAN_POINT ( 'NONE',  ( 9.734617625879998830E-15, -69.50000000000000000, -46.75000000000000000 ) ) ;
#28589 = CARTESIAN_POINT ( 'NONE',  ( 5.670030758810195692, -92.54383083955174527, -29.96833535579921204 ) ) ;
#28590 = CIRCLE ( 'NONE', #26745, 28.68388914670000034 ) ;
#28591 = LINE ( 'NONE', #26413, #16264 ) ;
#28592 = CARTESIAN_POINT ( 'NONE',  ( 8.096956726469999310, -93.90388142500000868, -24.52623309450000377 ) ) ;
#28593 = DIRECTION ( 'NONE',  ( 0.000000000000000000, 1.000000000000000000, 0.000000000000000000 ) ) ;
#28594 = CARTESIAN_POINT ( 'NONE',  ( -6.853461900220000125, -101.5369810359999860, 14.45809094780000059 ) ) ;
#28595 = ORIENTED_EDGE ( 'NONE', *, *, #7861, .F. ) ;
#28596 = DIRECTION ( 'NONE',  ( 0.000000000000000000, 1.000000000000000000, 0.000000000000000000 ) ) ;
#28597 = CARTESIAN_POINT ( 'NONE',  ( -12.56783578032861115, -100.9616911410483056, -10.74506713166292116 ) ) ;
#28598 = ORIENTED_EDGE ( 'NONE', *, *, #6345, .F. ) ;
#28599 = CARTESIAN_POINT ( 'NONE',  ( 8.229163310540000609, -36.50138226700000388, -21.31937092320000104 ) ) ;
#28600 = CARTESIAN_POINT ( 'NONE',  ( 26.92509574520000015, -92.51556042380001088, -10.07865068210000103 ) ) ;
#28601 = CARTESIAN_POINT ( 'NONE',  ( -1.161294068250000144, -101.3399913430000083, -16.09112164460000116 ) ) ;
#28602 = CARTESIAN_POINT ( 'NONE',  ( 20.33060048479999793, -36.00000012589999443, -9.320855386229998985 ) ) ;
#28603 = CARTESIAN_POINT ( 'NONE',  ( 22.18378897850000442, -19.15825174789999963, 0.3668181516639999473 ) ) ;
#28604 = CARTESIAN_POINT ( 'NONE',  ( -7.135466514619999145, -73.65708014139998738, 38.71640952649999434 ) ) ;
#28605 = CARTESIAN_POINT ( 'NONE',  ( -20.85953344891709449, -92.82668962667167989, -22.25151384493802809 ) ) ;
#28606 = ORIENTED_EDGE ( 'NONE', *, *, #14886, .T. ) ;
#28607 = CARTESIAN_POINT ( 'NONE',  ( -2.131628207279999844E-14, -80.50000000000000000, 1.776356839399999922E-14 ) ) ;
#28608 = CARTESIAN_POINT ( 'NONE',  ( -12.98525885659999979, -18.62004674389999792, 19.04822181160000483 ) ) ;
#28609 = CARTESIAN_POINT ( 'NONE',  ( 16.30128245607246740, -94.65384004866649548, 17.22816601156467087 ) ) ;
#28610 = ADVANCED_FACE ( 'NONE', ( #2847 ), #21193, .F. ) ;
#28611 = CARTESIAN_POINT ( 'NONE',  ( -36.72757213148325661, -65.10974319588410708, -0.1023444634981215962 ) ) ;
#28612 = AXIS2_PLACEMENT_3D ( 'NONE', #19836, #1945, #4260 ) ;
#28613 = DIRECTION ( 'NONE',  ( 0.000000000000000000, -1.000000000000000000, 0.000000000000000000 ) ) ;
#28614 = DIRECTION ( 'NONE',  ( 1.000000000000000000, 0.000000000000000000, 0.000000000000000000 ) ) ;
#28615 = DIRECTION ( 'NONE',  ( 0.000000000000000000, -1.000000000000000000, 0.000000000000000000 ) ) ;
#28616 = ORIENTED_EDGE ( 'NONE', *, *, #22419, .F. ) ;
#28617 = EDGE_CURVE ( 'NONE', #2510, #18068, #20914, .T. ) ;
#28618 = CARTESIAN_POINT ( 'NONE',  ( 8.007516345569998251, -18.50000000000000000, -19.07516293619999814 ) ) ;
#28619 = CARTESIAN_POINT ( 'NONE',  ( 22.06017367829999998, -36.00000000000000000, -10.88627920610000110 ) ) ;
#28620 = ORIENTED_EDGE ( 'NONE', *, *, #11877, .T. ) ;
#28621 = CARTESIAN_POINT ( 'NONE',  ( -1.972916809350000023, -62.77692288639999418, -24.64506619409999999 ) ) ;
#28622 = CARTESIAN_POINT ( 'NONE',  ( -25.65917880860000011, -93.81709628030000658, -2.425942638370000015 ) ) ;
#28623 = CARTESIAN_POINT ( 'NONE',  ( -20.02271108649999576, -55.00753887609999992, 14.43701757890000081 ) ) ;
#28624 = DIRECTION ( 'NONE',  ( 0.9704142011833034598, 0.000000000000000000, -0.2414462220490750377 ) ) ;
#28625 = CIRCLE ( 'NONE', #10015, 29.91857981989999971 ) ;
#28626 = ORIENTED_EDGE ( 'NONE', *, *, #18614, .F. ) ;
#28627 = CARTESIAN_POINT ( 'NONE',  ( 21.38036727909999613, -35.41472438419999946, -7.365645260430000008 ) ) ;
#28628 = CARTESIAN_POINT ( 'NONE',  ( 7.229366192820000592, -73.50064222369999811, -39.23631979990000218 ) ) ;
#28629 = VERTEX_POINT ( 'NONE', #7216 ) ;
#28630 = CARTESIAN_POINT ( 'NONE',  ( 0.000000000000000000, -22.69689110870000093, 0.000000000000000000 ) ) ;
#28631 = CARTESIAN_POINT ( 'NONE',  ( -14.23452928849999921, -80.18504828089999137, 36.64500871850000152 ) ) ;
#28632 = CARTESIAN_POINT ( 'NONE',  ( 21.17154477089999887, -39.34784663159999951, 9.865579592129998687 ) ) ;
#28633 = AXIS2_PLACEMENT_3D ( 'NONE', #18398, #24950, #11962 ) ;
#28634 = DIRECTION ( 'NONE',  ( 0.000000000000000000, 1.000000000000000000, 0.000000000000000000 ) ) ;
#28635 = ADVANCED_FACE ( 'NONE', ( #11710 ), #1765, .T. ) ;
#28636 = CARTESIAN_POINT ( 'NONE',  ( -15.46754588249999962, -101.3256027139999986, 3.711833783079999449 ) ) ;
#28637 = CARTESIAN_POINT ( 'NONE',  ( 7.135467304789999687, -73.50000064450000536, -38.71640881029999548 ) ) ;
#28638 = ORIENTED_EDGE ( 'NONE', *, *, #19091, .F. ) ;
#28639 = CARTESIAN_POINT ( 'NONE',  ( -27.68682485439999752, -36.20000000000000284, -50.68039294919999804 ) ) ;
#28640 = CARTESIAN_POINT ( 'NONE',  ( -12.36870887870000146, -101.2063419769999939, -10.12880706900000050 ) ) ;
#28641 = CARTESIAN_POINT ( 'NONE',  ( -7.135467304789999687, -73.50000064450000536, 38.71640881029999548 ) ) ;
#28642 = CARTESIAN_POINT ( 'NONE',  ( -13.15684669475222535, -99.57060688045895347, -11.33663430084732937 ) ) ;
#28643 = ORIENTED_EDGE ( 'NONE', *, *, #10049, .F. ) ;
#28644 = ADVANCED_FACE ( 'NONE', ( #17956 ), #24092, .T. ) ;
#28645 = CARTESIAN_POINT ( 'NONE',  ( 11.81986579350000000, -72.00000321289999761, -27.35691362350000233 ) ) ;
#28646 = ORIENTED_EDGE ( 'NONE', *, *, #13728, .F. ) ;
#28647 = CARTESIAN_POINT ( 'NONE',  ( 0.000000000000000000, -17.89999999999999858, 0.000000000000000000 ) ) ;
#28648 = FACE_OUTER_BOUND ( 'NONE', #24188, .T. ) ;
#28649 = VERTEX_POINT ( 'NONE', #4405 ) ;
#28650 = CARTESIAN_POINT ( 'NONE',  ( -19.07296793847176275, -97.32367535544746318, 6.861303669024300333 ) ) ;
#28651 = ORIENTED_EDGE ( 'NONE', *, *, #26618, .T. ) ;
#28652 = CARTESIAN_POINT ( 'NONE',  ( 21.78490392830000033, -93.61368451529999390, 12.86422805260000146 ) ) ;
#28653 = CARTESIAN_POINT ( 'NONE',  ( -27.68682485439999752, -24.50000000000000000, -50.68039294919999804 ) ) ;
#28654 = ORIENTED_EDGE ( 'NONE', *, *, #25218, .T. ) ;
#28655 = CARTESIAN_POINT ( 'NONE',  ( -41.86044139887496129, -65.74401284881750485, 1.128482062444109202 ) ) ;
#28656 = PLANE ( 'NONE',  #2965 ) ;
#28657 = B_SPLINE_CURVE_WITH_KNOTS ( 'NONE', 5,
 ( #8237, #17130, #26025, #6046, #14929, #27145, #26704, #22041, #6594 ),
 .UNSPECIFIED., .F., .F.,
 ( 6, 3, 6 ),
 ( 0.000000000000000000, 0.5000000000000000000, 1.000000000000000000 ),
 .UNSPECIFIED. ) ;
#28658 = CARTESIAN_POINT ( 'NONE',  ( 12.45454819569999927, -101.6484611540000031, -10.04451848439999928 ) ) ;
#28659 = CARTESIAN_POINT ( 'NONE',  ( -16.42874499639999897, -93.07154530329999886, -21.42660670609999940 ) ) ;
#28660 = CARTESIAN_POINT ( 'NONE',  ( -7.955258795889999845, -74.00000000000000000, 36.66863921009999672 ) ) ;
#28661 = ORIENTED_EDGE ( 'NONE', *, *, #21870, .T. ) ;
#28662 = CARTESIAN_POINT ( 'NONE',  ( 36.22844186549999534, -74.00000000000000000, -13.75000000000000000 ) ) ;
#28663 = EDGE_CURVE ( 'NONE', #8713, #12443, #8465, .T. ) ;
#28664 = CARTESIAN_POINT ( 'NONE',  ( 12.51978528759999953, -101.0678230150000019, -9.676466934249999596 ) ) ;
#28665 = CARTESIAN_POINT ( 'NONE',  ( -9.348798002780000616, -10.50000000000000000, -17.11285995690000306 ) ) ;
#28666 = CARTESIAN_POINT ( 'NONE',  ( -11.76876535810587043, -94.80026864432733191, -21.40432527480584923 ) ) ;
#28667 = CARTESIAN_POINT ( 'NONE',  ( -34.89999999999999858, -86.00000000000000000, 0.000000000000000000 ) ) ;
#28668 = CARTESIAN_POINT ( 'NONE',  ( 10.24074127443738824, -72.71346136330345189, -26.83295873777677443 ) ) ;
#28669 = CARTESIAN_POINT ( 'NONE',  ( -18.80282716219999983, -18.50000000000000000, 14.71063029340000128 ) ) ;
#28670 = ORIENTED_EDGE ( 'NONE', *, *, #8722, .F. ) ;
#28671 = DIRECTION ( 'NONE',  ( 0.4794255386042036715, 0.000000000000000000, 0.8775825618903724257 ) ) ;
#28672 = B_SPLINE_CURVE_WITH_KNOTS ( 'NONE', 5,
 ( #6540, #19784, #17912, #4355, #24169, #22580, #28666, #8698, #17614 ),
 .UNSPECIFIED., .F., .F.,
 ( 6, 3, 6 ),
 ( 0.000000000000000000, 0.5000000000000000000, 1.000000000000000000 ),
 .UNSPECIFIED. ) ;
#28673 = DIRECTION ( 'NONE',  ( 0.000000000000000000, 1.000000000000000000, 0.000000000000000000 ) ) ;
#28674 = CARTESIAN_POINT ( 'NONE',  ( -0.5413028987460000163, -57.47855601759999900, -23.35488904649999853 ) ) ;
#28675 = CARTESIAN_POINT ( 'NONE',  ( -0.4977272150621083191, -92.58608763743626469, -30.49593994900164162 ) ) ;
#28676 = SHAPE_DEFINITION_REPRESENTATION ( #6176, #26008 ) ;
#28677 = B_SPLINE_CURVE_WITH_KNOTS ( 'NONE', 3,
 ( #9360, #26715, #15764, #2535, #26860, #24963, #18261, #13287, #6900, #11076, #4860, #8912, #13585, #13433, #19993, #22190, #6755, #66, #17967, #24518, #22493, #13738, #15618, #656, #27008, #4555, #2385, #11241, #7195, #7049, #24820, #20147, #4993, #22638, #2678 ),
 .UNSPECIFIED., .F., .F.,
 ( 4, 2, 2, 2, 2, 2, 2, 1, 1, 2, 2, 2, 2, 1, 1, 1, 2, 2, 2, 4 ),
 ( 0.000000000000000000, 0.1249999999999757139, 0.1874999999999635847, 0.2187499999999575062, 0.2499999999999514277, 0.3749999999999258926, 0.4374999999999140687, 0.4687499999999091282, 0.4843749999999067413, 0.4921874999999054645, 0.4999999999999042988, 0.6249999999999072964, 0.6874999999999088507, 0.7187499999999096278, 0.7343749999999100719, 0.7421874999999102940, 0.7460937499999104050, 0.7499999999999105160, 0.8749999999999552580, 1.000000000000000000 ),
 .UNSPECIFIED. ) ;
#28678 = CARTESIAN_POINT ( 'NONE',  ( -4.794255386040000566, -54.00000000000000000, -8.775825618900000791 ) ) ;
#28679 = EDGE_LOOP ( 'NONE', ( #21205, #23744, #13950, #8238, #3219 ) ) ;
#28680 = EDGE_CURVE ( 'NONE', #23314, #6421, #13274, .T. ) ;
#28681 = CARTESIAN_POINT ( 'NONE',  ( 23.54314922829999901, -94.98812769020000246, -6.784139722789999993 ) ) ;
#28682 = ORIENTED_EDGE ( 'NONE', *, *, #27031, .T. ) ;
#28683 = CARTESIAN_POINT ( 'NONE',  ( -12.58874986569999876, -49.85661345660000165, 20.06068440369999806 ) ) ;
#28684 = CARTESIAN_POINT ( 'NONE',  ( 9.270471387543576469, -35.95566652371019956, -19.65325541728526915 ) ) ;
#28685 = ORIENTED_EDGE ( 'NONE', *, *, #11674, .F. ) ;
#28686 = CARTESIAN_POINT ( 'NONE',  ( 30.97095665689999677, -72.00000182920000213, -20.30102787789999752 ) ) ;
#28687 = CARTESIAN_POINT ( 'NONE',  ( -3.375526912685365755, -68.14528050418705618, -27.58514050670897788 ) ) ;
#28688 = CARTESIAN_POINT ( 'NONE',  ( -8.810772439400000877, -95.92349949569999978, -20.47205490330000188 ) ) ;
#28689 = CARTESIAN_POINT ( 'NONE',  ( 8.023929893669999203, -101.0253300669999987, 13.24802822849999906 ) ) ;
#28690 = CARTESIAN_POINT ( 'NONE',  ( -47.25000000000000000, -74.50000000000000000, 3.352534721190000231E-15 ) ) ;
#28691 = CARTESIAN_POINT ( 'NONE',  ( 9.391640714739999396, -49.05622624330000292, -22.99217564430000138 ) ) ;
#28692 = CARTESIAN_POINT ( 'NONE',  ( -29.41500720700000215, -92.50000000000000000, 8.062713625770001613 ) ) ;
#28693 = ORIENTED_EDGE ( 'NONE', *, *, #22511, .T. ) ;
#28694 = CARTESIAN_POINT ( 'NONE',  ( 8.666173000869999754, -92.85282594270000800, -27.14333248820000222 ) ) ;
#28695 = CARTESIAN_POINT ( 'NONE',  ( -50.00000000000000000, -11.00000000000000000, -4.500000000000000000 ) ) ;
#28696 = CARTESIAN_POINT ( 'NONE',  ( -14.13576225364580097, -80.50000169811967510, 36.61638830656482213 ) ) ;
#28697 = CARTESIAN_POINT ( 'NONE',  ( 40.25190969013254971, -74.15297958022469516, 7.245634850467974175 ) ) ;
#28698 = EDGE_LOOP ( 'NONE', ( #8997, #9499, #2761, #9659, #28489 ) ) ;
#28699 = FACE_OUTER_BOUND ( 'NONE', #27780, .T. ) ;
#28700 = CARTESIAN_POINT ( 'NONE',  ( -14.23620810470000109, -92.53807957989999977, 26.01251215649999793 ) ) ;
#28701 = CARTESIAN_POINT ( 'NONE',  ( -14.47984945249999988, -79.50000000000000000, 46.16378133559999952 ) ) ;
#28702 = ORIENTED_EDGE ( 'NONE', *, *, #17104, .F. ) ;
#28703 = AXIS2_PLACEMENT_3D ( 'NONE', #16829, #5184, #23110 ) ;
#28704 = CARTESIAN_POINT ( 'NONE',  ( 27.13959279059999830, -67.66818392540000104, 1.745401794850000021 ) ) ;
#28705 = CARTESIAN_POINT ( 'NONE',  ( 0.6376817541279999890, -100.7833805400000102, -15.89997782040000018 ) ) ;
#28706 = CARTESIAN_POINT ( 'NONE',  ( 24.11566500995067841, -74.16082669357513169, -30.79957691333705938 ) ) ;
#28707 = CARTESIAN_POINT ( 'NONE',  ( 15.76357705000000209, -101.5369810359999860, 2.742715859449999627 ) ) ;
#28708 = CIRCLE ( 'NONE', #14089, 29.91857981989999971 ) ;
#28709 = CARTESIAN_POINT ( 'NONE',  ( -11.02548659089999994, -34.66500525210000205, -19.94550985520000097 ) ) ;
#28710 = VERTEX_POINT ( 'NONE', #13573 ) ;
#28711 = DIRECTION ( 'NONE',  ( 1.000000000000000000, 0.000000000000000000, 0.000000000000000000 ) ) ;
#28712 = LINE ( 'NONE', #10929, #19470 ) ;
#28713 = CIRCLE ( 'NONE', #17565, 0.5000000000000027756 ) ;
#28714 = VERTEX_POINT ( 'NONE', #13128 ) ;
#28715 = EDGE_CURVE ( 'NONE', #19884, #26794, #25878, .T. ) ;
#28716 = CARTESIAN_POINT ( 'NONE',  ( -3.299060192128916658, -18.50000000000001776, -24.39335967336940314 ) ) ;
#28717 = CARTESIAN_POINT ( 'NONE',  ( 15.74335372270872746, -101.5555610555564101, 2.854262349832874079 ) ) ;
#28718 = CARTESIAN_POINT ( 'NONE',  ( -5.553447374120000113, -96.83679384949999758, 20.51777214570000041 ) ) ;
#28719 = ORIENTED_EDGE ( 'NONE', *, *, #2371, .T. ) ;
#28720 = CARTESIAN_POINT ( 'NONE',  ( -19.51835093920258757, -96.93405628829036402, 8.497249192397697826 ) ) ;
#28721 = ADVANCED_FACE ( 'NONE', ( #2221 ), #19982, .T. ) ;
#28722 = AXIS2_PLACEMENT_3D ( 'NONE', #28546, #8582, #17485 ) ;
#28723 = CARTESIAN_POINT ( 'NONE',  ( 20.86759588749999850, -25.49730385779999864, -7.704475033939999662 ) ) ;
#28724 = CARTESIAN_POINT ( 'NONE',  ( -1.604070449259999753, -100.9197075889999979, -15.54198650660000069 ) ) ;
#28725 = CARTESIAN_POINT ( 'NONE',  ( -6.623023768749999540, -101.1411470200000053, 13.89158803029999945 ) ) ;
#28726 = ORIENTED_EDGE ( 'NONE', *, *, #22594, .F. ) ;
#28727 = FACE_OUTER_BOUND ( 'NONE', #25139, .T. ) ;
#28728 = CARTESIAN_POINT ( 'NONE',  ( -12.66900072054220772, -100.7538407675254035, -10.87939260405267738 ) ) ;
#28729 = ORIENTED_EDGE ( 'NONE', *, *, #12711, .T. ) ;
#28730 = CYLINDRICAL_SURFACE ( 'NONE', #3867, 0.9999999999999991118 ) ;
#28731 = EDGE_CURVE ( 'NONE', #13393, #26990, #25971, .T. ) ;
#28732 = ORIENTED_EDGE ( 'NONE', *, *, #25678, .T. ) ;
#28733 = CARTESIAN_POINT ( 'NONE',  ( 7.761187578059999481, -99.03691213880000532, 16.30863471170000167 ) ) ;
#28734 = CARTESIAN_POINT ( 'NONE',  ( 21.33676307760000057, -18.50000000000000000, -0.4490903458859999975 ) ) ;
#28735 = CARTESIAN_POINT ( 'NONE',  ( -43.20000000000000284, -63.07912966450000880, -0.1732050807570000017 ) ) ;
#28736 = B_SPLINE_CURVE_WITH_KNOTS ( 'NONE', 3,
 ( #3436, #16681, #16401, #20791, #27491, #1135, #9836, #10245, #18886, #14227, #12015, #7381, #7807, #14362, #7946, #16833, #27770, #992, #5338, #12159, #16247, #23255, #23116, #27337, #5189, #5473, #844, #16548, #25722, #25585, #5613, #23393, #7542, #3162, #12302, #21343, #14493, #25158, #19020, #5751, #18603, #21074, #14074, #11878, #14638, #23535, #1402, #1264, #27905, #9973, #22976, #21211, #3573, #12430, #3023, #9688, #25310, #20933, #18746 ),
 .UNSPECIFIED., .F., .F.,
 ( 4, 2, 1, 1, 2, 2, 2, 2, 1, 1, 2, 2, 2, 2, 2, 2, 2, 1, 1, 2, 2, 2, 1, 1, 2, 2, 2, 1, 2, 2, 2, 2, 2, 4 ),
 ( 0.000000000000000000, 0.06249999999985383914, 0.09374999999978189669, 0.1093749999997448569, 0.1171874999997315620, 0.1249999999997182809, 0.1874999999995992372, 0.2187499999995454747, 0.2343749999995239919, 0.2421874999995143329, 0.2460937499995147215, 0.2499999999995151101, 0.3124999999997628564, 0.3437499999998855360, 0.3750000000000082712, 0.4375000000002447487, 0.4687500000003571587, 0.4843750000004051759, 0.4921875000004216072, 0.4960937500004218847, 0.5000000000004221068, 0.5625000000003723688, 0.5937500000003522738, 0.6093750000003471667, 0.6171875000003433920, 0.6250000000003395062, 0.6875000000002615685, 0.7187500000002227107, 0.7343750000002021716, 0.7500000000001816325, 0.8125000000001308953, 0.8437500000001064704, 0.8750000000000820455, 1.000000000000000000 ),
 .UNSPECIFIED. ) ;
#28737 = CARTESIAN_POINT ( 'NONE',  ( 0.000000000000000000, -22.69689110870000093, 0.000000000000000000 ) ) ;
#28738 = VECTOR ( 'NONE', #26658, 1000.000000000000000 ) ;
#28739 = CARTESIAN_POINT ( 'NONE',  ( -14.64568764270000045, -101.2530996969999961, 4.044604081960000208 ) ) ;
#28740 = CARTESIAN_POINT ( 'NONE',  ( -8.001416342079998856, -100.4792519539999915, 14.07906887139999874 ) ) ;
#28741 = LINE ( 'NONE', #235, #16472 ) ;
#28742 = B_SPLINE_SURFACE_WITH_KNOTS ( 'NONE', 5, 5, ( 
 ( #9052, #14172, #3112, #2815, #647, #16194 ),
 ( #22925, #5137, #9783, #23203, #16630, #24954 ),
 ( #21023, #20584, #16347, #3249, #9635, #20879 ),
 ( #11521, #18249, #7765, #14017, #25102, #25526 ),
 ( #7327, #2967, #939, #11966, #20428, #11825 ),
 ( #500, #9348, #20738, #13870, #797, #1082 ) ),
 .UNSPECIFIED., .F., .F., .F.,
 ( 6, 6 ),
 ( 6, 6 ),
 ( 26.13957982990000062, 31.08299525729999857 ),
 ( 0.000000000000000000, 2.000000000000000000 ),
 .UNSPECIFIED. ) ;
#28743 = DIRECTION ( 'NONE',  ( 0.000000000000000000, 1.000000000000000000, 0.000000000000000000 ) ) ;
#28744 = CARTESIAN_POINT ( 'NONE',  ( -12.04235212070000216, -66.18149755920001098, -24.32398530919999757 ) ) ;
#28745 = CARTESIAN_POINT ( 'NONE',  ( 19.97576656849999921, -55.50000000000000000, -19.97576656849999921 ) ) ;
#28746 = CARTESIAN_POINT ( 'NONE',  ( 24.74241209330589797, -93.18010901132686286, -14.18012848625775746 ) ) ;
#28747 = CARTESIAN_POINT ( 'NONE',  ( 19.18395247690000360, -26.81058807039999792, -9.003807793969999196 ) ) ;
#28748 = ORIENTED_EDGE ( 'NONE', *, *, #8478, .F. ) ;
#28749 = CARTESIAN_POINT ( 'NONE',  ( 26.22877582859999990, -72.82938648530000592, 11.61106434019999867 ) ) ;
#28750 = AXIS2_PLACEMENT_3D ( 'NONE', #22872, #25481, #16294 ) ;
#28751 = DIRECTION ( 'NONE',  ( 1.000000000000000000, 0.000000000000000000, 0.000000000000000000 ) ) ;
#28752 = CARTESIAN_POINT ( 'NONE',  ( -14.39036416260000095, -64.35840737179999849, 21.98073843050000065 ) ) ;
#28753 = DIRECTION ( 'NONE',  ( 0.000000000000000000, 1.000000000000000000, 0.000000000000000000 ) ) ;
#28754 = AXIS2_PLACEMENT_3D ( 'NONE', #21996, #15715, #20249 ) ;
#28755 = CARTESIAN_POINT ( 'NONE',  ( 9.067410242710000290, -37.66179406690000064, -22.27253134700000103 ) ) ;
#28756 = CARTESIAN_POINT ( 'NONE',  ( -25.14533824960000175, -93.65023553229998754, -2.072119361189999953 ) ) ;
#28757 = ADVANCED_FACE ( 'NONE', ( #20281, #1941 ), #10782, .T. ) ;
#28758 = CARTESIAN_POINT ( 'NONE',  ( -20.19582590579999959, -52.57401960349999825, 14.62459034920000001 ) ) ;
#28759 = DIRECTION ( 'NONE',  ( 1.000000000000000000, 0.000000000000000000, 0.000000000000000000 ) ) ;
#28760 = EDGE_CURVE ( 'NONE', #20241, #8703, #27829, .T. ) ;
#28761 = CARTESIAN_POINT ( 'NONE',  ( 20.29489564980377025, -19.47276819030039618, -8.375690697078448821 ) ) ;
#28762 = CARTESIAN_POINT ( 'NONE',  ( 16.03799742140000006, -100.8746138070000029, 4.294561568749999836 ) ) ;
#28763 = ORIENTED_EDGE ( 'NONE', *, *, #1222, .F. ) ;
#28764 =( NAMED_UNIT ( * ) PLANE_ANGLE_UNIT ( ) SI_UNIT ( $, .RADIAN. ) );
#28765 = CARTESIAN_POINT ( 'NONE',  ( 7.283540599140000182, -74.14144493730000818, -39.92825895720000062 ) ) ;
#28766 = ORIENTED_EDGE ( 'NONE', *, *, #4069, .F. ) ;
#28767 = EDGE_CURVE ( 'NONE', #10513, #28649, #28261, .T. ) ;
#28768 = CARTESIAN_POINT ( 'NONE',  ( -40.70731707320000226, -84.00000000000000000, -7.215414233289999757 ) ) ;
#28769 = EDGE_CURVE ( 'NONE', #19738, #20825, #16195, .T. ) ;
#28770 = CARTESIAN_POINT ( 'NONE',  ( 0.5880502493170355338, -99.62767017963351179, -17.32703895575575004 ) ) ;
#28771 = CIRCLE ( 'NONE', #3666, 0.4999999999999982236 ) ;
#28772 = CARTESIAN_POINT ( 'NONE',  ( -10.39027439690000065, -18.50000000000000000, -18.36289120799999708 ) ) ;
#28773 = CARTESIAN_POINT ( 'NONE',  ( 19.97576656849999921, -18.50000000000000000, -19.97576656849999921 ) ) ;
#28774 = CARTESIAN_POINT ( 'NONE',  ( 24.36857893470000036, -92.99570653130000153, -11.25322410160000075 ) ) ;
#28775 = PLANE ( 'NONE',  #2981 ) ;
#28776 = DIRECTION ( 'NONE',  ( 0.000000000000000000, -1.000000000000000000, 0.000000000000000000 ) ) ;
#28777 = CARTESIAN_POINT ( 'NONE',  ( 14.31067114689999897, -98.53908914310000000, -12.11010054220000143 ) ) ;
#28778 = ORIENTED_EDGE ( 'NONE', *, *, #26164, .T. ) ;
#28779 = CARTESIAN_POINT ( 'NONE',  ( -15.44795072159999982, -101.4309506800000094, 4.757508573860000034 ) ) ;
#28780 = DIRECTION ( 'NONE',  ( -0.8775825618903722036, 0.000000000000000000, 0.4794255386042041156 ) ) ;
#28781 = FACE_OUTER_BOUND ( 'NONE', #26256, .T. ) ;
#28782 = DIRECTION ( 'NONE',  ( 0.09756097560976760563, 0.000000000000000000, 0.9952295494196654602 ) ) ;
#28783 = CARTESIAN_POINT ( 'NONE',  ( -13.28489450998225685, -99.84800943042500876, -11.12833488179714081 ) ) ;
#28784 = ORIENTED_EDGE ( 'NONE', *, *, #24311, .F. ) ;
#28785 = VECTOR ( 'NONE', #25549, 1000.000000000000000 ) ;
#28786 = FACE_BOUND ( 'NONE', #4015, .T. ) ;
#28787 = CARTESIAN_POINT ( 'NONE',  ( 36.82078951440000480, -80.19526215299998739, -13.76146197529999959 ) ) ;
#28788 = ORIENTED_EDGE ( 'NONE', *, *, #16653, .F. ) ;
#28789 = CIRCLE ( 'NONE', #18601, 3.750000000000000000 ) ;
#28790 = AXIS2_PLACEMENT_3D ( 'NONE', #26628, #8549, #17451 ) ;
#28791 = CIRCLE ( 'NONE', #23691, 29.91857981989999971 ) ;
#28792 = DIRECTION ( 'NONE',  ( 1.000000000000000000, 0.000000000000000000, 0.000000000000000000 ) ) ;
#28793 = DIRECTION ( 'NONE',  ( 0.4794255386042042266, 0.000000000000000000, 0.8775825618903720926 ) ) ;
#28794 = CARTESIAN_POINT ( 'NONE',  ( -0.5413028987460000163, -57.47855601759999900, -23.35488904649999853 ) ) ;
#28795 = ORIENTED_EDGE ( 'NONE', *, *, #7604, .F. ) ;
#28796 = ADVANCED_FACE ( 'NONE', ( #4256 ), #6743, .T. ) ;
#28797 = DIRECTION ( 'NONE',  ( 0.4794255386042040601, 0.000000000000000000, 0.8775825618903719816 ) ) ;
#28798 = CARTESIAN_POINT ( 'NONE',  ( -19.25397897833660821, -97.06701639843478802, 7.326875019138189948 ) ) ;
#28799 = ORIENTED_EDGE ( 'NONE', *, *, #23398, .T. ) ;
#28800 = CARTESIAN_POINT ( 'NONE',  ( 25.83673624310000250, -92.67327661130001104, 10.43148741010000080 ) ) ;
#28801 = CARTESIAN_POINT ( 'NONE',  ( -40.00000000000000000, -69.50000000000000000, 1.332267629549999902E-15 ) ) ;
#28802 = CARTESIAN_POINT ( 'NONE',  ( 36.22844186549999534, -74.00000000000000000, -13.75000000000000000 ) ) ;
#28803 = NEXT_ASSEMBLY_USAGE_OCCURRENCE ( 'NAUO1', ' ', ' ', #11298, #121, $ ) ;
#28804 = NEXT_ASSEMBLY_USAGE_OCCURRENCE ( 'NAUO2', ' ', ' ', #11298, #10742, $ ) ;
#28805 = NEXT_ASSEMBLY_USAGE_OCCURRENCE ( 'NAUO3', ' ', ' ', #11298, #4003, $ ) ;
#28806 = NEXT_ASSEMBLY_USAGE_OCCURRENCE ( 'NAUO4', ' ', ' ', #11298, #26287, $ ) ;
#28807 = NEXT_ASSEMBLY_USAGE_OCCURRENCE ( 'NAUO5', ' ', ' ', #11298, #1029, $ ) ;
#28808 = NEXT_ASSEMBLY_USAGE_OCCURRENCE ( 'NAUO6', ' ', ' ', #11298, #28060, $ ) ;
#28809 = NEXT_ASSEMBLY_USAGE_OCCURRENCE ( 'NAUO7', ' ', ' ', #11298, #121, $ ) ;
#28810 = NEXT_ASSEMBLY_USAGE_OCCURRENCE ( 'NAUO8', ' ', ' ', #11298, #121, $ ) ;
#28811 = NEXT_ASSEMBLY_USAGE_OCCURRENCE ( 'NAUO9', ' ', ' ', #11298, #121, $ ) ;
ENDSEC;
END-ISO-10303-21;
